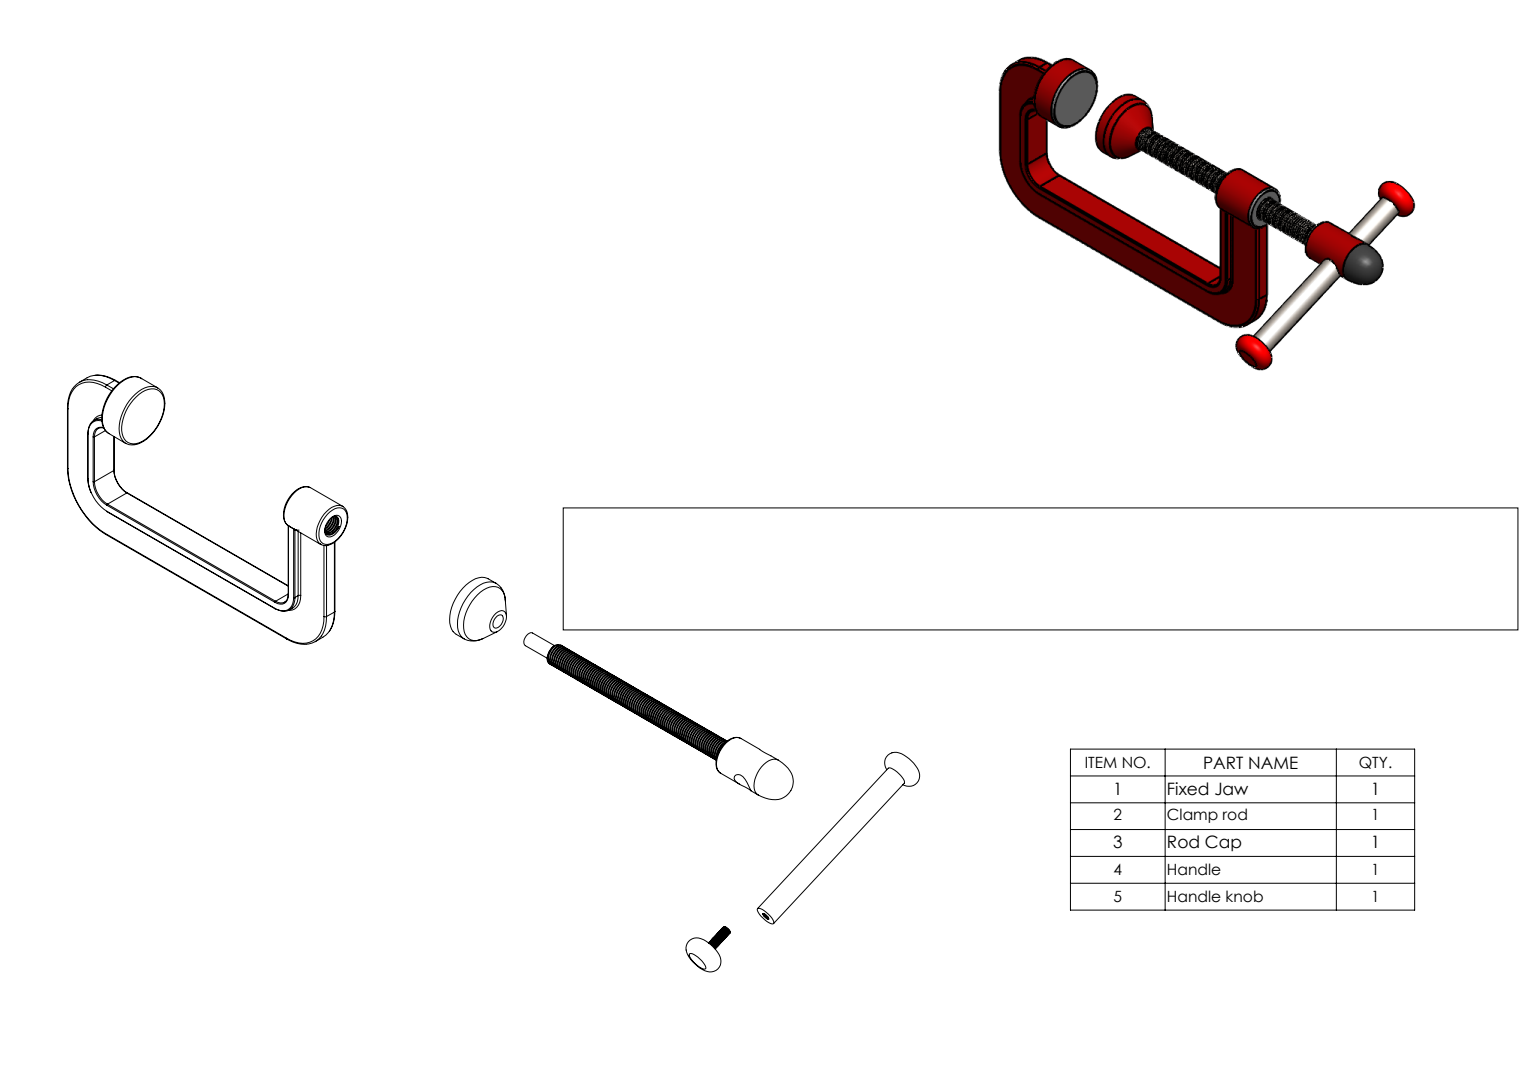
ISO-10303-21;
HEADER;
FILE_DESCRIPTION (('STEP AP214'),
    '1' );
FILE_NAME ('MAS-675',
    '2026-10-07T06:38:26',
    ( '' ),
    ( '' ),
    'SwSTEP 2.0',
    'SolidWorks 2021',
    '' );
FILE_SCHEMA (( 'AUTOMOTIVE_DESIGN' ));
ENDSEC;

DATA;
#1 = VERTEX_POINT ( 'NONE', #13580 ) ;
#2 = ORIENTED_EDGE ( 'NONE', *, *, #13115, .T. ) ;
#3 = CARTESIAN_POINT ( 'NONE',  ( 151.8675748654052029, -5.500000000000012434, 2.278174593052012309 ) ) ;
#4 = CARTESIAN_POINT ( 'NONE',  ( 134.2500000000000284, -6.000000000000005329, 0.000000000000000000 ) ) ;
#5 = ORIENTED_EDGE ( 'NONE', *, *, #19399, .F. ) ;
#6 = CARTESIAN_POINT ( 'NONE',  ( -5.412658773652684552, -3.125000000000099920, -143.0669872981078470 ) ) ;
#7 =( NAMED_UNIT ( * ) PLANE_ANGLE_UNIT ( ) SI_UNIT ( $, .RADIAN. ) );
#8 = CARTESIAN_POINT ( 'NONE',  ( 11.81249999999999822, -2.649519052838298805, 1.097466725451559322 ) ) ;
#9 = ADVANCED_FACE ( 'NONE', ( #19589 ), #12972, .F. ) ;
#10 = CARTESIAN_POINT ( 'NONE',  ( 5.999999999999999112, 2.951592740943527306E-14, -151.5863248654052029 ) ) ;
#11 = VECTOR ( 'NONE', #10192, 1000.000000000000000 ) ;
#12 = CARTESIAN_POINT ( 'NONE',  ( 18.18750000000005684, 0.8284271247463557142, 1.999999999999971800 ) ) ;
#13 = CARTESIAN_POINT ( 'NONE',  ( 3.464101615137757051, -5.999999999999979572, -171.3363248654052029 ) ) ;
#14 = CARTESIAN_POINT ( 'NONE',  ( 116.0000000000000142, 6.735557395310442023E-16, 5.500000000000000000 ) ) ;
#15 = CARTESIAN_POINT ( 'NONE',  ( -5.412658773652739619, 3.124999999999975131, -63.18301270189225249 ) ) ;
#16 = CARTESIAN_POINT ( 'NONE',  ( -5.999999999999963585, 1.780251999655701777E-13, -110.9136751345948255 ) ) ;
#17 = CARTESIAN_POINT ( 'NONE',  ( 143.2351497308104058, 3.535533905932725318, -3.535533905932725318 ) ) ;
#18 = DIRECTION ( 'NONE',  ( 1.000000000000000000, -5.551115123125774074E-17, 0.000000000000000000 ) ) ;
#19 = DIRECTION ( 'NONE',  ( -0.000000000000000000, -0.000000000000000000, -1.000000000000000000 ) ) ;
#20 = LINE ( 'NONE', #9560, #12153 ) ;
#21 = CYLINDRICAL_SURFACE ( 'NONE', #16144, 11.00000000000001599 ) ;
#22 = CARTESIAN_POINT ( 'NONE',  ( 112.1249999999998437, 1.767766952966293159, 1.767766952966431937 ) ) ;
#23 = EDGE_CURVE ( 'NONE', #18475, #14303, #3726, .T. ) ;
#24 = CARTESIAN_POINT ( 'NONE',  ( 15.64882486540532547, 2.500000000000084821, -1.035533905932929599 ) ) ;
#25 = DIRECTION ( 'NONE',  ( 0.000000000000000000, 0.000000000000000000, -1.000000000000000000 ) ) ;
#26 = EDGE_LOOP ( 'NONE', ( #21447, #18277, #20127, #3460 ) ) ;
#27 = CARTESIAN_POINT ( 'NONE',  ( -6.350852961085760029, -1.281975124255709124E-13, -55.12500000000003553 ) ) ;
#28 = DIRECTION ( 'NONE',  ( 1.000000000000000000, 0.000000000000000000, 0.000000000000000000 ) ) ;
#29 = CARTESIAN_POINT ( 'NONE',  ( 6.000000000000000888, -1.859271017917181981E-14, -167.1636751345948255 ) ) ;
#30 = CARTESIAN_POINT ( 'NONE',  ( -3.464101615137757051, -5.999999999999979572, -179.0863248654052313 ) ) ;
#31 = ORIENTED_EDGE ( 'NONE', *, *, #1535, .F. ) ;
#32 = CARTESIAN_POINT ( 'NONE',  ( 104.9374999999997726, 2.500000000000114575, -1.035533905932448873 ) ) ;
#33 = CARTESIAN_POINT ( 'NONE',  ( 142.6875000000000284, 4.242640687119269671, 4.242640687119298093 ) ) ;
#34 = CARTESIAN_POINT ( 'NONE',  ( -3.608439182435052128, -6.250000000000110134, -103.9419872981078328 ) ) ;
#35 = MECHANICAL_DESIGN_GEOMETRIC_PRESENTATION_REPRESENTATION (  '', ( #14770 ), #26040 ) ;
#36 = CARTESIAN_POINT ( 'NONE',  ( -3.464101615137725076, 5.999999999999979572, -176.5863248654052313 ) ) ;
#37 = VECTOR ( 'NONE', #4562, 1000.000000000000000 ) ;
#38 = CARTESIAN_POINT ( 'NONE',  ( 160.5788997308103774, -4.999999999999989342, 2.071067811865468400 ) ) ;
#39 = CARTESIAN_POINT ( 'NONE',  ( 118.3749999999999147, -1.767766952966293159, 1.767766952966431937 ) ) ;
#40 = CARTESIAN_POINT ( 'NONE',  ( 3.175426480543072749, -5.500000000000105693, -138.6250000000000568 ) ) ;
#41 = VECTOR ( 'NONE', #11597, 1000.000000000000000 ) ;
#42 = VERTEX_POINT ( 'NONE', #1381 ) ;
#43 = VECTOR ( 'NONE', #27184, 1000.000000000000000 ) ;
#44 = ORIENTED_EDGE ( 'NONE', *, *, #20112, .T. ) ;
#45 =( NAMED_UNIT ( * ) PLANE_ANGLE_UNIT ( ) SI_UNIT ( $, .RADIAN. ) );
#46 = EDGE_CURVE ( 'NONE', #22177, #19788, #18313, .T. ) ;
#47 = CARTESIAN_POINT ( 'NONE',  ( -3.175426480542816510, -5.500000000000057732, -66.87500000000002842 ) ) ;
#48 = CARTESIAN_POINT ( 'NONE',  ( 0.000000000000000000, -5.999999999999991118, -81.46132486540524553 ) ) ;
#49 = CARTESIAN_POINT ( 'NONE',  ( 159.6411875853270885, -12.17723633016814233, -3.777793391642500165 ) ) ;
#50 = CARTESIAN_POINT ( 'NONE',  ( 3.608439182435180470, 6.249999999999982236, -80.05801270189219565 ) ) ;
#51 = CARTESIAN_POINT ( 'NONE',  ( 5.196152422706629359, 3.000000000000002665, -140.0386751345948255 ) ) ;
#52 = CARTESIAN_POINT ( 'NONE',  ( 106.7497167782375129, 1.308140751793612777, 1.308140751793529510 ) ) ;
#53 = DIRECTION ( 'NONE',  ( -1.000000000000000000, -0.000000000000000000, -0.000000000000000000 ) ) ;
#54 = VECTOR ( 'NONE', #17424, 1000.000000000000000 ) ;
#55 = CARTESIAN_POINT ( 'NONE',  ( 119.3127832217621034, 1.849990392679501827, -0.7662911109077087390 ) ) ;
#56 = ADVANCED_FACE ( 'NONE', ( #10625 ), #5822, .T. ) ;
#57 = CONTEXT_DEPENDENT_SHAPE_REPRESENTATION ( #15191, #20980 ) ;
#58 =( BOUNDED_CURVE ( )  B_SPLINE_CURVE ( 2, ( #3111, #10057, #5114, #12242, #12386, #512, #17135, #26164, #2819 ),
 .UNSPECIFIED., .F., .T. ) 
 B_SPLINE_CURVE_WITH_KNOTS ( ( 3, 2, 2, 2, 3 ),
 ( 0.05277777777777781232, 0.05370370370370369795, 0.05555555555555558023, 0.05740740740740746251, 0.05833333333333334814 ),
 .UNSPECIFIED. ) 
 CURVE ( )  GEOMETRIC_REPRESENTATION_ITEM ( )  RATIONAL_B_SPLINE_CURVE ( ( 0.9330127018922194093, 0.9330127018922234061, 1.000000000000000000, 0.8660254037844388186, 1.000000000000000000, 0.8660254037844388186, 1.000000000000000000, 0.9330127018922194093, 0.9330127018922194093 ) ) 
 REPRESENTATION_ITEM ( '' )  );
#59 = CARTESIAN_POINT ( 'NONE',  ( 4.763139720814407951, -2.749999999999988454, -149.0000000000000284 ) ) ;
#60 = CARTESIAN_POINT ( 'NONE',  ( 139.5760635317500089, -9.165151396444613852, -8.000000000000007105 ) ) ;
#61 = CARTESIAN_POINT ( 'NONE',  ( 3.175426480543072749, -5.500000000000105693, -138.6250000000000568 ) ) ;
#62 = CARTESIAN_POINT ( 'NONE',  ( 3.608439182435180470, 6.249999999999982236, -164.0580127018922383 ) ) ;
#63 = CARTESIAN_POINT ( 'NONE',  ( 0.000000000000000000, -5.999999999999991118, -148.9613248654052597 ) ) ;
#64 = DIRECTION ( 'NONE',  ( 6.938893903907222067E-15, 1.000000000000000000, 0.000000000000000000 ) ) ;
#65 = CARTESIAN_POINT ( 'NONE',  ( 6.350852961086080661, -9.614813431917819062E-14, -76.87500000000002842 ) ) ;
#66 = FILL_AREA_STYLE ('',( #23440 ) ) ;
#67 = CARTESIAN_POINT ( 'NONE',  ( -4.763139720814407951, 2.749999999999946709, -62.75000000000002842 ) ) ;
#68 = CARTESIAN_POINT ( 'NONE',  ( -5.196152422706601826, 2.999999999999975131, -154.5386751345948539 ) ) ;
#69 = CARTESIAN_POINT ( 'NONE',  ( 145.1398502691896510, -3.535533905932752852, 3.535533905932725318 ) ) ;
#70 = CARTESIAN_POINT ( 'NONE',  ( 3.464101615137757051, -5.999999999999979572, -114.3363248654051745 ) ) ;
#71 = CARTESIAN_POINT ( 'NONE',  ( -5.196152422706573404, -3.000000000000002665, -144.7113248654052313 ) ) ;
#72 = CARTESIAN_POINT ( 'NONE',  ( 157.4062500000000284, 6.000000000000005329, -2.485281374238556218 ) ) ;
#73 = DIRECTION ( 'NONE',  ( 5.551115123125785167E-17, -1.000000000000000000, -8.881784197001256268E-16 ) ) ;
#74 = CARTESIAN_POINT ( 'NONE',  ( -3.464101615137757051, -5.999999999999979572, -50.08632486540522422 ) ) ;
#75 = CARTESIAN_POINT ( 'NONE',  ( 6.000000000000000888, -3.330669073875464691E-16, -7.560779664488942560E-35 ) ) ;
#76 = CARTESIAN_POINT ( 'NONE',  ( 116.5622167782374135, 1.849990392679562001, -0.7662911109077087390 ) ) ;
#77 = DIRECTION ( 'NONE',  ( 1.000000000000000000, 0.000000000000000000, 0.000000000000000000 ) ) ;
#78 = ORIENTED_EDGE ( 'NONE', *, *, #7844, .T. ) ;
#79 = CARTESIAN_POINT ( 'NONE',  ( 150.3750000000000284, 0.000000000000000000, 6.000000000000005329 ) ) ;
#80 = SURFACE_SIDE_STYLE ('',( #6693 ) ) ;
#81 = CARTESIAN_POINT ( 'NONE',  ( 115.7502832217623308, -1.308140751793585022, 1.308140751793640533 ) ) ;
#82 = CARTESIAN_POINT ( 'NONE',  ( -3.464101615137757051, -5.999999999999979572, -85.16367513459481131 ) ) ;
#83 = ORIENTED_EDGE ( 'NONE', *, *, #26629, .F. ) ;
#84 = VERTEX_POINT ( 'NONE', #7829 ) ;
#85 = CARTESIAN_POINT ( 'NONE',  ( 19.25000000000009948, 1.110223024625156540E-13, 1.999999999999946265 ) ) ;
#86 = VECTOR ( 'NONE', #24008, 1000.000000000000114 ) ;
#87 = VERTEX_POINT ( 'NONE', #29166 ) ;
#88 = EDGE_CURVE ( 'NONE', #16343, #27983, #2946, .T. ) ;
#89 = CARTESIAN_POINT ( 'NONE',  ( -6.350852961085760029, -1.281975124255709124E-13, -91.12500000000001421 ) ) ;
#90 = CARTESIAN_POINT ( 'NONE',  ( -7.216878364870328078, 0.000000000000000000, -106.5580127018922525 ) ) ;
#91 = VERTEX_POINT ( 'NONE', #21836 ) ;
#92 = CARTESIAN_POINT ( 'NONE',  ( 5.959413262067462469, 9.246315551493085039, -24.19612909832622449 ) ) ;
#93 = CARTESIAN_POINT ( 'NONE',  ( 156.4538997308104626, -2.071067811865468400, -4.999999999999989342 ) ) ;
#94 = CIRCLE ( 'NONE', #6471, 2.000000000000003109 ) ;
#95 = CARTESIAN_POINT ( 'NONE',  ( 3.464101615137757051, -5.999999999999979572, -63.33632486540521711 ) ) ;
#96 = CARTESIAN_POINT ( 'NONE',  ( 135.6737246954180023, -8.728829995094853800, 8.172675940893835644 ) ) ;
#97 = ADVANCED_FACE ( 'NONE', ( #784 ), #22288, .T. ) ;
#98 = ADVANCED_FACE ( 'NONE', ( #17543 ), #26707, .F. ) ;
#99 = CARTESIAN_POINT ( 'NONE',  ( 4.763139720814407951, 2.750000000000002665, -169.7500000000000000 ) ) ;
#100 = CARTESIAN_POINT ( 'NONE',  ( 23.03867513459492855, 2.220446049250313081E-13, -2.500000000000057732 ) ) ;
#101 = STYLED_ITEM ( 'NONE', ( #7132 ), #3790 ) ;
#102 = CARTESIAN_POINT ( 'NONE',  ( -4.763139720814407951, 2.749999999999946709, -151.2500000000000000 ) ) ;
#103 = SHAPE_REPRESENTATION ( 'MAS-675', ( #12959, #2139, #10996, #7044, #27128, #21262 ), #2611 ) ;
#104 = CARTESIAN_POINT ( 'NONE',  ( 112.4374999999998010, -2.499999999999934719, 1.035533905932989551 ) ) ;
#105 = AXIS2_PLACEMENT_3D ( 'NONE', #8951, #27958, #28266 ) ;
#106 = CARTESIAN_POINT ( 'NONE',  ( -2.775557561562891351E-14, -5.500000000000115463, -101.2500000000000000 ) ) ;
#107 = CARTESIAN_POINT ( 'NONE',  ( 135.0000000000000284, -54.99999999999993605, -7.500000000000007105 ) ) ;
#108 = CARTESIAN_POINT ( 'NONE',  ( 125.0000000000000568, -55.00000000000000711, -7.500000000000007105 ) ) ;
#110 = CARTESIAN_POINT ( 'NONE',  ( -3.175426480542816510, 5.499999999999865885, -86.87500000000007105 ) ) ;
#109 = CARTESIAN_POINT ( 'NONE',  ( 3.175426480543072749, 5.499999999999865885, -154.6250000000000853 ) ) ;
#111 = CARTESIAN_POINT ( 'NONE',  ( 161.5461002691896226, -2.071067811865468400, 4.999999999999989342 ) ) ;
#112 = CARTESIAN_POINT ( 'NONE',  ( 0.7724517649218355375, -15.49026069396310490, 8.142614232235679594 ) ) ;
#113 = ORIENTED_EDGE ( 'NONE', *, *, #22581, .F. ) ;
#114 = CARTESIAN_POINT ( 'NONE',  ( 9.937500000000083489, -1.097466725451379244, 2.649519052838238409 ) ) ;
#115 = UNCERTAINTY_MEASURE_WITH_UNIT (LENGTH_MEASURE( 1.000000000000000082E-05 ), #12056, 'distance_accuracy_value', 'NONE');
#116 = CARTESIAN_POINT ( 'NONE',  ( 114.5624999999997442, -2.499999999999934719, -1.035533905932448873 ) ) ;
#117 = CARTESIAN_POINT ( 'NONE',  ( -4.999999999999990230, -55.00000000000002132, 5.000000000000004441 ) ) ;
#118 = CARTESIAN_POINT ( 'NONE',  ( 106.5627832217621602, 0.7662911109078588412, 1.849990392679712103 ) ) ;
#119 = CARTESIAN_POINT ( 'NONE',  ( 23.66367513459491434, -1.767766952966209892, 1.767766952966376426 ) ) ;
#120 = ORIENTED_EDGE ( 'NONE', *, *, #127, .F. ) ;
#121 = DIRECTION ( 'NONE',  ( 0.000000000000000000, 0.000000000000000000, -1.000000000000000000 ) ) ;
#122 = DIRECTION ( 'NONE',  ( -7.147005652999508048E-36, 5.642372883946980038E-36, 1.000000000000000000 ) ) ;
#123 = ORIENTED_EDGE ( 'NONE', *, *, #24115, .F. ) ;
#124 = VERTEX_POINT ( 'NONE', #14929 ) ;
#125 = CARTESIAN_POINT ( 'NONE',  ( 151.9687500000000568, -2.485281374238585972, 6.000000000000005329 ) ) ;
#126 = ORIENTED_EDGE ( 'NONE', *, *, #11372, .T. ) ;
#127 = EDGE_CURVE ( 'NONE', #21812, #1827, #10033, .T. ) ;
#128 = CARTESIAN_POINT ( 'NONE',  ( 4.763139720814407951, -2.749999999999988454, -109.9999999999999858 ) ) ;
#129 = CARTESIAN_POINT ( 'NONE',  ( 21.62500000000011724, 1.110223024625156540E-13, 2.649519052838167354 ) ) ;
#130 = CARTESIAN_POINT ( 'NONE',  ( 3.175426480543072749, -5.500000000000105693, -150.6250000000000284 ) ) ;
#131 = CARTESIAN_POINT ( 'NONE',  ( -5.412658773652684552, -3.125000000000099920, -130.4330127018922383 ) ) ;
#132 = ORIENTED_EDGE ( 'NONE', *, *, #22296, .F. ) ;
#133 = CARTESIAN_POINT ( 'NONE',  ( 0.000000000000000000, 0.000000000000000000, 0.000000000000000000 ) ) ;
#134 = CARTESIAN_POINT ( 'NONE',  ( 3.608439182435180470, -6.249999999999997335, -171.1919872981078470 ) ) ;
#135 = CARTESIAN_POINT ( 'NONE',  ( 107.1249999999998437, 1.767766952966265404, 1.767766952966320915 ) ) ;
#136 = CARTESIAN_POINT ( 'NONE',  ( 134.2351497308104058, 3.535533905932725318, -3.535533905932725318 ) ) ;
#137 = VERTEX_POINT ( 'NONE', #1215 ) ;
#138 = CARTESIAN_POINT ( 'NONE',  ( 0.1879814459054835185, -15.40071801525260220, -8.313003687118166951 ) ) ;
#139 = ADVANCED_FACE ( 'NONE', ( #915 ), #19679, .F. ) ;
#140 = COLOUR_RGB ( '', 0.31764706, 0.68627451, 0.89019608) ;
#141 = CARTESIAN_POINT ( 'NONE',  ( -3.464101615137725076, 5.999999999999979572, -95.58632486540524553 ) ) ;
#142 = CYLINDRICAL_SURFACE ( 'NONE', #25085, 0.5000000000000004441 ) ;
#143 = CARTESIAN_POINT ( 'NONE',  ( -2.775557561562891351E-14, -5.500000000000115463, -180.7500000000000284 ) ) ;
#144 = CARTESIAN_POINT ( 'NONE',  ( 108.6877832217621318, -0.7662911109077388261, 1.849990392679712103 ) ) ;
#145 = CARTESIAN_POINT ( 'NONE',  ( -5.412658773652739619, 3.124999999999975131, -178.6830127018922383 ) ) ;
#146 = CARTESIAN_POINT ( 'NONE',  ( -0.5130136762305975706, -9.973972647538804637, -4.738252045315842764 ) ) ;
#147 = CARTESIAN_POINT ( 'NONE',  ( 159.9897649647779474, -11.17313463120727057, -4.377898023955410167 ) ) ;
#148 = UNCERTAINTY_MEASURE_WITH_UNIT (LENGTH_MEASURE( 1.000000000000000082E-05 ), #22122, 'distance_accuracy_value', 'NONE');
#149 = CARTESIAN_POINT ( 'NONE',  ( -6.350852961085760029, -1.281975124255709124E-13, -113.6249999999999858 ) ) ;
#150 = CARTESIAN_POINT ( 'NONE',  ( 135.0000000000000284, -8.662311887307041047, -7.546725650337192448 ) ) ;
#151 = CARTESIAN_POINT ( 'NONE',  ( 154.1175748654052313, 5.500000000000012434, -2.278174593052012309 ) ) ;
#152 = VERTEX_POINT ( 'NONE', #29328 ) ;
#153 = CARTESIAN_POINT ( 'NONE',  ( 21.25000000000013145, -1.873492889144845464, -1.873492889145178530 ) ) ;
#154 = DIRECTION ( 'NONE',  ( -7.147005652999508048E-36, 5.642372883946980038E-36, 1.000000000000000000 ) ) ;
#155 = CARTESIAN_POINT ( 'NONE',  ( 6.000000000000000888, 1.607695154586715303, -168.5966878364870354 ) ) ;
#156 = CARTESIAN_POINT ( 'NONE',  ( 5.196152422706629359, 3.000000000000002665, -131.9613248654052313 ) ) ;
#157 =( BOUNDED_CURVE ( )  B_SPLINE_CURVE ( 2, ( #10782, #15865, #1831, #11235, #29931, #22280, #26855, #27319, #5814 ),
 .UNSPECIFIED., .F., .T. ) 
 B_SPLINE_CURVE_WITH_KNOTS ( ( 3, 2, 2, 2, 3 ),
 ( 0.6750000000000000444, 0.6759259259259259300, 0.6777777777777778123, 0.6796296296296295836, 0.6805555555555554692 ),
 .UNSPECIFIED. ) 
 CURVE ( )  GEOMETRIC_REPRESENTATION_ITEM ( )  RATIONAL_B_SPLINE_CURVE ( ( 0.9330127018922194093, 0.9330127018922234061, 1.000000000000000000, 0.8660254037844388186, 1.000000000000000000, 0.8660254037844388186, 1.000000000000000000, 0.9330127018922234061, 0.9330127018922194093 ) ) 
 REPRESENTATION_ITEM ( '' )  );
#158 = AXIS2_PLACEMENT_3D ( 'NONE', #25640, #4289, #30093 ) ;
#159 = EDGE_LOOP ( 'NONE', ( #11290, #9356, #28132, #17982 ) ) ;
#160 = CARTESIAN_POINT ( 'NONE',  ( 118.4613248654051034, 1.110223024625156540E-13, -2.000000000000001776 ) ) ;
#161 = CARTESIAN_POINT ( 'NONE',  ( 22.21132486540528106, -2.499999999999780176, -1.110223024625156540E-13 ) ) ;
#162 = CARTESIAN_POINT ( 'NONE',  ( 142.5863248654052313, 0.000000000000000000, 5.500000000000005329 ) ) ;
#163 = CARTESIAN_POINT ( 'NONE',  ( 113.2113248654051034, -1.999999999999918510, 1.110223024625156540E-13 ) ) ;
#164 = ORIENTED_EDGE ( 'NONE', *, *, #27531, .F. ) ;
#165 = ORIENTED_EDGE ( 'NONE', *, *, #8341, .F. ) ;
#166 = CARTESIAN_POINT ( 'NONE',  ( 20.85117513459493921, -2.499999999999844569, -1.035533905932809473 ) ) ;
#167 = CARTESIAN_POINT ( 'NONE',  ( 135.1875000000000568, 4.242640687119269671, 4.242640687119298093 ) ) ;
#168 = EDGE_CURVE ( 'NONE', #2390, #1119, #5990, .T. ) ;
#169 = ADVANCED_FACE ( 'NONE', ( #22749 ), #29791, .T. ) ;
#170 = CARTESIAN_POINT ( 'NONE',  ( 3.608439182435180470, -6.249999999999997335, -141.1919872981078186 ) ) ;
#171 = CARTESIAN_POINT ( 'NONE',  ( -4.999999999999920952, -65.50000000000001421, -8.000000000000007105 ) ) ;
#172 =( NAMED_UNIT ( * ) PLANE_ANGLE_UNIT ( ) SI_UNIT ( $, .RADIAN. ) );
#173 = CARTESIAN_POINT ( 'NONE',  ( 19.75000000000009948, 1.665334536937734811E-13, -2.000000000000001776 ) ) ;
#174 = CARTESIAN_POINT ( 'NONE',  ( 117.7261751345945413, -1.999999999999971800, 0.8284271247464157772 ) ) ;
#175 = CIRCLE ( 'NONE', #14898, 0.5000000000000004441 ) ;
#176 = CARTESIAN_POINT ( 'NONE',  ( 144.5476497308104058, 0.000000000000000000, -5.000000000000004441 ) ) ;
#177 = CYLINDRICAL_SURFACE ( 'NONE', #16338, 6.000000000000000888 ) ;
#178 = CARTESIAN_POINT ( 'NONE',  ( 13.03867513459488947, 5.551115123125782702E-14, -2.500000000000002220 ) ) ;
#179 = CARTESIAN_POINT ( 'NONE',  ( 3.464101615137852974, 5.999999999999884537, -146.8363248654052313 ) ) ;
#180 = AXIS2_PLACEMENT_3D ( 'NONE', #24945, #8684, #29090 ) ;
#181 = CARTESIAN_POINT ( 'NONE',  ( 114.2886751345947971, 2.000000000000029310, 1.110223024625156540E-13 ) ) ;
#182 = CARTESIAN_POINT ( 'NONE',  ( 110.6249999999998437, -1.767766952966376426, -1.767766952966320915 ) ) ;
#183 = ORIENTED_EDGE ( 'NONE', *, *, #15487, .T. ) ;
#184 = CARTESIAN_POINT ( 'NONE',  ( -4.763139720814407951, -2.750000000000016431, -58.00000000000004974 ) ) ;
#185 = DIRECTION ( 'NONE',  ( 0.000000000000000000, 0.000000000000000000, 1.000000000000000000 ) ) ;
#186 = CYLINDRICAL_SURFACE ( 'NONE', #12466, 6.000000000000000888 ) ;
#187 = ORIENTED_EDGE ( 'NONE', *, *, #6959, .T. ) ;
#188 = CARTESIAN_POINT ( 'NONE',  ( 117.8122167782374135, 0.7662911109077388261, 1.849990392679832230 ) ) ;
#189 = CARTESIAN_POINT ( 'NONE',  ( 139.2187500000000284, 2.485281374238556218, -6.000000000000005329 ) ) ;
#190 = CARTESIAN_POINT ( 'NONE',  ( -7.216878364870328078, 0.000000000000000000, -99.69198729810781856 ) ) ;
#191 = DIRECTION ( 'NONE',  ( -0.000000000000000000, 1.000000000000000000, -0.000000000000000000 ) ) ;
#192 = CARTESIAN_POINT ( 'NONE',  ( 132.8437500000000284, -6.000000000000005329, -2.485281374238555774 ) ) ;
#193 = COLOUR_RGB ( '', 0.31764706, 0.68627451, 0.89019608) ;
#194 = CARTESIAN_POINT ( 'NONE',  ( -4.763139720814407951, 2.749999999999946709, -128.7500000000000284 ) ) ;
#195 = EDGE_CURVE ( 'NONE', #1664, #6421, #4446, .T. ) ;
#196 = EDGE_LOOP ( 'NONE', ( #23554, #27384, #25817, #24929 ) ) ;
#197 = EDGE_LOOP ( 'NONE', ( #23745, #2064, #9008, #12960 ) ) ;
#198 = CARTESIAN_POINT ( 'NONE',  ( 6.000000000000052403, 1.607695154586625819, -163.5193375672974128 ) ) ;
#199 = CARTESIAN_POINT ( 'NONE',  ( 0.000000000000000000, 5.499999999999991118, -67.50000000000000000 ) ) ;
#200 = CARTESIAN_POINT ( 'NONE',  ( -19.99999999999998224, -25.00000000000010658, -5.000000000000004441 ) ) ;
#201 = CARTESIAN_POINT ( 'NONE',  ( 2.775557561562891351E-14, 6.250000000000033751, -84.43301270189223828 ) ) ;
#202 = CARTESIAN_POINT ( 'NONE',  ( 6.000000000000000888, -3.330669073875464691E-16, -7.560779664488942560E-35 ) ) ;
#203 = CARTESIAN_POINT ( 'NONE',  ( 6.000000000000000888, 1.743066579297358182E-13, -113.1636751345948397 ) ) ;
#204 = CARTESIAN_POINT ( 'NONE',  ( 104.5622167782374703, 1.849990392679501827, -0.7662911109076485650 ) ) ;
#205 = FACE_OUTER_BOUND ( 'NONE', #29290, .T. ) ;
#206 = CARTESIAN_POINT ( 'NONE',  ( 119.3752832217622313, 1.849990392679523588, 0.000000000000000000 ) ) ;
#207 = ITEM_DEFINED_TRANSFORMATION ( 'NONE', 'NONE', #21262,  #18805 ) ;
#208 = CARTESIAN_POINT ( 'NONE',  ( -3.175426480542816066, -5.500000000000057732, -144.8750000000000853 ) ) ;
#209 = CARTESIAN_POINT ( 'NONE',  ( 5.196152422706629359, -2.999999999999988898, -105.2113248654052455 ) ) ;
#210 = CARTESIAN_POINT ( 'NONE',  ( 3.608439182435180470, -6.249999999999997335, -155.5580127018922383 ) ) ;
#211 = DIRECTION ( 'NONE',  ( 1.000000000000000000, -5.551115123125773458E-17, -1.260129944081490338E-35 ) ) ;
#212 = DIRECTION ( 'NONE',  ( 1.000000000000000000, -5.551115123125774074E-17, 0.000000000000000000 ) ) ;
#213 = CARTESIAN_POINT ( 'NONE',  ( -4.763139720814407951, 2.749999999999946709, -82.25000000000004263 ) ) ;
#214 = CARTESIAN_POINT ( 'NONE',  ( 5.999999999999974243, 1.607695154586759934, -132.5966878364870354 ) ) ;
#215 = CARTESIAN_POINT ( 'NONE',  ( -6.350852961085760029, -1.281975124255709124E-13, -67.12500000000002842 ) ) ;
#216 = CARTESIAN_POINT ( 'NONE',  ( -5.999999999999971578, 1.607695154586715303, -154.4806624327026157 ) ) ;
#217 = CARTESIAN_POINT ( 'NONE',  ( 145.0461002691896510, -2.071067811865468400, 4.999999999999989342 ) ) ;
#218 = CARTESIAN_POINT ( 'NONE',  ( 0.000000000000000000, 0.000000000000000000, 0.000000000000000000 ) ) ;
#219 = CARTESIAN_POINT ( 'NONE',  ( 157.2187500000000284, 2.485281374238556218, -6.000000000000005329 ) ) ;
#220 = CARTESIAN_POINT ( 'NONE',  ( 16.37500000000008527, -1.414213562373090038, 1.414213562373034527 ) ) ;
#221 = EDGE_CURVE ( 'NONE', #23969, #26551, #13207, .T. ) ;
#222 = CARTESIAN_POINT ( 'NONE',  ( 6.000000000000000888, 1.743066579297358182E-13, -49.58632486540520290 ) ) ;
#223 = FACE_OUTER_BOUND ( 'NONE', #11618, .T. ) ;
#224 = CARTESIAN_POINT ( 'NONE',  ( 116.4372167782373850, 0.7662911109078588412, -1.849990392679411677 ) ) ;
#225 = DIRECTION ( 'NONE',  ( -7.147005652999508048E-36, 5.642372883946980038E-36, 1.000000000000000000 ) ) ;
#226 = VERTEX_POINT ( 'NONE', #20904 ) ;
#227 = CARTESIAN_POINT ( 'NONE',  ( 149.4375000000000284, -4.242640687119298093, -4.242640687119298093 ) ) ;
#228 = CARTESIAN_POINT ( 'NONE',  ( 114.8752832217623165, -1.849990392679523588, 0.000000000000000000 ) ) ;
#229 = CARTESIAN_POINT ( 'NONE',  ( -5.999999999999963585, 1.780251999655701777E-13, -62.91367513459483973 ) ) ;
#230 =( BOUNDED_CURVE ( )  B_SPLINE_CURVE ( 2, ( #16660, #4488, #23098, #2488, #25984, #326, #16513, #12052, #16065 ),
 .UNSPECIFIED., .F., .T. ) 
 B_SPLINE_CURVE_WITH_KNOTS ( ( 3, 2, 2, 2, 3 ),
 ( 0.5083333333333334147, 0.5092592592592593004, 0.5111111111111110716, 0.5129629629629629539, 0.5138888888888888395 ),
 .UNSPECIFIED. ) 
 CURVE ( )  GEOMETRIC_REPRESENTATION_ITEM ( )  RATIONAL_B_SPLINE_CURVE ( ( 0.9330127018922194093, 0.9330127018922234061, 1.000000000000000000, 0.8660254037844388186, 1.000000000000000000, 0.8660254037844388186, 1.000000000000000000, 0.9330127018922234061, 0.9330127018922194093 ) ) 
 REPRESENTATION_ITEM ( '' )  );
#231 = ADVANCED_FACE ( 'NONE', ( #13556 ), #6599, .F. ) ;
#232 = CARTESIAN_POINT ( 'NONE',  ( 22.87500000000000711, 1.414213562373312083, -1.414213562373090038 ) ) ;
#233 = CARTESIAN_POINT ( 'NONE',  ( 2.775557561562891351E-14, -6.250000000000061284, -151.8169872981078186 ) ) ;
#234 = VERTEX_POINT ( 'NONE', #29941 ) ;
#235 = CARTESIAN_POINT ( 'NONE',  ( -2.775557561562891351E-14, -5.500000000000115463, -87.75000000000000000 ) ) ;
#236 = CARTESIAN_POINT ( 'NONE',  ( -5.412658773652684552, -3.125000000000099920, -100.4330127018922525 ) ) ;
#237 =( BOUNDED_CURVE ( )  B_SPLINE_CURVE ( 2, ( #7992, #5676, #24577, #27183, #10633, #12799, #20145, #15086, #3680 ),
 .UNSPECIFIED., .F., .F. ) 
 B_SPLINE_CURVE_WITH_KNOTS ( ( 3, 2, 2, 2, 3 ),
 ( 0.5416666666666667407, 0.5425925925925925153, 0.5444444444444445086, 0.5462962962962962798, 0.5472222222222222765 ),
 .UNSPECIFIED. ) 
 CURVE ( )  GEOMETRIC_REPRESENTATION_ITEM ( )  RATIONAL_B_SPLINE_CURVE ( ( 0.9330127018922194093, 0.9330127018922274029, 1.000000000000000000, 0.8660254037844388186, 1.000000000000000000, 0.8660254037844388186, 1.000000000000000000, 0.9330127018922154125, 0.9330127018922194093 ) ) 
 REPRESENTATION_ITEM ( '' )  );
#238 = ORIENTED_EDGE ( 'NONE', *, *, #23310, .F. ) ;
#239 = CARTESIAN_POINT ( 'NONE',  ( 154.6726497308104058, -5.000000000000004441, 0.000000000000000000 ) ) ;
#240 = CARTESIAN_POINT ( 'NONE',  ( 3.175426480543072749, -5.500000000000105693, -167.1250000000000000 ) ) ;
#241 = CARTESIAN_POINT ( 'NONE',  ( -5.999999999999962697, 3.323446944526963891E-14, -155.3363248654052313 ) ) ;
#242 = DIRECTION ( 'NONE',  ( 1.000000000000000000, -0.000000000000000000, -0.000000000000000000 ) ) ;
#243 = CARTESIAN_POINT ( 'NONE',  ( -5.999999999999963585, 1.780251999655701777E-13, -68.33632486540521711 ) ) ;
#244 = CARTESIAN_POINT ( 'NONE',  ( 6.350852961086080661, -9.614813431917819062E-14, -175.8750000000000284 ) ) ;
#245 = LINE ( 'NONE', #5439, #2253 ) ;
#246 = AXIS2_PLACEMENT_3D ( 'NONE', #9140, #8524, #18081 ) ;
#247 = CARTESIAN_POINT ( 'NONE',  ( -6.350852961085760029, -1.281975124255709124E-13, -158.6250000000000284 ) ) ;
#248 = CARTESIAN_POINT ( 'NONE',  ( 113.0624999999997726, 2.500000000000084821, 1.035533905932989551 ) ) ;
#249 = CARTESIAN_POINT ( 'NONE',  ( 0.000000000000000000, -5.999999999999991118, -103.9613248654052171 ) ) ;
#250 = AXIS2_PLACEMENT_3D ( 'NONE', #6454, #4145, #24741 ) ;
#251 = CARTESIAN_POINT ( 'NONE',  ( 6.350852961086080661, -9.614813431917819062E-14, -100.8749999999999858 ) ) ;
#252 = DIRECTION ( 'NONE',  ( 1.000000000000000000, 0.000000000000000000, 0.000000000000000000 ) ) ;
#253 = CARTESIAN_POINT ( 'NONE',  ( 144.7574251345947687, -2.278174593051733421, 5.500000000000292211 ) ) ;
#255 = CARTESIAN_POINT ( 'NONE',  ( 0.000000000000000000, 5.499999999999991118, -87.00000000000002842 ) ) ;
#254 = CARTESIAN_POINT ( 'NONE',  ( 0.000000000000000000, 5.499999999999991118, -156.0000000000000284 ) ) ;
#256 = CARTESIAN_POINT ( 'NONE',  ( 13.83632486540523132, 1.767766952966376426, 1.767766952966376426 ) ) ;
#257 = CARTESIAN_POINT ( 'NONE',  ( 156.7648502691896510, 3.535533905932725318, 3.535533905932752852 ) ) ;
#258 = CARTESIAN_POINT ( 'NONE',  ( 124.9999999999999432, -65.00000000000000000, -7.500000000000007105 ) ) ;
#259 = ORIENTED_EDGE ( 'NONE', *, *, #5614, .F. ) ;
#260 = CARTESIAN_POINT ( 'NONE',  ( 23.37500000000000711, -1.414213562373090038, 1.414213562373034527 ) ) ;
#261 = CARTESIAN_POINT ( 'NONE',  ( 111.3124999999998295, -1.035533905932629173, 2.500000000000325517 ) ) ;
#262 = EDGE_CURVE ( 'NONE', #25850, #8065, #1532, .T. ) ;
#263 = CARTESIAN_POINT ( 'NONE',  ( 106.6877832217621602, -0.7662911109076785410, 1.849990392679712103 ) ) ;
#264 = LINE ( 'NONE', #7761, #2214 ) ;
#265 = ORIENTED_EDGE ( 'NONE', *, *, #5075, .F. ) ;
#266 = VECTOR ( 'NONE', #18330, 1000.000000000000000 ) ;
#267 = FACE_OUTER_BOUND ( 'NONE', #28986, .T. ) ;
#268 = DIRECTION ( 'NONE',  ( 1.000000000000000000, -5.551115123125773458E-17, -1.260129944081490338E-35 ) ) ;
#269 = VERTEX_POINT ( 'NONE', #30248 ) ;
#270 = EDGE_CURVE ( 'NONE', #5714, #18702, #21431, .T. ) ;
#271 = EDGE_CURVE ( 'NONE', #137, #4894, #411, .T. ) ;
#272 = ORIENTED_EDGE ( 'NONE', *, *, #28675, .F. ) ;
#273 = CARTESIAN_POINT ( 'NONE',  ( 153.4687500000000853, -2.485281374238585972, 6.000000000000005329 ) ) ;
#274 = STYLED_ITEM ( 'NONE', ( #25687 ), #21644 ) ;
#275 = CARTESIAN_POINT ( 'NONE',  ( 4.763139720814407951, -2.749999999999988454, -111.5000000000000426 ) ) ;
#276 = CARTESIAN_POINT ( 'NONE',  ( 19.25000000000009948, 1.873492889145067508, -1.873492889144956486 ) ) ;
#277 = CARTESIAN_POINT ( 'NONE',  ( -7.216878364870328078, 0.000000000000000000, -123.0580127018922667 ) ) ;
#278 = VERTEX_POINT ( 'NONE', #29639 ) ;
#279 = CARTESIAN_POINT ( 'NONE',  ( 116.0000000000000142, 0.000000000000000000, 0.000000000000000000 ) ) ;
#280 = CARTESIAN_POINT ( 'NONE',  ( 5.412658773652712085, -3.125000000000086153, -171.0669872981078186 ) ) ;
#281 = CARTESIAN_POINT ( 'NONE',  ( 106.5624999999998295, -2.499999999999874767, -1.035533905932629173 ) ) ;
#282 = CARTESIAN_POINT ( 'NONE',  ( -5.999999999999963585, 1.780251999655701777E-13, -95.91367513459483973 ) ) ;
#283 = VERTEX_POINT ( 'NONE', #9216 ) ;
#284 = CARTESIAN_POINT ( 'NONE',  ( 1.170107792545981740, 5.489964307952348577, -180.0000000000000000 ) ) ;
#285 = CARTESIAN_POINT ( 'NONE',  ( 6.000000000000052403, 1.607695154586625819, -138.0193375672974128 ) ) ;
#286 = CARTESIAN_POINT ( 'NONE',  ( 3.175426480543072749, -5.500000000000105693, -176.1250000000000284 ) ) ;
#287 = CARTESIAN_POINT ( 'NONE',  ( 108.0002832217622597, -1.308140751793585022, -1.308140751793640533 ) ) ;
#288 = CARTESIAN_POINT ( 'NONE',  ( 5.412658773652712085, -3.125000000000086153, -173.4330127018922667 ) ) ;
#289 = SURFACE_SIDE_STYLE ('',( #7647 ) ) ;
#290 = CARTESIAN_POINT ( 'NONE',  ( 6.000000000000000888, -1.859271017917181981E-14, -159.6636751345948539 ) ) ;
#291 = CARTESIAN_POINT ( 'NONE',  ( 0.000000000000000000, 5.499999999999991118, -113.9999999999999858 ) ) ;
#292 = CARTESIAN_POINT ( 'NONE',  ( 116.2113248654050750, -2.000000000000029310, 0.000000000000000000 ) ) ;
#293 = CARTESIAN_POINT ( 'NONE',  ( 5.196152422706629359, 3.000000000000002665, -89.03867513459485394 ) ) ;
#294 = ORIENTED_EDGE ( 'NONE', *, *, #12008, .F. ) ;
#295 = CARTESIAN_POINT ( 'NONE',  ( 17.56250000000009592, 2.649519052838419153, -1.097466725451619718 ) ) ;
#296 = CIRCLE ( 'NONE', #5196, 0.5000000000000004441 ) ;
#297 = FACE_OUTER_BOUND ( 'NONE', #159, .T. ) ;
#298 = ADVANCED_FACE ( 'NONE', ( #18607 ), #22898, .T. ) ;
#299 = LINE ( 'NONE', #12465, #20459 ) ;
#300 = FACE_OUTER_BOUND ( 'NONE', #4802, .T. ) ;
#301 = ORIENTED_EDGE ( 'NONE', *, *, #25346, .T. ) ;
#302 = PLANE ( 'NONE',  #5431 ) ;
#303 = CARTESIAN_POINT ( 'NONE',  ( -2.775557561562891351E-14, -5.500000000000115463, -177.7500000000000284 ) ) ;
#304 = CARTESIAN_POINT ( 'NONE',  ( -5.999999999999919176, 1.607695154586804565, -109.4806624327025872 ) ) ;
#305 = VERTEX_POINT ( 'NONE', #20290 ) ;
#306 = ADVANCED_FACE ( 'NONE', ( #6902 ), #3947, .F. ) ;
#307 = CARTESIAN_POINT ( 'NONE',  ( 157.0386751345948539, -5.500000000000005329, 0.000000000000000000 ) ) ;
#308 = CARTESIAN_POINT ( 'NONE',  ( 140.9925748654052029, 2.278174593052074925, 5.499999999999950262 ) ) ;
#309 = ORIENTED_EDGE ( 'NONE', *, *, #13878, .F. ) ;
#310 = CARTESIAN_POINT ( 'NONE',  ( 6.000000000000000888, 1.607695154586715303, -141.5966878364870354 ) ) ;
#311 = CARTESIAN_POINT ( 'NONE',  ( 138.4687500000000284, -2.485281374238585972, 6.000000000000005329 ) ) ;
#312 = AXIS2_PLACEMENT_3D ( 'NONE', #25231, #13938, #2374 ) ;
#313 = CARTESIAN_POINT ( 'NONE',  ( 3.608439182435180470, -6.249999999999997335, -139.6919872981078470 ) ) ;
#314 =( LENGTH_UNIT ( ) NAMED_UNIT ( * ) SI_UNIT ( .MILLI., .METRE. ) );
#315 = CARTESIAN_POINT ( 'NONE',  ( 10.25000000000000888, 1.873492889144956486, -1.873492889144900975 ) ) ;
#316 = CARTESIAN_POINT ( 'NONE',  ( 0.000000000000000000, -5.999999999999991118, -116.5386751345948113 ) ) ;
#317 = CARTESIAN_POINT ( 'NONE',  ( 19.31250000000010303, -0.8284271247459350507, 2.000000000000091926 ) ) ;
#318 = CARTESIAN_POINT ( 'NONE',  ( 0.1092184406287978471, -15.15152031211519201, 8.760553818335999665 ) ) ;
#319 = CARTESIAN_POINT ( 'NONE',  ( 136.1101497308104342, 3.535533905932725318, 3.535533905932725318 ) ) ;
#320 = CARTESIAN_POINT ( 'NONE',  ( -6.000000000000007105, -1.607695154586655129, -56.84668783648705670 ) ) ;
#321 = CARTESIAN_POINT ( 'NONE',  ( -5.196152422706601826, 2.999999999999975131, -92.46132486540520290 ) ) ;
#322 = CARTESIAN_POINT ( 'NONE',  ( -5.196152422706601826, 2.999999999999975131, -60.03867513459481842 ) ) ;
#323 = CYLINDRICAL_SURFACE ( 'NONE', #17586, 6.000000000000000888 ) ;
#324 = CARTESIAN_POINT ( 'NONE',  ( 105.4374999999998153, -2.499999999999994671, 1.035533905932929599 ) ) ;
#325 =( BOUNDED_CURVE ( )  B_SPLINE_CURVE ( 2, ( #10202, #24450, #15442, #15117, #22321, #16023, #7867, #17427, #1256 ),
 .UNSPECIFIED., .F., .T. ) 
 B_SPLINE_CURVE_WITH_KNOTS ( ( 3, 2, 2, 2, 3 ),
 ( 0.9694444444444444420, 0.9703703703703703276, 0.9722222222222222099, 0.9740740740740740922, 0.9749999999999999778 ),
 .UNSPECIFIED. ) 
 CURVE ( )  GEOMETRIC_REPRESENTATION_ITEM ( )  RATIONAL_B_SPLINE_CURVE ( ( 0.9330127018922194093, 0.9330127018922194093, 1.000000000000000000, 0.8660254037844388186, 1.000000000000000000, 0.8660254037844388186, 1.000000000000000000, 0.9330127018922234061, 0.9330127018922194093 ) ) 
 REPRESENTATION_ITEM ( '' )  );
#326 = CARTESIAN_POINT ( 'NONE',  ( -3.464101615137725076, 5.999999999999979572, -112.6636751345948113 ) ) ;
#327 = ORIENTED_EDGE ( 'NONE', *, *, #30362, .T. ) ;
#328 = ADVANCED_FACE ( 'NONE', ( #15715 ), #11243, .F. ) ;
#329 = CARTESIAN_POINT ( 'NONE',  ( -20.99999999999998224, -54.99999999999990763, -4.000000000000003553 ) ) ;
#330 = CARTESIAN_POINT ( 'NONE',  ( 5.196152422706629359, 3.000000000000002665, -88.46132486540525974 ) ) ;
#331 = DIRECTION ( 'NONE',  ( 1.000000000000000000, -5.551115123125773458E-17, -1.260129944081490338E-35 ) ) ;
#332 = EDGE_CURVE ( 'NONE', #7475, #16343, #25564, .T. ) ;
#333 = ORIENTED_EDGE ( 'NONE', *, *, #11296, .T. ) ;
#334 = CARTESIAN_POINT ( 'NONE',  ( 116.4372167782373850, 0.7662911109078588412, -1.849990392679411677 ) ) ;
#335 = PRESENTATION_STYLE_ASSIGNMENT (( #28879 ) ) ;
#336 = CARTESIAN_POINT ( 'NONE',  ( -5.412658773652684552, -3.125000000000099920, -107.0669872981078186 ) ) ;
#337 = CARTESIAN_POINT ( 'NONE',  ( 133.5000000000000284, 6.000000000000005329, 0.000000000000000000 ) ) ;
#338 = CARTESIAN_POINT ( 'NONE',  ( 116.6249999999999716, -1.767766952966459693, -1.767766952966209892 ) ) ;
#339 = COLOUR_RGB ( '', 0.72549020, 0.75294118, 0.79215686) ;
#340 = CARTESIAN_POINT ( 'NONE',  ( -2.775557561562891351E-14, -5.500000000000115463, -126.7500000000000284 ) ) ;
#341 = VERTEX_POINT ( 'NONE', #2733 ) ;
#342 = ORIENTED_EDGE ( 'NONE', *, *, #4463, .F. ) ;
#343 = CARTESIAN_POINT ( 'NONE',  ( 0.000000000000000000, 5.999999999999977796, -163.2113248654052313 ) ) ;
#344 = CARTESIAN_POINT ( 'NONE',  ( 6.350852961086080661, -9.614813431917819062E-14, -58.87500000000005684 ) ) ;
#345 = CARTESIAN_POINT ( 'NONE',  ( 3.464101615137852974, 5.999999999999884537, -115.9136751345948255 ) ) ;
#346 = CARTESIAN_POINT ( 'NONE',  ( 159.0000000000000284, -12.00000000000001066, -4.000000000000003553 ) ) ;
#347 = CARTESIAN_POINT ( 'NONE',  ( -3.608439182435052128, -6.250000000000110134, -83.80801270189228092 ) ) ;
#348 = AXIS2_PLACEMENT_3D ( 'NONE', #13196, #18093, #13038 ) ;
#349 = CARTESIAN_POINT ( 'NONE',  ( 106.5622167782373708, 1.849990392679501827, -0.7662911109076485650 ) ) ;
#350 = CARTESIAN_POINT ( 'NONE',  ( 140.9019117484300523, -11.80382349685862486, -4.000000000000003553 ) ) ;
#351 = DIRECTION ( 'NONE',  ( 1.000000000000000000, -0.000000000000000000, -0.000000000000000000 ) ) ;
#352 = CARTESIAN_POINT ( 'NONE',  ( 114.3127832217620465, 1.849990392679562001, -0.7662911109076485650 ) ) ;
#353 = CARTESIAN_POINT ( 'NONE',  ( 4.763139720814407951, 2.750000000000002665, -141.2500000000000000 ) ) ;
#354 = CARTESIAN_POINT ( 'NONE',  ( 140.0509928599997238, -9.340762233865111952, 7.535282035301673176 ) ) ;
#355 = AXIS2_PLACEMENT_3D ( 'NONE', #19839, #19142, #17411 ) ;
#356 = CARTESIAN_POINT ( 'NONE',  ( -5.999999999999919176, 1.607695154586804565, -89.40331216351302146 ) ) ;
#357 = CARTESIAN_POINT ( 'NONE',  ( -4.763139720814407951, -2.750000000000016431, -70.00000000000000000 ) ) ;
#358 = AXIS2_PLACEMENT_3D ( 'NONE', #28689, #759, #17069 ) ;
#359 = CARTESIAN_POINT ( 'NONE',  ( 145.1175748654052597, 5.500000000000012434, -2.278174593052012309 ) ) ;
#360 =( NAMED_UNIT ( * ) SI_UNIT ( $, .STERADIAN. ) SOLID_ANGLE_UNIT ( ) );
#361 = CARTESIAN_POINT ( 'NONE',  ( 4.763139720814407951, -2.749999999999988454, -68.00000000000000000 ) ) ;
#362 = EDGE_CURVE ( 'NONE', #22602, #4075, #22644, .T. ) ;
#363 = CARTESIAN_POINT ( 'NONE',  ( 139.5500633684294769, -9.165151389911672553, 8.000000000000010658 ) ) ;
#364 = CARTESIAN_POINT ( 'NONE',  ( 146.8273502691896510, -5.000000000000004441, 0.000000000000000000 ) ) ;
#365 = CARTESIAN_POINT ( 'NONE',  ( 13.99999999999999822, 0.000000000000000000, 17.50000000000000355 ) ) ;
#366 = CARTESIAN_POINT ( 'NONE',  ( 160.5937500000000284, 6.000000000000005329, 2.485281374238585972 ) ) ;
#367 = CARTESIAN_POINT ( 'NONE',  ( 135.0000000000000284, -8.301023251189437957, -7.690744244795082452 ) ) ;
#368 = FACE_OUTER_BOUND ( 'NONE', #26036, .T. ) ;
#369 = CARTESIAN_POINT ( 'NONE',  ( 115.6872167782374561, 1.849990392679532247, 0.7662911109080692285 ) ) ;
#370 =( NAMED_UNIT ( * ) PLANE_ANGLE_UNIT ( ) SI_UNIT ( $, .RADIAN. ) );
#371 = VERTEX_POINT ( 'NONE', #11866 ) ;
#372 = CARTESIAN_POINT ( 'NONE',  ( 148.4062500000000568, 6.000000000000005329, -2.485281374238555774 ) ) ;
#373 = CARTESIAN_POINT ( 'NONE',  ( 112.5627832217621886, 0.7662911109078588412, 1.849990392679712103 ) ) ;
#374 =( NAMED_UNIT ( * ) PLANE_ANGLE_UNIT ( ) SI_UNIT ( $, .RADIAN. ) );
#375 = CARTESIAN_POINT ( 'NONE',  ( 5.196152422706629359, -2.999999999999988898, -158.2886751345948824 ) ) ;
#376 = CARTESIAN_POINT ( 'NONE',  ( 5.412658773652739619, 3.124999999999988898, -46.31698729810784698 ) ) ;
#377 = CARTESIAN_POINT ( 'NONE',  ( 20.25000000000015632, 1.110223024625156540E-13, 1.999999999999946265 ) ) ;
#378 = CARTESIAN_POINT ( 'NONE',  ( -3.608439182435115633, 6.249999999999965361, -152.4419872981078186 ) ) ;
#379 = VERTEX_POINT ( 'NONE', #23659 ) ;
#380 = CARTESIAN_POINT ( 'NONE',  ( 6.350852961086080661, -9.614813431917819062E-14, -93.37500000000001421 ) ) ;
#381 = ORIENTED_EDGE ( 'NONE', *, *, #8508, .F. ) ;
#382 = CARTESIAN_POINT ( 'NONE',  ( -5.999999999999963585, 8.134310703387671600E-14, -146.9136751345948255 ) ) ;
#383 = CARTESIAN_POINT ( 'NONE',  ( 155.5163997308104342, 4.999999999999989342, 2.071067811865468400 ) ) ;
#384 = EDGE_CURVE ( 'NONE', #3266, #22196, #14318, .T. ) ;
#385 = CARTESIAN_POINT ( 'NONE',  ( 3.464101615137852974, 5.999999999999884537, -54.41367513459480421 ) ) ;
#386 = CYLINDRICAL_SURFACE ( 'NONE', #2332, 2.000000000000012879 ) ;
#387 = SURFACE_SIDE_STYLE ('',( #14990 ) ) ;
#388 = CARTESIAN_POINT ( 'NONE',  ( 6.000000000000000888, -1.859271017917181981E-14, -58.58632486540521001 ) ) ;
#389 = FILL_AREA_STYLE_COLOUR ( '', #23703 ) ;
#390 = CARTESIAN_POINT ( 'NONE',  ( -6.350852961085760029, -1.281975124255709124E-13, -161.6250000000000284 ) ) ;
#391 = CARTESIAN_POINT ( 'NONE',  ( 3.464101615137852974, 5.999999999999884537, -58.33632486540519579 ) ) ;
#392 = STYLED_ITEM ( 'NONE', ( #29024 ), #17172 ) ;
#393 = CARTESIAN_POINT ( 'NONE',  ( 3.175426480543072749, 5.499999999999865885, -157.6250000000000000 ) ) ;
#394 = CARTESIAN_POINT ( 'NONE',  ( 113.9999999999998153, 2.500000000000085265, 0.000000000000000000 ) ) ;
#395 = CARTESIAN_POINT ( 'NONE',  ( -5.999999999999963585, 1.780251999655701777E-13, -52.41367513459481842 ) ) ;
#396 = CARTESIAN_POINT ( 'NONE',  ( 4.763139720814407951, -2.749999999999988454, -104.0000000000000426 ) ) ;
#397 = PLANE ( 'NONE',  #15284 ) ;
#398 = CARTESIAN_POINT ( 'NONE',  ( 4.763139720814407951, 2.750000000000002665, -85.75000000000000000 ) ) ;
#399 = EDGE_CURVE ( 'NONE', #13073, #10035, #3539, .T. ) ;
#400 = CARTESIAN_POINT ( 'NONE',  ( 155.3586002691896226, 2.071067811865468400, 4.999999999999989342 ) ) ;
#401 = CARTESIAN_POINT ( 'NONE',  ( 106.8511751345945981, -1.999999999999941602, -0.8284271247459350507 ) ) ;
#402 = CARTESIAN_POINT ( 'NONE',  ( 111.3749999999999289, -1.767766952966320915, 1.767766952966431937 ) ) ;
#403 = CARTESIAN_POINT ( 'NONE',  ( 6.000000000000000888, 1.743066579297358182E-13, -66.08632486540521711 ) ) ;
#404 = CARTESIAN_POINT ( 'NONE',  ( 149.3363248654052029, 0.000000000000000000, -5.500000000000005329 ) ) ;
#405 = DIRECTION ( 'NONE',  ( -7.147005652999508048E-36, 5.642372883946980038E-36, 1.000000000000000000 ) ) ;
#406 =( BOUNDED_CURVE ( )  B_SPLINE_CURVE ( 2, ( #1039, #17971, #8566, #24843, #3636, #27284, #29442, #15202, #10435 ),
 .UNSPECIFIED., .F., .T. ) 
 B_SPLINE_CURVE_WITH_KNOTS ( ( 3, 2, 2, 2, 3 ),
 ( 0.7305555555555556246, 0.7314814814814813992, 0.7333333333333333925, 0.7351851851851851638, 0.7361111111111111605 ),
 .UNSPECIFIED. ) 
 CURVE ( )  GEOMETRIC_REPRESENTATION_ITEM ( )  RATIONAL_B_SPLINE_CURVE ( ( 0.9330127018922194093, 0.9330127018922274029, 1.000000000000000000, 0.8660254037844388186, 1.000000000000000000, 0.8660254037844388186, 1.000000000000000000, 0.9330127018922154125, 0.9330127018922194093 ) ) 
 REPRESENTATION_ITEM ( '' )  );
#407 = VERTEX_POINT ( 'NONE', #16470 ) ;
#408 = DIRECTION ( 'NONE',  ( -8.326672684688675286E-17, -2.081668171172168821E-17, 1.000000000000000000 ) ) ;
#409 = CARTESIAN_POINT ( 'NONE',  ( 107.5622167782374561, 1.849990392679472073, -0.7662911109077686911 ) ) ;
#410 = ORIENTED_EDGE ( 'NONE', *, *, #8956, .T. ) ;
#411 =( BOUNDED_CURVE ( )  B_SPLINE_CURVE ( 2, ( #22599, #27778, #25320, #13714, #3980, #25172, #11559, #20749, #13403 ),
 .UNSPECIFIED., .F., .T. ) 
 B_SPLINE_CURVE_WITH_KNOTS ( ( 3, 2, 2, 2, 3 ),
 ( 0.7916666666666666297, 0.7925925925925926263, 0.7944444444444445086, 0.7962962962962962798, 0.7972222222222222765 ),
 .UNSPECIFIED. ) 
 CURVE ( )  GEOMETRIC_REPRESENTATION_ITEM ( )  RATIONAL_B_SPLINE_CURVE ( ( 0.9330127018922194093, 0.9330127018922154125, 1.000000000000000000, 0.8660254037844388186, 1.000000000000000000, 0.8660254037844388186, 1.000000000000000000, 0.9330127018922154125, 0.9330127018922194093 ) ) 
 REPRESENTATION_ITEM ( '' )  );
#412 = ORIENTED_EDGE ( 'NONE', *, *, #17980, .F. ) ;
#413 = CARTESIAN_POINT ( 'NONE',  ( 146.7187500000000284, 2.485281374238555774, -6.000000000000005329 ) ) ;
#414 = ORIENTED_EDGE ( 'NONE', *, *, #12706, .T. ) ;
#415 = CARTESIAN_POINT ( 'NONE',  ( -6.350852961085760029, -1.281975124255709124E-13, -116.6250000000000000 ) ) ;
#416 = CARTESIAN_POINT ( 'NONE',  ( 18.12500000000011369, 1.110223024625156540E-13, -2.649519052838278377 ) ) ;
#417 = CARTESIAN_POINT ( 'NONE',  ( -7.216878364870328078, 0.000000000000000000, -126.0580127018922383 ) ) ;
#418 = UNCERTAINTY_MEASURE_WITH_UNIT (LENGTH_MEASURE( 1.000000000000000082E-05 ), #11834, 'distance_accuracy_value', 'NONE');
#419 = ORIENTED_EDGE ( 'NONE', *, *, #27844, .T. ) ;
#420 = DIRECTION ( 'NONE',  ( -7.147005652999508048E-36, 5.642372883946980038E-36, 1.000000000000000000 ) ) ;
#421 = CARTESIAN_POINT ( 'NONE',  ( -5.412658773652739619, 3.124999999999975131, -164.3169872981078470 ) ) ;
#422 = CARTESIAN_POINT ( 'NONE',  ( 108.1874999999998579, 1.035533905932719101, 2.500000000000205169 ) ) ;
#423 = CARTESIAN_POINT ( 'NONE',  ( 133.4851497308104058, -3.535533905932725318, 3.535533905932725318 ) ) ;
#424 = EDGE_CURVE ( 'NONE', #5958, #13461, #21610, .T. ) ;
#425 = ORIENTED_EDGE ( 'NONE', *, *, #2357, .T. ) ;
#426 = CARTESIAN_POINT ( 'NONE',  ( 0.2111655239558809238, -15.49101385207805492, -8.141616853885579985 ) ) ;
#427 = CARTESIAN_POINT ( 'NONE',  ( 158.5386751345948539, -5.500000000000005329, 0.000000000000000000 ) ) ;
#428 = CYLINDRICAL_SURFACE ( 'NONE', #8935, 30.00000000000000000 ) ;
#429 = CARTESIAN_POINT ( 'NONE',  ( -6.350852961085760029, -1.281975124255709124E-13, -178.1250000000000568 ) ) ;
#430 = CARTESIAN_POINT ( 'NONE',  ( 109.6252832217622739, -2.775557561562891351E-14, 1.849990392679523588 ) ) ;
#431 = CARTESIAN_POINT ( 'NONE',  ( 1.110223024625164183E-16, -2.000000000000012879, -1.776356839400262692E-15 ) ) ;
#432 = CARTESIAN_POINT ( 'NONE',  ( 5.412658773652712085, -3.125000000000086153, -180.9330127018922099 ) ) ;
#433 = CARTESIAN_POINT ( 'NONE',  ( 3.464101615137852974, 5.999999999999884537, -76.33632486540521711 ) ) ;
#434 = CARTESIAN_POINT ( 'NONE',  ( 6.000000000000000888, -1.859271017917181981E-14, -101.1636751345948397 ) ) ;
#435 = CARTESIAN_POINT ( 'NONE',  ( 3.175426480543072749, 5.499999999999865885, -123.1250000000000426 ) ) ;
#436 = EDGE_CURVE ( 'NONE', #17742, #25655, #11378, .T. ) ;
#437 = CARTESIAN_POINT ( 'NONE',  ( 4.763139720814407951, -2.749999999999988454, -115.9999999999999858 ) ) ;
#438 = CARTESIAN_POINT ( 'NONE',  ( 135.4999999999990052, -9.047800747817513312, -8.000000000000007105 ) ) ;
#439 = DIRECTION ( 'NONE',  ( -1.000000000000000000, -1.665334536937736783E-16, -2.220446049250315546E-16 ) ) ;
#440 = ORIENTED_EDGE ( 'NONE', *, *, #16202, .T. ) ;
#441 = DIRECTION ( 'NONE',  ( 0.000000000000000000, 0.000000000000000000, -1.000000000000000000 ) ) ;
#442 = CARTESIAN_POINT ( 'NONE',  ( -6.000000000000007105, -1.607695154586655129, -137.2693375672974412 ) ) ;
#443 = EDGE_LOOP ( 'NONE', ( #123, #12542, #25078, #1896 ) ) ;
#444 = CARTESIAN_POINT ( 'NONE',  ( 111.7886751345948255, -1.999999999999974021, 0.000000000000000000 ) ) ;
#445 = CARTESIAN_POINT ( 'NONE',  ( -3.175426480542816066, -5.500000000000057732, -176.3750000000000284 ) ) ;
#446 = AXIS2_PLACEMENT_3D ( 'NONE', #10967, #13586, #23085 ) ;
#447 = CARTESIAN_POINT ( 'NONE',  ( 6.000000000000000888, -1.859271017917181981E-14, -110.1636751345948397 ) ) ;
#448 = VERTEX_POINT ( 'NONE', #25798 ) ;
#449 = CARTESIAN_POINT ( 'NONE',  ( 6.000000000000000888, 1.743066579297358182E-13, -77.16367513459482552 ) ) ;
#450 =( BOUNDED_CURVE ( )  B_SPLINE_CURVE ( 2, ( #19930, #8557, #7941, #22090, #29276, #19775, #5935, #15359, #8402 ),
 .UNSPECIFIED., .F., .F. ) 
 B_SPLINE_CURVE_WITH_KNOTS ( ( 3, 2, 2, 2, 3 ),
 ( 0.1874999999999996947, 0.1937499999999999500, 0.2000000000000002054, 0.2062500000000004330, 0.2125000000000006883 ),
 .UNSPECIFIED. ) 
 CURVE ( )  GEOMETRIC_REPRESENTATION_ITEM ( )  RATIONAL_B_SPLINE_CURVE ( ( 1.000000000000003775, 0.9238795325112830747, 1.000000000000000000, 0.9238795325112867385, 1.000000000000000000, 0.9238795325112867385, 1.000000000000000000, 0.9238795325112783008, 1.000000000000008438 ) ) 
 REPRESENTATION_ITEM ( '' )  );
#451 = ORIENTED_EDGE ( 'NONE', *, *, #28247, .T. ) ;
#452 = VERTEX_POINT ( 'NONE', #16766 ) ;
#453 = CARTESIAN_POINT ( 'NONE',  ( -5.999999999999919176, 1.607695154586804565, -84.90331216351302146 ) ) ;
#454 = CARTESIAN_POINT ( 'NONE',  ( 134.4523502691896510, 0.000000000000000000, 5.000000000000004441 ) ) ;
#455 = CARTESIAN_POINT ( 'NONE',  ( 10.93750000000009948, 2.000000000000091926, -0.8284271247462354770 ) ) ;
#456 = ORIENTED_EDGE ( 'NONE', *, *, #9428, .T. ) ;
#457 = CARTESIAN_POINT ( 'NONE',  ( -7.216878364870328078, 0.000000000000000000, -131.1919872981078754 ) ) ;
#458 = CARTESIAN_POINT ( 'NONE',  ( 12.37500000000010836, 2.649519052838500421, 0.000000000000000000 ) ) ;
#459 = CARTESIAN_POINT ( 'NONE',  ( 116.0000000000000142, 0.000000000000000000, -5.500000000000000000 ) ) ;
#460 = ADVANCED_FACE ( 'NONE', ( #26093 ), #4748, .F. ) ;
#461 = ORIENTED_EDGE ( 'NONE', *, *, #4777, .F. ) ;
#462 = CARTESIAN_POINT ( 'NONE',  ( 20.43750000000014566, -1.999999999999911626, 0.8284271247462354770 ) ) ;
#463 = CARTESIAN_POINT ( 'NONE',  ( 0.1053031288717025393, -15.23283975038566318, 8.619984219653339608 ) ) ;
#464 = CARTESIAN_POINT ( 'NONE',  ( 139.8601497308104058, -3.535533905932725318, -3.535533905932725318 ) ) ;
#465 = CARTESIAN_POINT ( 'NONE',  ( 22.97617513459487881, -1.035533905932689347, -2.500000000000024425 ) ) ;
#466 = DIRECTION ( 'NONE',  ( 1.000000000000000000, 0.000000000000000000, 0.000000000000000000 ) ) ;
#467 = LINE ( 'NONE', #14635, #3548 ) ;
#468 =( NAMED_UNIT ( * ) PLANE_ANGLE_UNIT ( ) SI_UNIT ( $, .RADIAN. ) );
#469 = PRESENTATION_STYLE_ASSIGNMENT (( #21238 ) ) ;
#470 = CARTESIAN_POINT ( 'NONE',  ( 104.8124999999998153, 1.035533905932779275, -2.499999999999904521 ) ) ;
#471 = DIRECTION ( 'NONE',  ( 1.000000000000000000, -5.551115123125773458E-17, -1.260129944081490338E-35 ) ) ;
#472 = AXIS2_PLACEMENT_3D ( 'NONE', #8835, #8361, #29233 ) ;
#473 = EDGE_CURVE ( 'NONE', #2749, #5395, #21945, .T. ) ;
#474 = AXIS2_PLACEMENT_3D ( 'NONE', #15433, #6176, #10653 ) ;
#475 = CARTESIAN_POINT ( 'NONE',  ( 15.71132486540535744, 2.500000000000113243, -1.110223024625156540E-13 ) ) ;
#476 = VERTEX_POINT ( 'NONE', #745 ) ;
#477 = DIRECTION ( 'NONE',  ( 0.000000000000000000, 1.224646799147353454E-16, 1.000000000000000000 ) ) ;
#478 = CARTESIAN_POINT ( 'NONE',  ( -5.196152422706601826, 2.999999999999975131, -62.46132486540523132 ) ) ;
#479 = ORIENTED_EDGE ( 'NONE', *, *, #25996, .F. ) ;
#480 = CARTESIAN_POINT ( 'NONE',  ( 115.9372167782375129, -0.7662911109076785410, 1.849990392679712103 ) ) ;
#481 = CARTESIAN_POINT ( 'NONE',  ( 136.2187500000000284, 2.485281374238556218, -6.000000000000005329 ) ) ;
#482 = CARTESIAN_POINT ( 'NONE',  ( 11.93750000000008527, 2.000000000000091926, -0.8284271247462354770 ) ) ;
#483 = CARTESIAN_POINT ( 'NONE',  ( -5.412658773652739619, 3.124999999999975131, -107.3169872981078470 ) ) ;
#484 = CARTESIAN_POINT ( 'NONE',  ( 0.000000000000000000, -5.999999999999991118, -50.53867513459481131 ) ) ;
#485 = CARTESIAN_POINT ( 'NONE',  ( 160.9538997308104058, -2.071067811865468400, -4.999999999999989342 ) ) ;
#486 = CARTESIAN_POINT ( 'NONE',  ( 116.4999999999999574, -2.499999999999891198, 0.000000000000000000 ) ) ;
#487 = CIRCLE ( 'NONE', #25995, 17.50000000000000355 ) ;
#488 = CARTESIAN_POINT ( 'NONE',  ( -4.763139720814407951, -2.750000000000016431, -128.5000000000000000 ) ) ;
#489 = AXIS2_PLACEMENT_3D ( 'NONE', #15313, #15469, #1284 ) ;
#490 = ORIENTED_EDGE ( 'NONE', *, *, #27090, .F. ) ;
#491 =( NAMED_UNIT ( * ) SI_UNIT ( $, .STERADIAN. ) SOLID_ANGLE_UNIT ( ) );
#492 = CARTESIAN_POINT ( 'NONE',  ( -4.763139720814407951, -2.750000000000016431, -58.00000000000004974 ) ) ;
#493 = EDGE_CURVE ( 'NONE', #3216, #20658, #28980, .T. ) ;
#494 = CARTESIAN_POINT ( 'NONE',  ( 3.464101615137757051, -5.999999999999979572, -179.4136751345948255 ) ) ;
#495 = ADVANCED_FACE ( 'NONE', ( #14745 ), #24385, .T. ) ;
#496 = CARTESIAN_POINT ( 'NONE',  ( -5.412658773652739619, 3.124999999999975131, -85.68301270189226670 ) ) ;
#497 =( BOUNDED_CURVE ( )  B_SPLINE_CURVE ( 2, ( #1610, #24805, #8523, #10863, #3898, #11012, #30329, #18684, #16396 ),
 .UNSPECIFIED., .F., .T. ) 
 B_SPLINE_CURVE_WITH_KNOTS ( ( 3, 2, 2, 2, 3 ),
 ( 0.3027777777777777568, 0.3037037037037036979, 0.3055555555555555802, 0.3074074074074074070, 0.3083333333333333481 ),
 .UNSPECIFIED. ) 
 CURVE ( )  GEOMETRIC_REPRESENTATION_ITEM ( )  RATIONAL_B_SPLINE_CURVE ( ( 0.9330127018922194093, 0.9330127018922174109, 1.000000000000000000, 0.8660254037844388186, 1.000000000000000000, 0.8660254037844388186, 1.000000000000000000, 0.9330127018922174109, 0.9330127018922194093 ) ) 
 REPRESENTATION_ITEM ( '' )  );
#498 = UNCERTAINTY_MEASURE_WITH_UNIT (LENGTH_MEASURE( 1.000000000000000082E-05 ), #21304, 'distance_accuracy_value', 'NONE');
#499 = LINE ( 'NONE', #202, #6440 ) ;
#500 = CARTESIAN_POINT ( 'NONE',  ( 105.2886751345946550, 2.000000000000057288, 0.000000000000000000 ) ) ;
#501 = CARTESIAN_POINT ( 'NONE',  ( 105.4997167782376550, 1.308140751793668288, -1.308140751793640533 ) ) ;
#502 = CARTESIAN_POINT ( 'NONE',  ( 116.0000000000000142, 0.000000000000000000, -5.500000000000000000 ) ) ;
#503 = CARTESIAN_POINT ( 'NONE',  ( 114.1877832217620892, 0.7662911109078588412, -1.849990392679291551 ) ) ;
#504 = CARTESIAN_POINT ( 'NONE',  ( -3.175426480542816066, 5.499999999999865885, -137.8750000000000568 ) ) ;
#505 = CARTESIAN_POINT ( 'NONE',  ( -5.999999999999963585, 1.780251999655701777E-13, -68.33632486540521711 ) ) ;
#506 = CARTESIAN_POINT ( 'NONE',  ( 3.608439182435180470, 6.249999999999982236, -156.5580127018922383 ) ) ;
#507 = CARTESIAN_POINT ( 'NONE',  ( 139.6011751345948539, 3.889087296526011706, -3.889087296526011706 ) ) ;
#508 = AXIS2_PLACEMENT_3D ( 'NONE', #25825, #23387, #22922 ) ;
#509 = CARTESIAN_POINT ( 'NONE',  ( 3.175426480543072749, -5.500000000000105693, -68.12500000000002842 ) ) ;
#510 = CARTESIAN_POINT ( 'NONE',  ( 6.000000000000000888, 1.607695154586715303, -114.5966878364870496 ) ) ;
#511 = CARTESIAN_POINT ( 'NONE',  ( 4.763139720814407951, -2.749999999999988454, -66.50000000000000000 ) ) ;
#512 = CARTESIAN_POINT ( 'NONE',  ( 3.464101615137852974, 5.999999999999884537, -53.83632486540516737 ) ) ;
#513 = CARTESIAN_POINT ( 'NONE',  ( 146.5461002691896510, -2.071067811865468400, 4.999999999999989342 ) ) ;
#514 = CARTESIAN_POINT ( 'NONE',  ( 6.000000000000000888, -1.607695154586752384, -144.1533121635130215 ) ) ;
#515 = CARTESIAN_POINT ( 'NONE',  ( 153.9375000000000284, -4.242640687119298093, -4.242640687119298093 ) ) ;
#516 = CARTESIAN_POINT ( 'NONE',  ( 0.000000000000000000, 5.999999999999977796, -133.7886751345947971 ) ) ;
#517 = CARTESIAN_POINT ( 'NONE',  ( 115.1488248654049613, -1.999999999999941602, 0.8284271247464759513 ) ) ;
#518 = DIRECTION ( 'NONE',  ( 1.000000000000000000, -5.551115123125773458E-17, -1.260129944081490338E-35 ) ) ;
#520 = ORIENTED_EDGE ( 'NONE', *, *, #8340, .T. ) ;
#519 = AXIS2_PLACEMENT_3D ( 'NONE', #17217, #21810, #19211 ) ;
#521 = CARTESIAN_POINT ( 'NONE',  ( 149.6250000000000284, 0.000000000000000000, -6.000000000000005329 ) ) ;
#522 = CARTESIAN_POINT ( 'NONE',  ( 118.8511751345945413, -1.999999999999911626, -0.8284271247460553989 ) ) ;
#523 = UNCERTAINTY_MEASURE_WITH_UNIT (LENGTH_MEASURE( 1.000000000000000082E-05 ), #26176, 'distance_accuracy_value', 'NONE');
#524 = CARTESIAN_POINT ( 'NONE',  ( 104.7836787521071216, 1.152921169277180358, 1.489079044806365992 ) ) ;
#525 = CARTESIAN_POINT ( 'NONE',  ( -4.763139720814407951, 2.749999999999946709, -176.7500000000000284 ) ) ;
#526 = CARTESIAN_POINT ( 'NONE',  ( 22.00000000000010303, 2.000000000000168310, 0.000000000000000000 ) ) ;
#527 = ORIENTED_EDGE ( 'NONE', *, *, #25589, .T. ) ;
#528 = CARTESIAN_POINT ( 'NONE',  ( 5.412658773652712085, -3.125000000000086153, -151.5669872981077901 ) ) ;
#529 = ORIENTED_EDGE ( 'NONE', *, *, #11929, .F. ) ;
#530 = CARTESIAN_POINT ( 'NONE',  ( 0.000000000000000000, 5.499999999999991118, -79.50000000000001421 ) ) ;
#531 = AXIS2_PLACEMENT_3D ( 'NONE', #29230, #26925, #12705 ) ;
#532 = EDGE_CURVE ( 'NONE', #23217, #14931, #6701, .T. ) ;
#533 = EDGE_CURVE ( 'NONE', #16758, #856, #5098, .T. ) ;
#534 = CARTESIAN_POINT ( 'NONE',  ( 2.775557561562891351E-14, -6.250000000000061284, -98.68301270189222407 ) ) ;
#535 = ORIENTED_EDGE ( 'NONE', *, *, #24962, .F. ) ;
#536 = AXIS2_PLACEMENT_3D ( 'NONE', #24063, #9950, #268 ) ;
#537 = CARTESIAN_POINT ( 'NONE',  ( 6.000000000000000888, 1.743066579297358182E-13, -99.08632486540518869 ) ) ;
#538 = DIRECTION ( 'NONE',  ( 5.551115123125785167E-17, -1.000000000000000000, -8.881784197001256268E-16 ) ) ;
#539 = CARTESIAN_POINT ( 'NONE',  ( 111.4613248654051176, 5.551115123125782702E-14, -2.000000000000001776 ) ) ;
#540 = CARTESIAN_POINT ( 'NONE',  ( 134.9486760520005078, -8.594915014419392207, 8.000000000000007105 ) ) ;
#541 = FILL_AREA_STYLE ('',( #389 ) ) ;
#542 = CARTESIAN_POINT ( 'NONE',  ( -6.350852961085760029, -1.281975124255709124E-13, -167.6249999999999716 ) ) ;
#543 = CARTESIAN_POINT ( 'NONE',  ( 143.3363248654052029, 0.000000000000000000, -5.500000000000005329 ) ) ;
#544 = CARTESIAN_POINT ( 'NONE',  ( -3.175426480542816510, -5.500000000000057732, -155.3750000000000000 ) ) ;
#545 = CARTESIAN_POINT ( 'NONE',  ( -5.999999999999971578, 1.607695154586715303, -76.48066243270260145 ) ) ;
#546 = CARTESIAN_POINT ( 'NONE',  ( -3.464101615137757051, -5.999999999999979572, -104.0863248654052171 ) ) ;
#547 =( BOUNDED_SURFACE ( )  B_SPLINE_SURFACE ( 3, 2, ( 
 ( #13704, #1829, #23045 ),
 ( #11233, #20739, #27768 ),
 ( #8443, #14456, #16759 ),
 ( #2587, #11702, #20890 ),
 ( #2301, #21499, #23504 ),
 ( #4588, #426, #4740 ),
 ( #16902, #19192, #4435 ),
 ( #7051, #14167, #11858 ),
 ( #21198, #138, #737 ),
 ( #26662, #8079, #7637 ),
 ( #12747, #12446, #19491 ),
 ( #10269, #10420, #14736 ),
 ( #17198, #19634, #26225 ),
 ( #24223, #10119, #7781 ) ),
 .UNSPECIFIED., .F., .F., .F. ) 
 B_SPLINE_SURFACE_WITH_KNOTS ( ( 4, 2, 2, 2, 2, 2, 4 ),
 ( 3, 3 ),
 ( 0.007087992156775593799, 0.007143427954787825995, 0.007198863752800057324, 0.007254299550812288652, 0.007309735348824520848, 0.007420606944848983505, 0.007531478540873447029 ),
 ( 0.000000000000000000, 1.000000000000000000 ),
 .UNSPECIFIED. ) 
 GEOMETRIC_REPRESENTATION_ITEM ( )  RATIONAL_B_SPLINE_SURFACE ( (
 ( 1.000000000000000000, 0.8593225670956824436, 1.000000000000000000),
 ( 1.000000000000000000, 0.8663660590095438874, 1.000000000000000000),
 ( 1.000000000000000000, 0.8726340236266260098, 1.000000000000000000),
 ( 1.000000000000000000, 0.8802009473587890653, 1.000000000000000000),
 ( 1.000000000000000000, 0.8813323811479394365, 1.000000000000000000),
 ( 1.000000000000000000, 0.8771298408144754255, 1.000000000000000000),
 ( 1.000000000000000000, 0.8720285761146205905, 1.000000000000000000),
 ( 1.000000000000000000, 0.8593306477498514617, 1.000000000000000000),
 ( 1.000000000000000000, 0.8518162931196250343, 1.000000000000000000),
 ( 1.000000000000000000, 0.8295128813679467639, 1.000000000000000000),
 ( 1.000000000000000000, 0.8153081809651850920, 1.000000000000000000),
 ( 1.000000000000000000, 0.7919334258735726273, 1.000000000000000000),
 ( 1.000000000000000000, 0.7823637235328708694, 1.000000000000000000),
 ( 1.000000000000000000, 0.7743236465966842896, 1.000000000000000000) ) ) 
 REPRESENTATION_ITEM ( '' )  SURFACE ( )  );
#548 = CARTESIAN_POINT ( 'NONE',  ( -4.763139720814407951, 2.749999999999946709, -91.25000000000005684 ) ) ;
#549 = CARTESIAN_POINT ( 'NONE',  ( -5.999999999999963585, 8.134310703387671600E-14, -125.3363248654052171 ) ) ;
#550 = CARTESIAN_POINT ( 'NONE',  ( 145.4136751345948539, 0.000000000000000000, -5.500000000000005329 ) ) ;
#551 = CARTESIAN_POINT ( 'NONE',  ( -4.763139720814407951, -2.750000000000016431, -89.50000000000002842 ) ) ;
#552 = CARTESIAN_POINT ( 'NONE',  ( 135.5550748654052313, -5.500000000000012434, -2.278174593052012309 ) ) ;
#553 = DIRECTION ( 'NONE',  ( -7.147005652999508048E-36, 5.642372883946980038E-36, 1.000000000000000000 ) ) ;
#554 = CARTESIAN_POINT ( 'NONE',  ( 23.50000000000010303, -1.999999999999779732, -5.551115123125782702E-14 ) ) ;
#555 = CARTESIAN_POINT ( 'NONE',  ( 114.0624999999997300, 2.500000000000114575, 1.035533905932989551 ) ) ;
#556 = DIRECTION ( 'NONE',  ( 0.000000000000000000, 0.000000000000000000, -1.000000000000000000 ) ) ;
#557 = AXIS2_PLACEMENT_3D ( 'NONE', #30242, #4590, #11704 ) ;
#558 =( NAMED_UNIT ( * ) PLANE_ANGLE_UNIT ( ) SI_UNIT ( $, .RADIAN. ) );
#559 = FACE_OUTER_BOUND ( 'NONE', #25739, .T. ) ;
#560 = ORIENTED_EDGE ( 'NONE', *, *, #8732, .F. ) ;
#561 = CARTESIAN_POINT ( 'NONE',  ( 2.775557561562895769E-14, 11.00000000000000000, -14.99152654425661702 ) ) ;
#562 = LINE ( 'NONE', #14722, #2515 ) ;
#563 = VECTOR ( 'NONE', #154, 1000.000000000000000 ) ;
#564 = CARTESIAN_POINT ( 'NONE',  ( 104.6872167782374277, 1.849990392679532247, 0.7662911109080692285 ) ) ;
#565 = EDGE_CURVE ( 'NONE', #10035, #23969, #28298, .T. ) ;
#566 = VERTEX_POINT ( 'NONE', #11935 ) ;
#567 = VERTEX_POINT ( 'NONE', #2802 ) ;
#568 = CARTESIAN_POINT ( 'NONE',  ( 6.350852961086080661, -9.614813431917819062E-14, -108.3750000000000426 ) ) ;
#569 = CARTESIAN_POINT ( 'NONE',  ( 16.87499999999997158, -2.649519052838222866, 0.000000000000000000 ) ) ;
#570 = EDGE_CURVE ( 'NONE', #16363, #15998, #499, .T. ) ;
#571 = CARTESIAN_POINT ( 'NONE',  ( -5.412658773652739619, 3.124999999999975131, -124.6830127018922525 ) ) ;
#572 = ORIENTED_EDGE ( 'NONE', *, *, #9855, .F. ) ;
#573 = CARTESIAN_POINT ( 'NONE',  ( 158.3363248654052313, 0.000000000000000000, -5.500000000000005329 ) ) ;
#574 = CARTESIAN_POINT ( 'NONE',  ( -3.608439182435115633, 6.249999999999965361, -164.4419872981078186 ) ) ;
#575 = CARTESIAN_POINT ( 'NONE',  ( 107.4374999999997868, -2.499999999999964473, 1.035533905932989551 ) ) ;
#576 = AXIS2_PLACEMENT_3D ( 'NONE', #8205, #17621, #15159 ) ;
#577 = CARTESIAN_POINT ( 'NONE',  ( 132.7351497308104058, 3.535533905932725318, -3.535533905932725318 ) ) ;
#578 = VECTOR ( 'NONE', #10743, 1000.000000000000000 ) ;
#579 = CARTESIAN_POINT ( 'NONE',  ( -5.412658773652739619, 3.124999999999975131, -57.18301270189224539 ) ) ;
#580 = ORIENTED_EDGE ( 'NONE', *, *, #270, .T. ) ;
#581 = DIRECTION ( 'NONE',  ( 0.000000000000000000, -5.551115123125768527E-17, 1.000000000000000000 ) ) ;
#582 = CARTESIAN_POINT ( 'NONE',  ( 158.7261751345948539, -3.889087296526011706, -3.889087296526011706 ) ) ;
#583 = CARTESIAN_POINT ( 'NONE',  ( -4.763139720814407951, -2.750000000000016431, -175.0000000000000568 ) ) ;
#584 = CARTESIAN_POINT ( 'NONE',  ( 109.7502832217623734, -1.308140751793612777, 1.308140751793640533 ) ) ;
#585 = CARTESIAN_POINT ( 'NONE',  ( 0.000000000000000000, -5.999999999999991118, -112.9613248654052171 ) ) ;
#586 = CARTESIAN_POINT ( 'NONE',  ( 2.775557561562891351E-14, 6.250000000000033751, -177.4330127018922667 ) ) ;
#587 = DIRECTION ( 'NONE',  ( 0.000000000000000000, 1.000000000000000000, -1.224646799147353207E-16 ) ) ;
#588 = DIRECTION ( 'NONE',  ( 1.000000000000000000, 0.000000000000000000, 0.000000000000000000 ) ) ;
#589 = CARTESIAN_POINT ( 'NONE',  ( 3.175426480543072749, 5.499999999999865885, -118.6250000000000284 ) ) ;
#590 = CARTESIAN_POINT ( 'NONE',  ( -5.999999999999963585, 1.780251999655701777E-13, -48.83632486540521711 ) ) ;
#591 =( BOUNDED_CURVE ( )  B_SPLINE_CURVE ( 3, ( #1681, #22434, #25161, #22888 ),
 .UNSPECIFIED., .F., .T. ) 
 B_SPLINE_CURVE_WITH_KNOTS ( ( 4, 4 ),
 ( 1.570796326794896558, 2.746801533890014468 ),
 .UNSPECIFIED. ) 
 CURVE ( )  GEOMETRIC_REPRESENTATION_ITEM ( )  RATIONAL_B_SPLINE_CURVE ( ( 1.000000000000000000, 0.8880335295585656263, 0.8880335295585656263, 1.000000000000000000 ) ) 
 REPRESENTATION_ITEM ( '' )  );
#592 = CARTESIAN_POINT ( 'NONE',  ( -4.763139720814407951, -2.750000000000016431, -113.5000000000000426 ) ) ;
#593 = DIRECTION ( 'NONE',  ( -1.000000000000000000, 6.938893903907221278E-15, 0.000000000000000000 ) ) ;
#594 = CARTESIAN_POINT ( 'NONE',  ( 0.000000000000000000, 5.999999999999977796, -88.78867513459486815 ) ) ;
#595 = ORIENTED_EDGE ( 'NONE', *, *, #5857, .F. ) ;
#596 = AXIS2_PLACEMENT_3D ( 'NONE', #27372, #17745, #27220 ) ;
#597 = CARTESIAN_POINT ( 'NONE',  ( 6.000000000000000888, -1.859271017917181981E-14, -171.6636751345948539 ) ) ;
#598 = PLANE ( 'NONE',  #4757 ) ;
#599 =( BOUNDED_CURVE ( )  B_SPLINE_CURVE ( 2, ( #12471, #25953, #21667, #4903, #7659, #2902, #14759, #17068, #757 ),
 .UNSPECIFIED., .F., .T. ) 
 B_SPLINE_CURVE_WITH_KNOTS ( ( 3, 2, 2, 2, 3 ),
 ( 0.4531250000000000000, 0.4609375000000000000, 0.4687500000000000000, 0.4765625000000000000, 0.4843750000000000000 ),
 .UNSPECIFIED. ) 
 CURVE ( )  GEOMETRIC_REPRESENTATION_ITEM ( )  RATIONAL_B_SPLINE_CURVE ( ( 1.000000000000000000, 0.9238795325112867385, 1.000000000000000000, 0.9238795325112867385, 1.000000000000000000, 0.9238795325112867385, 1.000000000000000000, 0.9238795325112867385, 1.000000000000000000 ) ) 
 REPRESENTATION_ITEM ( '' )  );
#600 = ORIENTED_EDGE ( 'NONE', *, *, #19995, .T. ) ;
#601 = EDGE_CURVE ( 'NONE', #5531, #29422, #23638, .T. ) ;
#602 = CARTESIAN_POINT ( 'NONE',  ( 0.000000000000000000, 5.499999999999991118, -177.0000000000000568 ) ) ;
#603 = EDGE_CURVE ( 'NONE', #26278, #3013, #9857, .T. ) ;
#604 = CARTESIAN_POINT ( 'NONE',  ( 22.58632486540529527, 1.767766952966487448, -1.767766952966431937 ) ) ;
#605 = VERTEX_POINT ( 'NONE', #14955 ) ;
#606 = CARTESIAN_POINT ( 'NONE',  ( -5.196152422706573404, -3.000000000000002665, -125.7886751345948539 ) ) ;
#607 = ORIENTED_EDGE ( 'NONE', *, *, #14978, .T. ) ;
#608 = FACE_OUTER_BOUND ( 'NONE', #22324, .T. ) ;
#609 = CARTESIAN_POINT ( 'NONE',  ( 161.5312500000000568, -2.485281374238555774, -6.000000000000005329 ) ) ;
#610 = EDGE_CURVE ( 'NONE', #5920, #21964, #16795, .T. ) ;
#611 = CARTESIAN_POINT ( 'NONE',  ( 11.12500000000010658, 1.414213562373201061, 1.414213562373034527 ) ) ;
#612 = EDGE_LOOP ( 'NONE', ( #28143, #13844, #4187, #4536 ) ) ;
#613 = CARTESIAN_POINT ( 'NONE',  ( 135.0000000000000284, 6.735557395310442023E-16, 5.500000000000000000 ) ) ;
#614 = CARTESIAN_POINT ( 'NONE',  ( 2.775557561562891351E-14, 6.250000000000033751, -134.5669872981078470 ) ) ;
#615 = CARTESIAN_POINT ( 'NONE',  ( 116.0000000000000142, 0.000000000000000000, 0.000000000000000000 ) ) ;
#616 = CARTESIAN_POINT ( 'NONE',  ( 3.464101615137852974, 5.999999999999884537, -130.9136751345948539 ) ) ;
#617 = LINE ( 'NONE', #459, #26505 ) ;
#618 = B_SPLINE_CURVE_WITH_KNOTS ( 'NONE', 3,
 ( #5629, #26527, #9972, #878 ),
 .UNSPECIFIED., .F., .F.,
 ( 4, 4 ),
 ( 0.000000000000000000, 0.0004191943366147233034 ),
 .UNSPECIFIED. ) ;
#619 = ORIENTED_EDGE ( 'NONE', *, *, #4595, .F. ) ;
#620 = CARTESIAN_POINT ( 'NONE',  ( 20.75000000000012790, 1.665334536937734811E-13, -2.000000000000001776 ) ) ;
#621 = CARTESIAN_POINT ( 'NONE',  ( 6.000000000000000888, -1.859271017917181981E-14, -135.6636751345948255 ) ) ;
#622 = DIRECTION ( 'NONE',  ( 0.000000000000000000, 0.000000000000000000, 1.000000000000000000 ) ) ;
#623 = CARTESIAN_POINT ( 'NONE',  ( 10.00000000000014744, 1.110223024625156540E-13, -5.551115123125782702E-14 ) ) ;
#624 = CARTESIAN_POINT ( 'NONE',  ( 139.2038997308104058, 2.071067811865468400, 4.999999999999989342 ) ) ;
#625 = CARTESIAN_POINT ( 'NONE',  ( -2.081668171172168020E-16, -5.204170427930420051E-17, 2.499999999999999112 ) ) ;
#626 = CARTESIAN_POINT ( 'NONE',  ( 15.53867513459491967, 1.110223024625156540E-13, 2.499999999999835687 ) ) ;
#627 = DIRECTION ( 'NONE',  ( 1.000000000000000000, 0.000000000000000000, 0.000000000000000000 ) ) ;
#628 = CARTESIAN_POINT ( 'NONE',  ( 107.9999999999998863, 2.500000000000002220, 0.000000000000000000 ) ) ;
#629 = LINE ( 'NONE', #14357, #14784 ) ;
#630 = CARTESIAN_POINT ( 'NONE',  ( 4.763139720814407951, 2.750000000000002665, -139.7500000000000284 ) ) ;
#631 =( NAMED_UNIT ( * ) SI_UNIT ( $, .STERADIAN. ) SOLID_ANGLE_UNIT ( ) );
#632 = CARTESIAN_POINT ( 'NONE',  ( 153.7574251345948539, -2.278174593051795149, 5.500000000000228262 ) ) ;
#633 = EDGE_LOOP ( 'NONE', ( #16313, #27975, #1968, #14002 ) ) ;
#634 = CARTESIAN_POINT ( 'NONE',  ( 3.175426480543072749, -5.500000000000105693, -48.62500000000000711 ) ) ;
#635 = CARTESIAN_POINT ( 'NONE',  ( -3.464101615137725076, 5.999999999999979572, -88.08632486540520290 ) ) ;
#636 = CARTESIAN_POINT ( 'NONE',  ( -3.464101615137757051, -5.999999999999979572, -100.1636751345948113 ) ) ;
#637 = STYLED_ITEM ( 'NONE', ( #9932 ), #15129 ) ;
#638 = EDGE_LOOP ( 'NONE', ( #15445, #9531, #17876, #24636 ) ) ;
#639 = CARTESIAN_POINT ( 'NONE',  ( 116.9997167782375698, -1.308140751793557266, 1.308140751793862577 ) ) ;
#640 = CARTESIAN_POINT ( 'NONE',  ( 118.3511751345946266, 2.000000000000091926, 0.8284271247463557142 ) ) ;
#641 = CARTESIAN_POINT ( 'NONE',  ( 12.06249999999996447, 2.000000000000091926, 0.8284271247461753029 ) ) ;
#642 = EDGE_CURVE ( 'NONE', #1738, #14551, #13017, .T. ) ;
#643 = CARTESIAN_POINT ( 'NONE',  ( 7.216878364870455975, -6.409875621278545621E-14, -95.94198729810780435 ) ) ;
#644 = CARTESIAN_POINT ( 'NONE',  ( 20.46132486540533435, 1.110223024625156540E-13, -2.500000000000057732 ) ) ;
#645 = CARTESIAN_POINT ( 'NONE',  ( 117.5624999999997584, -2.499999999999904521, -1.035533905932508825 ) ) ;
#646 = CARTESIAN_POINT ( 'NONE',  ( 0.000000000000000000, 0.000000000000000000, 0.000000000000000000 ) ) ;
#647 = EDGE_CURVE ( 'NONE', #14487, #18130, #29517, .T. ) ;
#648 = CARTESIAN_POINT ( 'NONE',  ( -6.350852961085760029, -1.281975124255709124E-13, -130.1250000000000284 ) ) ;
#649 = VECTOR ( 'NONE', #7995, 1000.000000000000000 ) ;
#650 = ADVANCED_FACE ( 'NONE', ( #5702 ), #17888, .T. ) ;
#651 = VERTEX_POINT ( 'NONE', #19847 ) ;
#652 = ORIENTED_EDGE ( 'NONE', *, *, #19956, .F. ) ;
#653 = MECHANICAL_DESIGN_GEOMETRIC_PRESENTATION_REPRESENTATION (  '', ( #6546 ), #18839 ) ;
#654 = LINE ( 'NONE', #11769, #4245 ) ;
#655 = CARTESIAN_POINT ( 'NONE',  ( 4.763139720814407951, -2.749999999999988454, -56.00000000000004974 ) ) ;
#656 = DIRECTION ( 'NONE',  ( -7.147005652999508048E-36, 5.642372883946980038E-36, 1.000000000000000000 ) ) ;
#657 = DIRECTION ( 'NONE',  ( 1.000000000000000000, 0.000000000000000000, 0.000000000000000000 ) ) ;
#658 = CARTESIAN_POINT ( 'NONE',  ( -7.216878364870328078, 0.000000000000000000, -82.55801270189220986 ) ) ;
#659 = CARTESIAN_POINT ( 'NONE',  ( -6.000000000000000888, 1.067854986875958443E-15, 7.560779664488942560E-35 ) ) ;
#660 = CARTESIAN_POINT ( 'NONE',  ( 152.7261751345948539, -3.889087296526011706, -3.889087296526011706 ) ) ;
#661 = CARTESIAN_POINT ( 'NONE',  ( -5.196152422706601826, 2.999999999999975131, -79.53867513459483973 ) ) ;
#662 = CARTESIAN_POINT ( 'NONE',  ( 140.3637585460053288, -11.68187927300243345, -4.222310544175148728 ) ) ;
#663 = CARTESIAN_POINT ( 'NONE',  ( 117.1877832217620892, 0.7662911109078287542, -1.849990392679472073 ) ) ;
#664 = CARTESIAN_POINT ( 'NONE',  ( -4.763139720814407951, 2.749999999999946709, -136.2499999999999716 ) ) ;
#665 = CARTESIAN_POINT ( 'NONE',  ( 139.9918614756773536, -8.909704403337718404, 8.038575526839014884 ) ) ;
#666 = DIRECTION ( 'NONE',  ( -7.147005652999508048E-36, 5.642372883946980038E-36, 1.000000000000000000 ) ) ;
#667 = CARTESIAN_POINT ( 'NONE',  ( 6.000000000000000888, 1.743066579297358182E-13, -51.66367513459483263 ) ) ;
#668 = CARTESIAN_POINT ( 'NONE',  ( -2.775557561562891351E-14, -5.500000000000115463, -71.25000000000002842 ) ) ;
#669 = CARTESIAN_POINT ( 'NONE',  ( 0.000000000000000000, 5.999999999999977796, -114.2886751345948397 ) ) ;
#670 = CARTESIAN_POINT ( 'NONE',  ( 3.175426480543072749, 5.499999999999865885, -58.62499999999998579 ) ) ;
#671 = LINE ( 'NONE', #12834, #5698 ) ;
#672 = CARTESIAN_POINT ( 'NONE',  ( 144.2961002691896795, 2.071067811865468400, -4.999999999999989342 ) ) ;
#673 = CARTESIAN_POINT ( 'NONE',  ( 150.0000000000000284, 6.000000000000005329, 0.000000000000000000 ) ) ;
#674 = DIRECTION ( 'NONE',  ( 1.260129944081490070E-35, 5.642372883946978702E-36, 1.000000000000000000 ) ) ;
#675 = CARTESIAN_POINT ( 'NONE',  ( 17.31250000000004263, -0.8284271247461152399, 2.000000000000091926 ) ) ;
#676 = EDGE_CURVE ( 'NONE', #12037, #42, #5973, .T. ) ;
#677 = CARTESIAN_POINT ( 'NONE',  ( -5.196152422706573404, -3.000000000000002665, -58.28867513459484684 ) ) ;
#678 =( LENGTH_UNIT ( ) NAMED_UNIT ( * ) SI_UNIT ( .MILLI., .METRE. ) );
#679 = EDGE_LOOP ( 'NONE', ( #963, #7486, #21683, #27878 ) ) ;
#680 = CARTESIAN_POINT ( 'NONE',  ( 142.3125000000000284, 4.242640687119298093, -4.242640687119298093 ) ) ;
#681 = DIRECTION ( 'NONE',  ( -7.147005652999508048E-36, 5.642372883946980038E-36, 1.000000000000000000 ) ) ;
#682 = B_SPLINE_CURVE_WITH_KNOTS ( 'NONE', 3,
 ( #9797, #28649, #26068, #3010, #25919, #2864, #19176, #7620 ),
 .UNSPECIFIED., .F., .F.,
 ( 4, 2, 2, 4 ),
 ( 0.000000000000000000, 0.0002903981794584280240, 0.0005807963589168560481, 0.001161592717833712096 ),
 .UNSPECIFIED. ) ;
#683 = EDGE_CURVE ( 'NONE', #22336, #13151, #10426, .T. ) ;
#684 = CARTESIAN_POINT ( 'NONE',  ( 112.7886751345947403, -1.999999999999946265, 0.000000000000000000 ) ) ;
#685 =( BOUNDED_CURVE ( )  B_SPLINE_CURVE ( 2, ( #21379, #16796, #14490, #23827, #19664, #24717, #8270, #12486, #26695 ),
 .UNSPECIFIED., .F., .T. ) 
 B_SPLINE_CURVE_WITH_KNOTS ( ( 3, 2, 2, 2, 3 ),
 ( 0.9527777777777778345, 0.9537037037037037202, 0.9555555555555556024, 0.9574074074074073737, 0.9583333333333333703 ),
 .UNSPECIFIED. ) 
 CURVE ( )  GEOMETRIC_REPRESENTATION_ITEM ( )  RATIONAL_B_SPLINE_CURVE ( ( 0.9330127018922194093, 0.9330127018922234061, 1.000000000000000000, 0.8660254037844388186, 1.000000000000000000, 0.8660254037844388186, 1.000000000000000000, 0.9330127018922154125, 0.9330127018922194093 ) ) 
 REPRESENTATION_ITEM ( '' )  );
#686 = CARTESIAN_POINT ( 'NONE',  ( 3.175426480543072749, -5.500000000000105693, -180.6250000000000284 ) ) ;
#687 = CARTESIAN_POINT ( 'NONE',  ( 23.00000000000013145, 2.000000000000168310, 0.000000000000000000 ) ) ;
#688 = VERTEX_POINT ( 'NONE', #17572 ) ;
#689 = CARTESIAN_POINT ( 'NONE',  ( -6.350852961085760029, -1.281975124255709124E-13, -79.12500000000001421 ) ) ;
#690 = CARTESIAN_POINT ( 'NONE',  ( 5.412658773652739619, 3.124999999999988898, -101.1830127018922241 ) ) ;
#691 = VERTEX_POINT ( 'NONE', #5851 ) ;
#692 = DIRECTION ( 'NONE',  ( -0.000000000000000000, 0.000000000000000000, 1.000000000000000000 ) ) ;
#693 = CARTESIAN_POINT ( 'NONE',  ( -4.763139720814407951, 2.749999999999946709, -167.7500000000000000 ) ) ;
#694 = DIRECTION ( 'NONE',  ( 5.551115123125785167E-17, -1.000000000000000000, -8.881784197001256268E-16 ) ) ;
#695 = DIRECTION ( 'NONE',  ( 0.000000000000000000, 0.000000000000000000, -1.000000000000000000 ) ) ;
#696 = CARTESIAN_POINT ( 'NONE',  ( 111.2113248654051176, -1.999999999999946265, 0.000000000000000000 ) ) ;
#697 = CARTESIAN_POINT ( 'NONE',  ( -5.999999999999956479, -1.607695154586745057, -59.26933756729745539 ) ) ;
#698 = PRESENTATION_LAYER_ASSIGNMENT (  '', '', ( #6600 ) ) ;
#699 =( NAMED_UNIT ( * ) SI_UNIT ( $, .STERADIAN. ) SOLID_ANGLE_UNIT ( ) );
#700 = CARTESIAN_POINT ( 'NONE',  ( 4.763139720814407951, -2.749999999999988454, -167.0000000000000284 ) ) ;
#701 = CARTESIAN_POINT ( 'NONE',  ( 0.000000000000000000, -5.999999999999991118, -60.46132486540523132 ) ) ;
#702 = CARTESIAN_POINT ( 'NONE',  ( -2.775557561562891351E-14, -5.500000000000115463, -150.7500000000000568 ) ) ;
#703 = DIRECTION ( 'NONE',  ( 0.000000000000000000, 0.000000000000000000, 1.000000000000000000 ) ) ;
#704 = CARTESIAN_POINT ( 'NONE',  ( -5.196152422706573404, -3.000000000000002665, -52.28867513459483973 ) ) ;
#705 = CARTESIAN_POINT ( 'NONE',  ( 3.175426480543072749, -5.500000000000105693, -98.12500000000004263 ) ) ;
#706 = CARTESIAN_POINT ( 'NONE',  ( -3.175426480542816510, 5.499999999999865885, -89.87500000000001421 ) ) ;
#707 = CARTESIAN_POINT ( 'NONE',  ( 140.0000000000000284, 0.000000000000000000, 0.000000000000000000 ) ) ;
#708 = CARTESIAN_POINT ( 'NONE',  ( 157.4211002691896510, -4.999999999999989342, -2.071067811865468400 ) ) ;
#709 = CARTESIAN_POINT ( 'NONE',  ( 0.000000000000000000, -5.999999999999991118, -136.0386751345948255 ) ) ;
#710 = CARTESIAN_POINT ( 'NONE',  ( 24.87500000000009237, 1.414213562373312083, -1.414213562373145550 ) ) ;
#711 = CARTESIAN_POINT ( 'NONE',  ( 110.8749999999998721, 1.767766952966431937, -1.767766952966209892 ) ) ;
#712 = CARTESIAN_POINT ( 'NONE',  ( 6.000000000000000888, -1.859271017917181981E-14, -88.58632486540523132 ) ) ;
#713 = EDGE_CURVE ( 'NONE', #28274, #9960, #8962, .T. ) ;
#714 = FILL_AREA_STYLE_COLOUR ( '', #23926 ) ;
#715 = CARTESIAN_POINT ( 'NONE',  ( 112.9613248654051461, 5.551115123125782702E-14, 2.000000000000112799 ) ) ;
#716 = EDGE_CURVE ( 'NONE', #15617, #21702, #27616, .T. ) ;
#717 = EDGE_LOOP ( 'NONE', ( #27605, #12662, #17142, #22496 ) ) ;
#718 = CARTESIAN_POINT ( 'NONE',  ( 6.000000000000000888, -3.330669073875464691E-16, -7.560779664488942560E-35 ) ) ;
#719 = CYLINDRICAL_SURFACE ( 'NONE', #14325, 4.000000000000004441 ) ;
#720 = CARTESIAN_POINT ( 'NONE',  ( 119.5002832217621886, 1.308140751793640533, 1.308140751793751555 ) ) ;
#721 = EDGE_LOOP ( 'NONE', ( #24132, #26615, #12517, #1556 ) ) ;
#722 = CARTESIAN_POINT ( 'NONE',  ( 145.5000000000000284, 6.000000000000005329, 0.000000000000000000 ) ) ;
#723 = ORIENTED_EDGE ( 'NONE', *, *, #24077, .F. ) ;
#724 = CARTESIAN_POINT ( 'NONE',  ( -4.763139720814407951, 2.749999999999946709, -106.2500000000000142 ) ) ;
#725 = CARTESIAN_POINT ( 'NONE',  ( 20.18750000000012079, 1.097466725451679892, -2.649519052838238409 ) ) ;
#726 = CARTESIAN_POINT ( 'NONE',  ( 2.775557561562891351E-14, -6.250000000000061284, -122.6830127018922525 ) ) ;
#727 = ORIENTED_EDGE ( 'NONE', *, *, #26320, .T. ) ;
#728 = CARTESIAN_POINT ( 'NONE',  ( 6.000000000000000888, 1.743066579297358182E-13, -111.6636751345948255 ) ) ;
#729 = CARTESIAN_POINT ( 'NONE',  ( 3.608439182435180470, 6.249999999999982236, -157.1919872981078470 ) ) ;
#730 = CARTESIAN_POINT ( 'NONE',  ( 104.8124999999997868, 1.035533905932779275, -2.499999999999904521 ) ) ;
#731 = CARTESIAN_POINT ( 'NONE',  ( -0.4142135623730960892, -9.292893218813460976, 4.000000000000004441 ) ) ;
#732 = TOROIDAL_SURFACE ( 'NONE', #28662, 1.000000000000000000, 0.5000000000000000000 ) ;
#733 = VECTOR ( 'NONE', #24203, 1000.000000000000000 ) ;
#734 =( BOUNDED_CURVE ( )  B_SPLINE_CURVE ( 2, ( #7930, #21493, #12589, #26656, #9808, #28516, #7487, #16897, #14586 ),
 .UNSPECIFIED., .F., .F. ) 
 B_SPLINE_CURVE_WITH_KNOTS ( ( 3, 2, 2, 2, 3 ),
 ( 0.8361111111111110272, 0.8370370370370370239, 0.8388888888888889062, 0.8407407407407407884, 0.8416666666666666741 ),
 .UNSPECIFIED. ) 
 CURVE ( )  GEOMETRIC_REPRESENTATION_ITEM ( )  RATIONAL_B_SPLINE_CURVE ( ( 0.9330127018922194093, 0.9330127018922154125, 1.000000000000000000, 0.8660254037844388186, 1.000000000000000000, 0.8660254037844388186, 1.000000000000000000, 0.9330127018922194093, 0.9330127018922194093 ) ) 
 REPRESENTATION_ITEM ( '' )  );
#735 = CARTESIAN_POINT ( 'NONE',  ( 2.775557561562891351E-14, -6.250000000000061284, -61.18301270189224539 ) ) ;
#736 = ORIENTED_EDGE ( 'NONE', *, *, #27454, .T. ) ;
#737 = CARTESIAN_POINT ( 'NONE',  ( 0.7723847956792433411, -15.49036276797524891, -8.142419924191026226 ) ) ;
#738 = CARTESIAN_POINT ( 'NONE',  ( 158.2574251345948539, -2.278174593051826236, 5.500000000000198064 ) ) ;
#739 = CARTESIAN_POINT ( 'NONE',  ( 116.0000000000000142, 0.000000000000000000, 0.000000000000000000 ) ) ;
#740 = FACE_OUTER_BOUND ( 'NONE', #21778, .T. ) ;
#741 = CARTESIAN_POINT ( 'NONE',  ( 118.5624999999997016, -2.499999999999874767, -1.035533905932568777 ) ) ;
#742 = CARTESIAN_POINT ( 'NONE',  ( -5.999999999999963585, -1.487416814333745711E-14, -113.3363248654052029 ) ) ;
#743 = CARTESIAN_POINT ( 'NONE',  ( -7.216878364870328078, 0.000000000000000000, -166.5580127018922383 ) ) ;
#744 = CARTESIAN_POINT ( 'NONE',  ( 0.000000000000000000, 0.000000000000000000, 0.000000000000000000 ) ) ;
#745 = CARTESIAN_POINT ( 'NONE',  ( -19.99999999999998224, -25.00000000000010658, 5.000000000000004441 ) ) ;
#746 = AXIS2_PLACEMENT_3D ( 'NONE', #18168, #3378, #12804 ) ;
#747 = CARTESIAN_POINT ( 'NONE',  ( 4.763139720814407951, 2.750000000000002665, -115.7500000000000142 ) ) ;
#748 = CARTESIAN_POINT ( 'NONE',  ( -4.763139720814407951, -2.750000000000016431, -114.9999999999999858 ) ) ;
#749 = CARTESIAN_POINT ( 'NONE',  ( -5.999999999999963585, -1.487416814333745711E-14, -88.41367513459482552 ) ) ;
#750 = VERTEX_POINT ( 'NONE', #6178 ) ;
#751 = CARTESIAN_POINT ( 'NONE',  ( 17.06250000000010303, -2.649519052838178457, 1.097466725451559322 ) ) ;
#752 = CARTESIAN_POINT ( 'NONE',  ( 120.3124999999998579, -1.035533905932689347, 2.500000000000205169 ) ) ;
#753 = CARTESIAN_POINT ( 'NONE',  ( 3.464101615137852974, 5.999999999999884537, -109.3363248654052313 ) ) ;
#754 = ADVANCED_FACE ( 'NONE', ( #3547 ), #12979, .T. ) ;
#755 = EDGE_LOOP ( 'NONE', ( #871, #25414, #7664, #11467 ) ) ;
#756 = FILL_AREA_STYLE ('',( #7658 ) ) ;
#757 = CARTESIAN_POINT ( 'NONE',  ( 17.53867513459494987, 1.665334536937734811E-13, 2.499999999999946709 ) ) ;
#758 = CIRCLE ( 'NONE', #17959, 6.500000000000016875 ) ;
#759 = DIRECTION ( 'NONE',  ( 1.000000000000000000, 0.000000000000000000, -0.000000000000000000 ) ) ;
#760 = ORIENTED_EDGE ( 'NONE', *, *, #21946, .T. ) ;
#761 = CARTESIAN_POINT ( 'NONE',  ( 5.196152422706629359, 3.000000000000002665, -144.5386751345948539 ) ) ;
#762 = ORIENTED_EDGE ( 'NONE', *, *, #5312, .T. ) ;
#763 = ORIENTED_EDGE ( 'NONE', *, *, #21634, .T. ) ;
#764 = CARTESIAN_POINT ( 'NONE',  ( 135.3898502691896510, 3.535533905932725318, -3.535533905932725318 ) ) ;
#765 = VERTEX_POINT ( 'NONE', #10655 ) ;
#766 = AXIS2_PLACEMENT_3D ( 'NONE', #22355, #13325, #29562 ) ;
#767 = VECTOR ( 'NONE', #17071, 1000.000000000000000 ) ;
#768 = CARTESIAN_POINT ( 'NONE',  ( -3.608439182435115633, 6.249999999999965361, -131.4419872981078470 ) ) ;
#769 =( LENGTH_UNIT ( ) NAMED_UNIT ( * ) SI_UNIT ( .MILLI., .METRE. ) );
#770 = CARTESIAN_POINT ( 'NONE',  ( 6.000000000000000888, -1.859271017917181981E-14, -84.08632486540520290 ) ) ;
#771 = CARTESIAN_POINT ( 'NONE',  ( -5.999999999999963585, 8.134310703387671600E-14, -116.9136751345948539 ) ) ;
#772 = ORIENTED_EDGE ( 'NONE', *, *, #22651, .T. ) ;
#773 = CARTESIAN_POINT ( 'NONE',  ( 17.00000000000015277, 2.000000000000112799, 0.000000000000000000 ) ) ;
#774 = DIRECTION ( 'NONE',  ( -7.147005652999508048E-36, 5.642372883946980038E-36, 1.000000000000000000 ) ) ;
#775 = CARTESIAN_POINT ( 'NONE',  ( 135.5000000000000284, -9.047800747817580813, -8.000000000000007105 ) ) ;
#776 =( BOUNDED_CURVE ( )  B_SPLINE_CURVE ( 2, ( #18217, #4046, #8982, #16240, #3741, #13175, #17921, #22513, #27535 ),
 .UNSPECIFIED., .F., .T. ) 
 B_SPLINE_CURVE_WITH_KNOTS ( ( 3, 2, 2, 2, 3 ),
 ( 0.7249999999999999778, 0.7259259259259259744, 0.7277777777777777457, 0.7296296296296296280, 0.7305555555555556246 ),
 .UNSPECIFIED. ) 
 CURVE ( )  GEOMETRIC_REPRESENTATION_ITEM ( )  RATIONAL_B_SPLINE_CURVE ( ( 0.9330127018922194093, 0.9330127018922154125, 1.000000000000000000, 0.8660254037844388186, 1.000000000000000000, 0.8660254037844388186, 1.000000000000000000, 0.9330127018922154125, 0.9330127018922194093 ) ) 
 REPRESENTATION_ITEM ( '' )  );
#777 = CARTESIAN_POINT ( 'NONE',  ( 139.7663997308104342, -4.999999999999989342, -2.071067811865468400 ) ) ;
#778 = CARTESIAN_POINT ( 'NONE',  ( 0.000000000000000000, 0.000000000000000000, 0.000000000000000000 ) ) ;
#779 = DIRECTION ( 'NONE',  ( 1.000000000000000000, -0.000000000000000000, 0.000000000000000000 ) ) ;
#780 = ADVANCED_FACE ( 'NONE', ( #10194 ), #11219, .F. ) ;
#781 = CARTESIAN_POINT ( 'NONE',  ( 6.000000000000052403, -1.607695154586662678, -162.1533121635129646 ) ) ;
#782 = CARTESIAN_POINT ( 'NONE',  ( -0.5000000000000004441, -15.50000000000001421, 7.500000000000007105 ) ) ;
#783 = CARTESIAN_POINT ( 'NONE',  ( 104.5624999999997442, -2.499999999999934719, -1.035533905932689347 ) ) ;
#784 = FACE_OUTER_BOUND ( 'NONE', #24987, .T. ) ;
#785 = CARTESIAN_POINT ( 'NONE',  ( 6.350852961086080661, -9.614813431917819062E-14, -138.3750000000000568 ) ) ;
#786 = CARTESIAN_POINT ( 'NONE',  ( 0.8631338372297875372, -15.37878787878788067, -8.351220472436777342 ) ) ;
#787 = ORIENTED_EDGE ( 'NONE', *, *, #30306, .T. ) ;
#788 = CARTESIAN_POINT ( 'NONE',  ( -6.000000000000000888, 1.067854986875958443E-15, 7.560779664488942560E-35 ) ) ;
#789 = DIRECTION ( 'NONE',  ( 1.000000000000000000, 0.000000000000000000, 0.000000000000000000 ) ) ;
#790 = ADVANCED_FACE ( 'NONE', ( #29667 ), #8635, .T. ) ;
#791 = ORIENTED_EDGE ( 'NONE', *, *, #29842, .T. ) ;
#792 = CARTESIAN_POINT ( 'NONE',  ( 118.7497167782375982, 1.308140751793696044, 1.308140751793640533 ) ) ;
#793 = DIRECTION ( 'NONE',  ( -7.147005652999508048E-36, 5.642372883946980038E-36, 1.000000000000000000 ) ) ;
#794 = CARTESIAN_POINT ( 'NONE',  ( 2.775557561562891351E-14, -6.250000000000061284, -91.81698729810783277 ) ) ;
#795 = CARTESIAN_POINT ( 'NONE',  ( 13.99999999999999822, 0.000000000000000000, 0.000000000000000000 ) ) ;
#796 = CARTESIAN_POINT ( 'NONE',  ( 114.2499999999999147, -1.110223024625156540E-13, 2.500000000000057732 ) ) ;
#797 = CARTESIAN_POINT ( 'NONE',  ( 140.4831164018241338, -11.48311640182299698, 4.126236462591083232 ) ) ;
#798 = CARTESIAN_POINT ( 'NONE',  ( -4.763139720814407951, -2.750000000000016431, -130.0000000000000000 ) ) ;
#799 = VERTEX_POINT ( 'NONE', #16 ) ;
#800 = EDGE_LOOP ( 'NONE', ( #8417, #10263, #10021, #8901 ) ) ;
#801 = PRESENTATION_LAYER_ASSIGNMENT (  '', '', ( #18016 ) ) ;
#802 = CARTESIAN_POINT ( 'NONE',  ( 159.0000000000000284, -11.07692307692306777, 4.615384615384604317 ) ) ;
#803 = CARTESIAN_POINT ( 'NONE',  ( -3.175426480542816510, 5.499999999999865885, -53.87500000000003553 ) ) ;
#804 = CARTESIAN_POINT ( 'NONE',  ( -6.000000000000007105, -1.607695154586655129, -51.76933756729743408 ) ) ;
#805 = CARTESIAN_POINT ( 'NONE',  ( 3.682280293032525798, 10.37087330740121516, -29.75307074678472219 ) ) ;
#806 = CARTESIAN_POINT ( 'NONE',  ( -3.608439182435052128, -6.250000000000110134, -73.30801270189222407 ) ) ;
#807 = DIRECTION ( 'NONE',  ( -1.000000000000000000, 0.000000000000000000, 0.000000000000000000 ) ) ;
#808 = CARTESIAN_POINT ( 'NONE',  ( 0.000000000000000000, 0.000000000000000000, -183.0000000000000000 ) ) ;
#809 = EDGE_CURVE ( 'NONE', #26790, #13355, #14385, .T. ) ;
#810 = CARTESIAN_POINT ( 'NONE',  ( 3.175426480543072749, -5.500000000000105693, -141.6250000000000000 ) ) ;
#811 = CARTESIAN_POINT ( 'NONE',  ( 140.5000000000000000, -9.600000000000008527, 7.199999999999995737 ) ) ;
#812 = CARTESIAN_POINT ( 'NONE',  ( -7.216878364870328078, 0.000000000000000000, -156.0580127018922383 ) ) ;
#813 = CARTESIAN_POINT ( 'NONE',  ( 0.000000000000000000, 5.499999999999991118, -70.50000000000000000 ) ) ;
#814 = ADVANCED_FACE ( 'NONE', ( #25673 ), #14053, .T. ) ;
#815 = CARTESIAN_POINT ( 'NONE',  ( -6.350852961085760029, -1.281975124255709124E-13, -61.12500000000000711 ) ) ;
#816 = ORIENTED_EDGE ( 'NONE', *, *, #14649, .T. ) ;
#817 = CARTESIAN_POINT ( 'NONE',  ( 142.0461002691896795, -2.071067811865468400, 4.999999999999989342 ) ) ;
#818 = CARTESIAN_POINT ( 'NONE',  ( 152.3437500000000853, -6.000000000000005329, -2.485281374238556218 ) ) ;
#819 = CARTESIAN_POINT ( 'NONE',  ( 6.000000000000000888, 7.762456499804234384E-14, -127.5863248654052171 ) ) ;
#820 = VECTOR ( 'NONE', #10037, 1000.000000000000000 ) ;
#821 = DIRECTION ( 'NONE',  ( -1.000000000000000000, -1.665334536937736783E-16, -2.220446049250315546E-16 ) ) ;
#822 = CIRCLE ( 'NONE', #18037, 10.49999999999999822 ) ;
#823 = ORIENTED_EDGE ( 'NONE', *, *, #13344, .F. ) ;
#824 = CARTESIAN_POINT ( 'NONE',  ( 141.8437500000000284, -6.000000000000005329, -2.485281374238555774 ) ) ;
#825 = LINE ( 'NONE', #21591, #17050 ) ;
#826 = COLOUR_RGB ( '', 0.31764706, 0.68627451, 0.89019608) ;
#827 = CARTESIAN_POINT ( 'NONE',  ( -4.999999999999990230, -9.165151389911669000, -8.000000000000007105 ) ) ;
#828 = CARTESIAN_POINT ( 'NONE',  ( 3.175426480543072749, -5.500000000000105693, -177.6250000000000284 ) ) ;
#829 = CARTESIAN_POINT ( 'NONE',  ( 17.06250000000001066, 2.000000000000151879, 0.8284271247461753029 ) ) ;
#830 = CARTESIAN_POINT ( 'NONE',  ( 2.775557561562891351E-14, 6.250000000000033751, -155.5669872981078186 ) ) ;
#831 = FILL_AREA_STYLE_COLOUR ( '', #193 ) ;
#832 = CARTESIAN_POINT ( 'NONE',  ( 3.175426480543072749, 5.499999999999865885, -79.62500000000002842 ) ) ;
#833 = CARTESIAN_POINT ( 'NONE',  ( 15.50000000000023626, 1.873492889145123019, 1.873492889144845464 ) ) ;
#834 = CARTESIAN_POINT ( 'NONE',  ( 0.000000000000000000, 11.00000000000001066, 4.000000000000003553 ) ) ;
#835 = EDGE_CURVE ( 'NONE', #29880, #28765, #16801, .T. ) ;
#836 = DIRECTION ( 'NONE',  ( 0.000000000000000000, 0.000000000000000000, 1.000000000000000000 ) ) ;
#837 = CARTESIAN_POINT ( 'NONE',  ( 2.676951800742168933E-14, -11.00000000000000000, -19.00000000000002132 ) ) ;
#838 = CARTESIAN_POINT ( 'NONE',  ( -20.99999999999998224, -54.99999999999990763, -5.000000000000004441 ) ) ;
#839 = CARTESIAN_POINT ( 'NONE',  ( -2.775557561562891351E-14, -5.500000000000115463, -162.7500000000000000 ) ) ;
#840 = CARTESIAN_POINT ( 'NONE',  ( -5.999999999999963585, 1.780251999655701777E-13, -70.41367513459482552 ) ) ;
#841 = CARTESIAN_POINT ( 'NONE',  ( 3.175426480543072749, -5.500000000000105693, -144.6250000000000000 ) ) ;
#842 = CARTESIAN_POINT ( 'NONE',  ( 135.0000000000000284, 6.000000000000005329, 0.000000000000000000 ) ) ;
#843 = CARTESIAN_POINT ( 'NONE',  ( 3.175426480543072749, 5.499999999999865885, -91.62500000000001421 ) ) ;
#844 = LINE ( 'NONE', #12869, #23611 ) ;
#845 = EDGE_CURVE ( 'NONE', #8188, #25843, #3483, .T. ) ;
#846 =( BOUNDED_CURVE ( )  B_SPLINE_CURVE ( 2, ( #18304, #29786, #27617, #4440, #13865, #23205, #26380, #5028, #14738 ),
 .UNSPECIFIED., .F., .F. ) 
 B_SPLINE_CURVE_WITH_KNOTS ( ( 3, 2, 2, 2, 3 ),
 ( 0.7694444444444443754, 0.7703703703703703720, 0.7722222222222222543, 0.7740740740740741366, 0.7750000000000000222 ),
 .UNSPECIFIED. ) 
 CURVE ( )  GEOMETRIC_REPRESENTATION_ITEM ( )  RATIONAL_B_SPLINE_CURVE ( ( 0.9330127018922194093, 0.9330127018922154125, 1.000000000000000000, 0.8660254037844388186, 1.000000000000000000, 0.8660254037844388186, 1.000000000000000000, 0.9330127018922194093, 0.9330127018922194093 ) ) 
 REPRESENTATION_ITEM ( '' )  );
#847 = CARTESIAN_POINT ( 'NONE',  ( -6.350852961085760029, -1.281975124255709124E-13, -82.12500000000004263 ) ) ;
#848 = CARTESIAN_POINT ( 'NONE',  ( -3.464101615137725076, 5.999999999999979572, -143.5863248654052029 ) ) ;
#849 = AXIS2_PLACEMENT_3D ( 'NONE', #28828, #17055, #25940 ) ;
#850 = DIRECTION ( 'NONE',  ( 0.000000000000000000, 0.000000000000000000, -1.000000000000000000 ) ) ;
#851 = CARTESIAN_POINT ( 'NONE',  ( 113.0863248654050892, -1.414213562373173305, 1.414213562373145550 ) ) ;
#852 =( BOUNDED_CURVE ( )  B_SPLINE_CURVE ( 2, ( #24151, #4805, #2504, #29351, #26590, #5848, #8314, #29192, #17722 ),
 .UNSPECIFIED., .F., .T. ) 
 B_SPLINE_CURVE_WITH_KNOTS ( ( 3, 2, 2, 2, 3 ),
 ( 0.2624999999999988454, 0.2687499999999991562, 0.2749999999999993561, 0.2812499999999996114, 0.2874999999999998113 ),
 .UNSPECIFIED. ) 
 CURVE ( )  GEOMETRIC_REPRESENTATION_ITEM ( )  RATIONAL_B_SPLINE_CURVE ( ( 1.000000000000013545, 0.9238795325112731938, 1.000000000000000000, 0.9238795325112867385, 1.000000000000000000, 0.9238795325112867385, 1.000000000000000000, 0.9238795325112887369, 0.9999999999999980016 ) ) 
 REPRESENTATION_ITEM ( '' )  );
#853 = ORIENTED_EDGE ( 'NONE', *, *, #6435, .T. ) ;
#854 = DIRECTION ( 'NONE',  ( -7.147005652999508048E-36, 5.642372883946980038E-36, 1.000000000000000000 ) ) ;
#855 = CARTESIAN_POINT ( 'NONE',  ( 0.000000000000000000, 0.000000000000000000, 0.000000000000000000 ) ) ;
#856 = VERTEX_POINT ( 'NONE', #23833 ) ;
#857 = MECHANICAL_DESIGN_GEOMETRIC_PRESENTATION_REPRESENTATION (  '', ( #20483 ), #28806 ) ;
#858 = CARTESIAN_POINT ( 'NONE',  ( 147.3750000000000284, 0.000000000000000000, 6.000000000000005329 ) ) ;
#859 = ORIENTED_EDGE ( 'NONE', *, *, #13108, .T. ) ;
#860 = CARTESIAN_POINT ( 'NONE',  ( -6.350852961085760029, -1.281975124255709124E-13, -109.1250000000000426 ) ) ;
#861 = CARTESIAN_POINT ( 'NONE',  ( 18.81250000000011013, -2.649519052838178457, 1.097466725451379244 ) ) ;
#862 = CARTESIAN_POINT ( 'NONE',  ( 7.216878364870455975, -6.409875621278545621E-14, -123.8080127018922099 ) ) ;
#863 = CARTESIAN_POINT ( 'NONE',  ( -3.464101615137725076, 5.999999999999979572, -111.1636751345948113 ) ) ;
#864 = CARTESIAN_POINT ( 'NONE',  ( -5.412658773652684552, -3.125000000000099920, -158.0669872981078754 ) ) ;
#865 = DIRECTION ( 'NONE',  ( -1.000000000000000000, -1.665334536937736783E-16, -2.220446049250315546E-16 ) ) ;
#866 = VECTOR ( 'NONE', #30376, 1000.000000000000000 ) ;
#867 = CARTESIAN_POINT ( 'NONE',  ( 147.0074251345948539, 2.278174593052012309, -5.500000000000012434 ) ) ;
#868 =( GEOMETRIC_REPRESENTATION_CONTEXT ( 3 ) GLOBAL_UNCERTAINTY_ASSIGNED_CONTEXT ( ( #5005 ) ) GLOBAL_UNIT_ASSIGNED_CONTEXT ( ( #1107, #10205, #8488 ) ) REPRESENTATION_CONTEXT ( 'NONE', 'WORKASPACE' ) );
#869 = ADVANCED_FACE ( 'NONE', ( #2769 ), #23688, .T. ) ;
#870 = CARTESIAN_POINT ( 'NONE',  ( 3.608439182435180470, 6.249999999999982236, -56.05801270189221697 ) ) ;
#871 = ORIENTED_EDGE ( 'NONE', *, *, #20566, .F. ) ;
#872 = DIRECTION ( 'NONE',  ( 1.000000000000000000, 1.067522139062651411E-16, -0.000000000000000000 ) ) ;
#873 = EDGE_CURVE ( 'NONE', #26117, #9617, #18488, .T. ) ;
#874 = DIRECTION ( 'NONE',  ( 1.000000000000000000, 1.067522139062651904E-16, -0.000000000000000000 ) ) ;
#875 = CARTESIAN_POINT ( 'NONE',  ( 0.000000000000000000, 5.999999999999977796, -137.7113248654052029 ) ) ;
#876 = CARTESIAN_POINT ( 'NONE',  ( 3.175426480543072749, -5.500000000000105693, -173.1250000000000284 ) ) ;
#877 = CARTESIAN_POINT ( 'NONE',  ( 105.0627832217622455, -0.7662911109076785410, -1.849990392679411677 ) ) ;
#878 = CARTESIAN_POINT ( 'NONE',  ( 0.000000000000000000, -14.14213562373095634, 8.500000000000007105 ) ) ;
#879 = CARTESIAN_POINT ( 'NONE',  ( 7.216878364870455975, -6.409875621278545621E-14, -167.3080127018922951 ) ) ;
#880 = CARTESIAN_POINT ( 'NONE',  ( 160.0000000000000284, -59.99999999999980105, 4.000000000000003553 ) ) ;
#881 = DIRECTION ( 'NONE',  ( -1.000000000000000000, -1.665334536937731113E-16, 1.526556658859586792E-16 ) ) ;
#882 = CARTESIAN_POINT ( 'NONE',  ( -3.175426480542816066, 5.499999999999865885, -119.8750000000000284 ) ) ;
#883 = DIRECTION ( 'NONE',  ( -1.000000000000000000, -1.665334536937736783E-16, -2.220446049250315546E-16 ) ) ;
#884 = CARTESIAN_POINT ( 'NONE',  ( -2.775557561562891351E-14, -5.500000000000115463, -105.7500000000000142 ) ) ;
#885 = CARTESIAN_POINT ( 'NONE',  ( -5.196152422706601826, 2.999999999999975131, -100.5386751345947971 ) ) ;
#886 = VERTEX_POINT ( 'NONE', #10157 ) ;
#887 = CARTESIAN_POINT ( 'NONE',  ( 19.18750000000007461, -2.649519052838178457, -1.097466725451499370 ) ) ;
#888 = CARTESIAN_POINT ( 'NONE',  ( 119.9999999999999289, 2.500000000000057732, 1.110223024625156540E-13 ) ) ;
#889 = CARTESIAN_POINT ( 'NONE',  ( -5.999999999999963585, 1.780251999655701777E-13, -104.3363248654052313 ) ) ;
#890 = CARTESIAN_POINT ( 'NONE',  ( 0.000000000000000000, 5.999999999999977796, -86.71132486540523132 ) ) ;
#891 = VERTEX_POINT ( 'NONE', #3355 ) ;
#892 = CARTESIAN_POINT ( 'NONE',  ( 5.196152422706629359, -2.999999999999988898, -126.7886751345948539 ) ) ;
#893 = CARTESIAN_POINT ( 'NONE',  ( -7.216878364870328078, 0.000000000000000000, -84.69198729810781856 ) ) ;
#894 = FILL_AREA_STYLE ('',( #9836 ) ) ;
#895 = ORIENTED_EDGE ( 'NONE', *, *, #26464, .T. ) ;
#896 = DIRECTION ( 'NONE',  ( -1.000000000000000000, 6.938893903907222067E-15, 0.000000000000000000 ) ) ;
#897 = ORIENTED_EDGE ( 'NONE', *, *, #14049, .F. ) ;
#898 = CARTESIAN_POINT ( 'NONE',  ( 134.5461002691896510, -2.071067811865468400, 4.999999999999989342 ) ) ;
#899 = VERTEX_POINT ( 'NONE', #10460 ) ;
#900 = CARTESIAN_POINT ( 'NONE',  ( 5.412658773652712085, -3.125000000000086153, -127.5669872981078328 ) ) ;
#901 = FILL_AREA_STYLE_COLOUR ( '', #10334 ) ;
#902 = CARTESIAN_POINT ( 'NONE',  ( 161.0000000000000284, 0.000000000000000000, 0.000000000000000000 ) ) ;
#903 = CARTESIAN_POINT ( 'NONE',  ( 143.9136751345948539, 0.000000000000000000, -5.500000000000005329 ) ) ;
#904 = EDGE_LOOP ( 'NONE', ( #7851, #19174, #4581, #7003 ) ) ;
#905 = DIRECTION ( 'NONE',  ( -1.000000000000000000, -6.938893903907222067E-15, 0.000000000000000000 ) ) ;
#906 = CARTESIAN_POINT ( 'NONE',  ( -4.999999999999990230, -55.00000000000002132, 8.000000000000007105 ) ) ;
#907 = EDGE_CURVE ( 'NONE', #26173, #21329, #8122, .T. ) ;
#908 = CYLINDRICAL_SURFACE ( 'NONE', #11806, 6.000000000000000888 ) ;
#909 = CARTESIAN_POINT ( 'NONE',  ( 137.9851497308104058, -3.535533905932725318, 3.535533905932725318 ) ) ;
#910 = CARTESIAN_POINT ( 'NONE',  ( 137.8050748654052597, 5.500000000000012434, 2.278174593052012309 ) ) ;
#911 = CARTESIAN_POINT ( 'NONE',  ( -3.464101615137757051, -5.999999999999979572, -47.08632486540521001 ) ) ;
#912 = CARTESIAN_POINT ( 'NONE',  ( 2.775557561562891351E-14, 6.250000000000033751, -68.56698729810784698 ) ) ;
#913 =( LENGTH_UNIT ( ) NAMED_UNIT ( * ) SI_UNIT ( .MILLI., .METRE. ) );
#914 = CARTESIAN_POINT ( 'NONE',  ( 107.8124999999997442, 1.035533905932809473, -2.499999999999784173 ) ) ;
#915 = FACE_OUTER_BOUND ( 'NONE', #16215, .T. ) ;
#916 = CARTESIAN_POINT ( 'NONE',  ( -3.175426480542816510, -5.500000000000057732, -135.8750000000000284 ) ) ;
#917 = DIRECTION ( 'NONE',  ( 1.000000000000000000, -0.000000000000000000, -0.000000000000000000 ) ) ;
#918 = CARTESIAN_POINT ( 'NONE',  ( 104.7401757384975980, 1.479039993424821287, -1.137087370475787784 ) ) ;
#919 = ORIENTED_EDGE ( 'NONE', *, *, #28096, .T. ) ;
#920 = CARTESIAN_POINT ( 'NONE',  ( 13.08632486540528461, -1.767766952966265404, 1.767766952966320915 ) ) ;
#921 = CARTESIAN_POINT ( 'NONE',  ( -4.763139720814407951, 2.749999999999946709, -47.75000000000001421 ) ) ;
#922 = FACE_OUTER_BOUND ( 'NONE', #3937, .T. ) ;
#923 = CARTESIAN_POINT ( 'NONE',  ( -6.000000000000000888, 1.067854986875958443E-15, 7.560779664488942560E-35 ) ) ;
#924 = STYLED_ITEM ( 'NONE', ( #25837 ), #14331 ) ;
#925 = ORIENTED_EDGE ( 'NONE', *, *, #18609, .T. ) ;
#926 = CARTESIAN_POINT ( 'NONE',  ( 112.8122167782374419, 0.7662911109079189043, 1.849990392679772278 ) ) ;
#927 = CARTESIAN_POINT ( 'NONE',  ( 136.5000000000000284, 6.000000000000005329, 0.000000000000000000 ) ) ;
#928 = CARTESIAN_POINT ( 'NONE',  ( -7.216878364870328078, 0.000000000000000000, -95.19198729810780435 ) ) ;
#929 = FACE_OUTER_BOUND ( 'NONE', #23458, .T. ) ;
#930 = CARTESIAN_POINT ( 'NONE',  ( 11.21132486540529705, -2.499999999999891198, -5.551115123125782702E-14 ) ) ;
#931 = CARTESIAN_POINT ( 'NONE',  ( 115.8749999999998579, 1.767766952966431937, -1.767766952966320915 ) ) ;
#932 = CARTESIAN_POINT ( 'NONE',  ( 140.6451377260904678, -11.29027545218218087, 4.288736938852112601 ) ) ;
#933 = EDGE_CURVE ( 'NONE', #5714, #6341, #12785, .T. ) ;
#934 =( BOUNDED_CURVE ( )  B_SPLINE_CURVE ( 2, ( #21772, #10103, #29104, #3305, #19474, #12731, #22070, #10405, #17478 ),
 .UNSPECIFIED., .F., .T. ) 
 B_SPLINE_CURVE_WITH_KNOTS ( ( 3, 2, 2, 2, 3 ),
 ( 0.7305555555555556246, 0.7314814814814815103, 0.7333333333333332815, 0.7351851851851851638, 0.7361111111111110494 ),
 .UNSPECIFIED. ) 
 CURVE ( )  GEOMETRIC_REPRESENTATION_ITEM ( )  RATIONAL_B_SPLINE_CURVE ( ( 0.9330127018922194093, 0.9330127018922234061, 1.000000000000000000, 0.8660254037844388186, 1.000000000000000000, 0.8660254037844388186, 1.000000000000000000, 0.9330127018922234061, 0.9330127018922194093 ) ) 
 REPRESENTATION_ITEM ( '' )  );
#935 = CARTESIAN_POINT ( 'NONE',  ( 25.25000000000015987, 1.873492889145067508, -1.873492889144956486 ) ) ;
#936 = ORIENTED_EDGE ( 'NONE', *, *, #2428, .F. ) ;
#937 = DIRECTION ( 'NONE',  ( -8.326672684688675286E-17, -2.081668171172168821E-17, 1.000000000000000000 ) ) ;
#938 = CARTESIAN_POINT ( 'NONE',  ( -4.763139720814407951, -2.750000000000016431, -56.49999999999999289 ) ) ;
#939 = AXIS2_PLACEMENT_3D ( 'NONE', #2581, #2142, #18442 ) ;
#940 = FACE_OUTER_BOUND ( 'NONE', #9045, .T. ) ;
#941 = FACE_OUTER_BOUND ( 'NONE', #3694, .T. ) ;
#942 = CARTESIAN_POINT ( 'NONE',  ( -5.412658773652739619, 3.124999999999975131, -78.18301270189220986 ) ) ;
#943 = ADVANCED_FACE ( 'NONE', ( #22128 ), #15230, .F. ) ;
#944 = CARTESIAN_POINT ( 'NONE',  ( 116.3363248654050608, -1.414213562373201061, -1.414213562373034527 ) ) ;
#945 = CARTESIAN_POINT ( 'NONE',  ( 157.2976497308104342, 0.000000000000000000, 5.000000000000004441 ) ) ;
#946 = DIRECTION ( 'NONE',  ( -7.147005652999508048E-36, 5.642372883946980038E-36, 1.000000000000000000 ) ) ;
#947 = CARTESIAN_POINT ( 'NONE',  ( 0.000000000000000000, 5.999999999999977796, -104.7113248654052455 ) ) ;
#948 = CARTESIAN_POINT ( 'NONE',  ( 3.175426480543072749, -5.500000000000105693, -129.6250000000000284 ) ) ;
#949 = CARTESIAN_POINT ( 'NONE',  ( 135.5000000000000000, -54.99999999999993605, 8.000000000000007105 ) ) ;
#950 = CARTESIAN_POINT ( 'NONE',  ( 139.8824251345948539, 5.500000000000012434, 2.278174593052012309 ) ) ;
#951 = CARTESIAN_POINT ( 'NONE',  ( 5.196152422706629359, 3.000000000000002665, -51.53867513459481131 ) ) ;
#952 = CARTESIAN_POINT ( 'NONE',  ( -3.175426480542816066, 5.499999999999865885, -71.87500000000000000 ) ) ;
#953 = FACE_OUTER_BOUND ( 'NONE', #5363, .T. ) ;
#954 = CARTESIAN_POINT ( 'NONE',  ( 6.350852961086080661, -9.614813431917819062E-14, -55.87500000000003553 ) ) ;
#955 = CARTESIAN_POINT ( 'NONE',  ( 136.0000000000000284, 0.000000000000000000, 0.000000000000000000 ) ) ;
#956 = VERTEX_POINT ( 'NONE', #3206 ) ;
#957 = CARTESIAN_POINT ( 'NONE',  ( 138.8586002691896226, 2.071067811865468400, 4.999999999999989342 ) ) ;
#958 = CARTESIAN_POINT ( 'NONE',  ( 151.1250000000000284, 0.000000000000000000, -6.000000000000005329 ) ) ;
#959 = CARTESIAN_POINT ( 'NONE',  ( 0.000000000000000000, 5.999999999999977796, -97.78867513459482552 ) ) ;
#960 = AXIS2_PLACEMENT_3D ( 'NONE', #4048, #22201, #11151 ) ;
#961 = CARTESIAN_POINT ( 'NONE',  ( -5.999999999999963585, -1.487416814333745711E-14, -167.9136751345948255 ) ) ;
#962 = CARTESIAN_POINT ( 'NONE',  ( 114.3122167782374419, -0.7662911109077388261, -1.849990392679231599 ) ) ;
#963 = ORIENTED_EDGE ( 'NONE', *, *, #30074, .T. ) ;
#964 = PRESENTATION_LAYER_ASSIGNMENT (  '', '', ( #10316 ) ) ;
#965 = CARTESIAN_POINT ( 'NONE',  ( 146.0625000000000284, -4.242640687119298093, 4.242640687119298093 ) ) ;
#966 = CARTESIAN_POINT ( 'NONE',  ( -4.999999999999920952, -65.00000000000001421, 7.500000000000007105 ) ) ;
#967 = AXIS2_PLACEMENT_3D ( 'NONE', #10942, #18012, #27929 ) ;
#968 = ADVANCED_FACE ( 'NONE', ( #1786 ), #908, .T. ) ;
#969 = CYLINDRICAL_SURFACE ( 'NONE', #5964, 6.000000000000000888 ) ;
#970 = CARTESIAN_POINT ( 'NONE',  ( -3.175426480542816510, -5.500000000000057732, -176.3750000000000284 ) ) ;
#971 = CARTESIAN_POINT ( 'NONE',  ( 18.12500000000000355, 1.414213562373090038, 1.414213562373090038 ) ) ;
#972 = CARTESIAN_POINT ( 'NONE',  ( -5.412658773652739619, 3.124999999999975131, -147.8169872981078186 ) ) ;
#973 = SURFACE_SIDE_STYLE ('',( #7890 ) ) ;
#974 = CARTESIAN_POINT ( 'NONE',  ( 4.763139720814407951, 2.750000000000002665, -82.74999999999998579 ) ) ;
#975 = ADVANCED_FACE ( 'NONE', ( #5513 ), #10306, .T. ) ;
#976 = CARTESIAN_POINT ( 'NONE',  ( 2.775557561562891351E-14, 6.250000000000033751, -91.93301270189225249 ) ) ;
#977 = EDGE_CURVE ( 'NONE', #23810, #29031, #4696, .T. ) ;
#978 = ORIENTED_EDGE ( 'NONE', *, *, #13835, .F. ) ;
#979 = ADVANCED_FACE ( 'NONE', ( #10082 ), #9930, .F. ) ;
#980 = CARTESIAN_POINT ( 'NONE',  ( 120.0000000000000000, 1.338994316744045454, 1.808804601853416072 ) ) ;
#981 = DIRECTION ( 'NONE',  ( -8.326672684688675286E-17, -2.081668171172168821E-17, 1.000000000000000000 ) ) ;
#982 = DIRECTION ( 'NONE',  ( 1.000000000000000000, -5.551115123125773458E-17, -1.260129944081490338E-35 ) ) ;
#983 = CARTESIAN_POINT ( 'NONE',  ( 135.0000000000000284, -7.170817622374790368, -8.464363312639777703 ) ) ;
#984 = PLANE ( 'NONE',  #25487 ) ;
#985 = CARTESIAN_POINT ( 'NONE',  ( 4.763139720814407951, -2.749999999999988454, -165.4999999999999716 ) ) ;
#986 = CARTESIAN_POINT ( 'NONE',  ( 137.3363248654052029, 0.000000000000000000, -5.500000000000005329 ) ) ;
#987 = CARTESIAN_POINT ( 'NONE',  ( 3.175426480543072749, 5.499999999999865885, -145.6250000000000284 ) ) ;
#988 = CARTESIAN_POINT ( 'NONE',  ( 117.0386751345946692, 5.551115123125782702E-14, -2.000000000000001776 ) ) ;
#989 = CARTESIAN_POINT ( 'NONE',  ( 0.000000000000000000, 0.000000000000000000, 0.000000000000000000 ) ) ;
#990 = CARTESIAN_POINT ( 'NONE',  ( -3.175426480542816066, 5.499999999999865885, -94.37500000000002842 ) ) ;
#991 = DIRECTION ( 'NONE',  ( 1.000000000000000000, -0.000000000000000000, -0.000000000000000000 ) ) ;
#992 = CARTESIAN_POINT ( 'NONE',  ( 0.000000000000000000, 5.499999999999991118, -78.00000000000001421 ) ) ;
#993 = CARTESIAN_POINT ( 'NONE',  ( 0.000000000000000000, 0.000000000000000000, 0.000000000000000000 ) ) ;
#994 = CARTESIAN_POINT ( 'NONE',  ( 6.000000000000000888, -1.607695154586752384, -72.15331216351299304 ) ) ;
#995 = CARTESIAN_POINT ( 'NONE',  ( 6.000000000000052403, -1.607695154586662678, -108.1533121635129362 ) ) ;
#996 = CARTESIAN_POINT ( 'NONE',  ( 18.21132486540530238, -2.499999999999835687, -2.220446049250313081E-13 ) ) ;
#997 = CARTESIAN_POINT ( 'NONE',  ( 10.77382486540524376, 2.499999999999964473, 1.035533905932689347 ) ) ;
#998 = CARTESIAN_POINT ( 'NONE',  ( -1.110223024625164676E-16, 2.000000000000012879, 2.021286199229734960E-15 ) ) ;
#999 = ORIENTED_EDGE ( 'NONE', *, *, #22038, .F. ) ;
#1000 = CARTESIAN_POINT ( 'NONE',  ( 160.1250000000000568, 0.000000000000000000, -6.000000000000005329 ) ) ;
#1001 = DIRECTION ( 'NONE',  ( 1.000000000000000000, 0.000000000000000000, 0.000000000000000000 ) ) ;
#1002 = CARTESIAN_POINT ( 'NONE',  ( 6.000000000000000888, 1.743066579297358182E-13, -78.66367513459482552 ) ) ;
#1003 = CARTESIAN_POINT ( 'NONE',  ( 120.3127832217622171, 1.849990392679591977, -0.7662911109075883909 ) ) ;
#1004 = ADVANCED_FACE ( 'NONE', ( #16866, #5585 ), #5138, .F. ) ;
#1005 = VECTOR ( 'NONE', #25347, 1000.000000000000000 ) ;
#1006 = ORIENTED_EDGE ( 'NONE', *, *, #436, .T. ) ;
#1007 = AXIS2_PLACEMENT_3D ( 'NONE', #11830, #2700, #14140 ) ;
#1008 = CARTESIAN_POINT ( 'NONE',  ( 147.2812500000000284, 2.485281374238585972, 6.000000000000005329 ) ) ;
#1009 = ORIENTED_EDGE ( 'NONE', *, *, #24041, .F. ) ;
#1010 = CARTESIAN_POINT ( 'NONE',  ( -2.775557561562891351E-14, -5.500000000000115463, -102.7500000000000142 ) ) ;
#1011 = EDGE_CURVE ( 'NONE', #22693, #15450, #2747, .T. ) ;
#1012 = CARTESIAN_POINT ( 'NONE',  ( 7.216878364870455975, -6.409875621278545621E-14, -116.3080127018922383 ) ) ;
#1013 = EDGE_CURVE ( 'NONE', #6421, #8510, #3135, .T. ) ;
#1014 = ORIENTED_EDGE ( 'NONE', *, *, #14291, .F. ) ;
#1015 = CARTESIAN_POINT ( 'NONE',  ( 3.464101615137852974, 5.999999999999884537, -111.4136751345948113 ) ) ;
#1016 = CARTESIAN_POINT ( 'NONE',  ( -3.608439182435115633, 6.249999999999965361, -158.4419872981077901 ) ) ;
#1017 = CARTESIAN_POINT ( 'NONE',  ( 105.6874999999997442, -1.035533905932659149, -2.499999999999724221 ) ) ;
#1018 = CARTESIAN_POINT ( 'NONE',  ( -5.196152422706601826, 2.999999999999975131, -63.03867513459482552 ) ) ;
#1019 = CARTESIAN_POINT ( 'NONE',  ( -3.608439182435115633, 6.249999999999965361, -60.30801270189223118 ) ) ;
#1020 = EDGE_LOOP ( 'NONE', ( #18550, #4036, #18447, #25532 ) ) ;
#1021 = DIRECTION ( 'NONE',  ( -7.147005652999508048E-36, 5.642372883946980038E-36, 1.000000000000000000 ) ) ;
#1022 =( BOUNDED_CURVE ( )  B_SPLINE_CURVE ( 2, ( #24795, #13319, #10381, #3742, #29082, #17457, #26771, #1446, #29558 ),
 .UNSPECIFIED., .F., .F. ) 
 B_SPLINE_CURVE_WITH_KNOTS ( ( 3, 2, 2, 2, 3 ),
 ( 0.2249999999999999778, 0.2259259259259259189, 0.2277777777777777735, 0.2296296296296296280, 0.2305555555555555691 ),
 .UNSPECIFIED. ) 
 CURVE ( )  GEOMETRIC_REPRESENTATION_ITEM ( )  RATIONAL_B_SPLINE_CURVE ( ( 0.9330127018922196314, 0.9330127018922185211, 1.000000000000000000, 0.8660254037844388186, 1.000000000000000000, 0.8660254037844388186, 1.000000000000000000, 0.9330127018922184101, 0.9330127018922194093 ) ) 
 REPRESENTATION_ITEM ( '' )  );
#1023 = CARTESIAN_POINT ( 'NONE',  ( -5.196152422706573404, -3.000000000000002665, -56.78867513459484684 ) ) ;
#1024 = CARTESIAN_POINT ( 'NONE',  ( -5.999999999999963585, 1.780251999655701777E-13, -62.33632486540522422 ) ) ;
#1025 = CARTESIAN_POINT ( 'NONE',  ( 0.9172842643931518047, -15.89806073124487185, -7.323133569090728656 ) ) ;
#1026 = CARTESIAN_POINT ( 'NONE',  ( 4.763139720814407951, -2.749999999999988454, -174.5000000000000000 ) ) ;
#1027 = CARTESIAN_POINT ( 'NONE',  ( 118.4374999999998863, -2.499999999999964473, 1.035533905932929599 ) ) ;
#1028 = DIRECTION ( 'NONE',  ( -1.000000000000000000, -1.665334536937731113E-16, 1.526556658859586792E-16 ) ) ;
#1029 = CARTESIAN_POINT ( 'NONE',  ( -3.608439182435115633, 6.249999999999965361, -165.3080127018922667 ) ) ;
#1030 = CARTESIAN_POINT ( 'NONE',  ( 6.000000000000000888, -3.330669073875464691E-16, -7.560779664488942560E-35 ) ) ;
#1031 = CARTESIAN_POINT ( 'NONE',  ( 116.0000000000000142, 6.735557395310442023E-16, 5.500000000000000000 ) ) ;
#1032 = CARTESIAN_POINT ( 'NONE',  ( 6.350852961086080661, -9.614813431917819062E-14, -112.8750000000000568 ) ) ;
#1033 = CARTESIAN_POINT ( 'NONE',  ( 135.5571281299438056, -8.633349045433602598, 8.190208147179278697 ) ) ;
#1034 = CARTESIAN_POINT ( 'NONE',  ( 3.175426480543072749, -5.500000000000105693, -102.6250000000000000 ) ) ;
#1035 =( BOUNDED_CURVE ( )  B_SPLINE_CURVE ( 2, ( #20444, #22610, #6457, #17710, #18023, #8300, #10800, #6304, #22145 ),
 .UNSPECIFIED., .F., .T. ) 
 B_SPLINE_CURVE_WITH_KNOTS ( ( 3, 2, 2, 2, 3 ),
 ( 0.04687500000000000000, 0.05468750000000000000, 0.06250000000000000000, 0.07031250000000000000, 0.07812500000000000000 ),
 .UNSPECIFIED. ) 
 CURVE ( )  GEOMETRIC_REPRESENTATION_ITEM ( )  RATIONAL_B_SPLINE_CURVE ( ( 1.000000000000000000, 0.9238795325112867385, 1.000000000000000000, 0.9238795325112867385, 1.000000000000000000, 0.9238795325112867385, 1.000000000000000000, 0.9238795325112867385, 1.000000000000000000 ) ) 
 REPRESENTATION_ITEM ( '' )  );
#1036 = SURFACE_STYLE_FILL_AREA ( #5338 ) ;
#1037 = CARTESIAN_POINT ( 'NONE',  ( -5.999999999999963585, 1.780251999655701777E-13, -112.4136751345948255 ) ) ;
#1038 = CARTESIAN_POINT ( 'NONE',  ( 11.16367513459498539, 1.767766952966431937, -1.767766952966431937 ) ) ;
#1039 = CARTESIAN_POINT ( 'NONE',  ( -5.999999999999963585, 8.134310703387671600E-14, -144.8363248654052029 ) ) ;
#1040 = AXIS2_PLACEMENT_3D ( 'NONE', #7864, #2954, #12983 ) ;
#1041 = ORIENTED_EDGE ( 'NONE', *, *, #16511, .T. ) ;
#1042 = CARTESIAN_POINT ( 'NONE',  ( 13.50000000000006750, 1.873492889145123019, -1.873492889145011997 ) ) ;
#1043 = DIRECTION ( 'NONE',  ( -7.147005652999508048E-36, 5.642372883946980038E-36, 1.000000000000000000 ) ) ;
#1044 = CARTESIAN_POINT ( 'NONE',  ( 135.3284178065447634, -8.627956986131243511, -8.066146656158570849 ) ) ;
#1045 = ORIENTED_EDGE ( 'NONE', *, *, #27533, .F. ) ;
#1046 = CARTESIAN_POINT ( 'NONE',  ( -3.175426480542816510, 5.499999999999865885, -160.3750000000000000 ) ) ;
#1047 = CARTESIAN_POINT ( 'NONE',  ( -3.464101615137725076, 5.999999999999979572, -65.58632486540523132 ) ) ;
#1048 = CARTESIAN_POINT ( 'NONE',  ( 109.9997167782376835, -1.308140751793612777, 1.308140751793640533 ) ) ;
#1049 = AXIS2_PLACEMENT_3D ( 'NONE', #25942, #13872, #14024 ) ;
#1050 = CARTESIAN_POINT ( 'NONE',  ( 2.775557561562891351E-14, 6.250000000000033751, -85.06698729810780435 ) ) ;
#1051 = EDGE_CURVE ( 'NONE', #4225, #9180, #11354, .T. ) ;
#1052 = CARTESIAN_POINT ( 'NONE',  ( 6.000000000000052403, -1.607695154586662678, -102.7306624327026014 ) ) ;
#1053 = VERTEX_POINT ( 'NONE', #1286 ) ;
#1054 = AXIS2_PLACEMENT_3D ( 'NONE', #3334, #26390, #14748 ) ;
#1055 = ORIENTED_EDGE ( 'NONE', *, *, #17559, .T. ) ;
#1056 = EDGE_LOOP ( 'NONE', ( #1553, #10806, #23532, #17880 ) ) ;
#1057 = CARTESIAN_POINT ( 'NONE',  ( 133.0461002691896510, -2.071067811865468400, 4.999999999999989342 ) ) ;
#1058 = AXIS2_PLACEMENT_3D ( 'NONE', #778, #19533, #17385 ) ;
#1059 = EDGE_CURVE ( 'NONE', #22372, #26763, #10533, .T. ) ;
#1060 = CARTESIAN_POINT ( 'NONE',  ( 5.412658773652712085, -3.125000000000086153, -141.9330127018922383 ) ) ;
#1061 = ORIENTED_EDGE ( 'NONE', *, *, #15386, .T. ) ;
#1062 = CARTESIAN_POINT ( 'NONE',  ( 157.5863248654052597, 0.000000000000000000, 5.500000000000005329 ) ) ;
#1063 = CARTESIAN_POINT ( 'NONE',  ( 2.775557561562891351E-14, -6.250000000000061284, -130.8169872981078186 ) ) ;
#1064 = CARTESIAN_POINT ( 'NONE',  ( 6.000000000000000888, -1.607695154586752384, -135.1533121635129646 ) ) ;
#1065 = CARTESIAN_POINT ( 'NONE',  ( 6.000000000000000888, 1.743066579297358182E-13, -50.16367513459482552 ) ) ;
#1066 = CARTESIAN_POINT ( 'NONE',  ( 140.5384615384615756, -11.07692307692306777, -4.615384615384604317 ) ) ;
#1067 = VERTEX_POINT ( 'NONE', #13320 ) ;
#1068 = CARTESIAN_POINT ( 'NONE',  ( -0.02759001725020546192, -15.32981123538816703, -6.905035842853324723 ) ) ;
#1069 = CARTESIAN_POINT ( 'NONE',  ( 149.1636751345948255, 0.000000000000000000, 5.500000000000005329 ) ) ;
#1070 = SURFACE_STYLE_FILL_AREA ( #19813 ) ;
#1071 = DIRECTION ( 'NONE',  ( -1.000000000000000000, -1.665334536937736783E-16, -2.220446049250315546E-16 ) ) ;
#1072 = CARTESIAN_POINT ( 'NONE',  ( 3.464101615137852974, 5.999999999999884537, -46.33632486540520290 ) ) ;
#1073 = CARTESIAN_POINT ( 'NONE',  ( -5.412658773652739619, 3.124999999999975131, -65.31698729810780435 ) ) ;
#1074 = VECTOR ( 'NONE', #6895, 1000.000000000000000 ) ;
#1075 = CARTESIAN_POINT ( 'NONE',  ( 3.608439182435180470, 6.249999999999982236, -55.19198729810779724 ) ) ;
#1076 = CARTESIAN_POINT ( 'NONE',  ( 135.0000000000000000, 2.502093630246796874, 4.956520372253784501 ) ) ;
#1077 = CARTESIAN_POINT ( 'NONE',  ( 119.9999999999996163, 1.621546429789529453, -1.617766924407829654 ) ) ;
#1078 = DIRECTION ( 'NONE',  ( -7.147005652999508048E-36, 5.642372883946980038E-36, 1.000000000000000000 ) ) ;
#1079 = CARTESIAN_POINT ( 'NONE',  ( -3.175426480542816510, -5.500000000000057732, -131.3750000000000000 ) ) ;
#1080 = DIRECTION ( 'NONE',  ( 0.000000000000000000, 1.776356839400250465E-15, -1.000000000000000000 ) ) ;
#1081 = ORIENTED_EDGE ( 'NONE', *, *, #14582, .F. ) ;
#1082 = CARTESIAN_POINT ( 'NONE',  ( 141.8363248654052029, 0.000000000000000000, -5.500000000000005329 ) ) ;
#1083 = CARTESIAN_POINT ( 'NONE',  ( 0.000000000000000000, 0.000000000000000000, 0.000000000000000000 ) ) ;
#1084 = CARTESIAN_POINT ( 'NONE',  ( 16.83632486540531659, 1.767766952966487448, 1.767766952966320915 ) ) ;
#1085 = CARTESIAN_POINT ( 'NONE',  ( 6.000000000000000888, 7.762456499804235646E-14, -128.1636751345948539 ) ) ;
#1086 = VERTEX_POINT ( 'NONE', #10382 ) ;
#1087 = CARTESIAN_POINT ( 'NONE',  ( 112.2497167782374561, -1.308140751793585022, -1.308140751793640533 ) ) ;
#1088 = LINE ( 'NONE', #8141, #5633 ) ;
#1089 = CARTESIAN_POINT ( 'NONE',  ( 10.43750000000004619, -1.999999999999851674, 0.8284271247461753029 ) ) ;
#1090 = EDGE_CURVE ( 'NONE', #15347, #24916, #19018, .T. ) ;
#1091 = LINE ( 'NONE', #16959, #11184 ) ;
#1092 = EDGE_CURVE ( 'NONE', #11180, #15059, #22063, .T. ) ;
#1093 = CARTESIAN_POINT ( 'NONE',  ( 20.96132486540536277, 5.551115123125782702E-14, 2.500000000000002220 ) ) ;
#1094 = CARTESIAN_POINT ( 'NONE',  ( 115.3749999999999574, -1.767766952966320915, 1.767766952966431937 ) ) ;
#1095 = FACE_OUTER_BOUND ( 'NONE', #24456, .T. ) ;
#1096 = CARTESIAN_POINT ( 'NONE',  ( 10.06250000000005151, 2.000000000000212275, 0.8284271247461152399 ) ) ;
#1097 = CARTESIAN_POINT ( 'NONE',  ( 136.4925748654052882, 2.278174593052074925, 5.499999999999950262 ) ) ;
#1098 = CARTESIAN_POINT ( 'NONE',  ( -4.763139720814407951, -2.750000000000016431, -50.49999999999998579 ) ) ;
#1099 = FACE_OUTER_BOUND ( 'NONE', #25635, .T. ) ;
#1100 = FACE_OUTER_BOUND ( 'NONE', #19908, .T. ) ;
#1101 = CARTESIAN_POINT ( 'NONE',  ( 148.3913997308104058, -2.071067811865468400, 4.999999999999989342 ) ) ;
#1102 = CARTESIAN_POINT ( 'NONE',  ( 0.000000000000000000, 5.999999999999977796, -169.2113248654052313 ) ) ;
#1103 = CARTESIAN_POINT ( 'NONE',  ( 135.2243793856090690, -8.380352225012890344, 8.129889850246460270 ) ) ;
#1104 =( GEOMETRIC_REPRESENTATION_CONTEXT ( 3 ) GLOBAL_UNCERTAINTY_ASSIGNED_CONTEXT ( ( #498 ) ) GLOBAL_UNIT_ASSIGNED_CONTEXT ( ( #21304, #26930, #28783 ) ) REPRESENTATION_CONTEXT ( 'NONE', 'WORKASPACE' ) );
#1105 = CARTESIAN_POINT ( 'NONE',  ( -4.763139720814407951, -2.750000000000016431, -128.5000000000000000 ) ) ;
#1106 = DIRECTION ( 'NONE',  ( 0.000000000000000000, 5.551115123125767911E-17, -1.000000000000000000 ) ) ;
#1107 =( LENGTH_UNIT ( ) NAMED_UNIT ( * ) SI_UNIT ( .MILLI., .METRE. ) );
#1108 = CARTESIAN_POINT ( 'NONE',  ( 4.763139720814407951, 2.750000000000002665, -60.25000000000002842 ) ) ;
#1109 = CARTESIAN_POINT ( 'NONE',  ( -6.350852961085760029, -1.281975124255709124E-13, -53.62500000000002842 ) ) ;
#1110 = ORIENTED_EDGE ( 'NONE', *, *, #6647, .T. ) ;
#1111 = CARTESIAN_POINT ( 'NONE',  ( 151.0312500000000568, -2.485281374238556218, -6.000000000000005329 ) ) ;
#1112 = CARTESIAN_POINT ( 'NONE',  ( 159.0000000000000284, -11.07692307692306777, 4.615384615384604317 ) ) ;
#1113 = CARTESIAN_POINT ( 'NONE',  ( 15.12500000000000000, 1.414213562373201061, 1.414213562373034527 ) ) ;
#1114 = CARTESIAN_POINT ( 'NONE',  ( 6.000000000000052403, -1.607695154586662678, -98.23066243270257303 ) ) ;
#1115 = CARTESIAN_POINT ( 'NONE',  ( 111.1872167782375698, -1.849990392679472073, -0.7662911109075283278 ) ) ;
#1116 =( BOUNDED_CURVE ( )  B_SPLINE_CURVE ( 2, ( #10622, #3670, #22746, #13106, #10787, #29483, #3826, #13256, #22596 ),
 .UNSPECIFIED., .F., .T. ) 
 B_SPLINE_CURVE_WITH_KNOTS ( ( 3, 2, 2, 2, 3 ),
 ( 0.05882352941176470507, 0.06617647058823529493, 0.07352941176470588480, 0.08088235294117647467, 0.08823529411764706454 ),
 .UNSPECIFIED. ) 
 CURVE ( )  GEOMETRIC_REPRESENTATION_ITEM ( )  RATIONAL_B_SPLINE_CURVE ( ( 1.000000000000000000, 0.9238795325112867385, 1.000000000000000000, 0.9238795325112867385, 1.000000000000000000, 0.9238795325112867385, 1.000000000000000000, 0.9238795325112867385, 1.000000000000000000 ) ) 
 REPRESENTATION_ITEM ( '' )  );
#1117 = EDGE_CURVE ( 'NONE', #22297, #28019, #20626, .T. ) ;
#1118 = VECTOR ( 'NONE', #779, 1000.000000000000000 ) ;
#1119 = VERTEX_POINT ( 'NONE', #8675 ) ;
#1120 = CARTESIAN_POINT ( 'NONE',  ( 144.6562500000000568, -6.000000000000005329, 2.485281374238555774 ) ) ;
#1121 = CARTESIAN_POINT ( 'NONE',  ( 161.4367659555122430, -4.821111411827510906, -3.478723816445097317 ) ) ;
#1122 = EDGE_LOOP ( 'NONE', ( #29042, #12206, #2437, #3414 ) ) ;
#1123 = CARTESIAN_POINT ( 'NONE',  ( 6.350852961086080661, -9.614813431917819062E-14, -147.3750000000000284 ) ) ;
#1124 = CARTESIAN_POINT ( 'NONE',  ( -5.412658773652684552, -3.125000000000099920, -50.06698729810782567 ) ) ;
#1125 = CARTESIAN_POINT ( 'NONE',  ( 15.31250000000006928, -0.8284271247461753029, 1.999999999999911626 ) ) ;
#1126 = EDGE_LOOP ( 'NONE', ( #23177, #6889, #6796, #29307 ) ) ;
#1127 = CARTESIAN_POINT ( 'NONE',  ( -5.412658773652739619, 3.124999999999975131, -150.8169872981078186 ) ) ;
#1128 = CARTESIAN_POINT ( 'NONE',  ( -4.763139720814407951, -2.750000000000016431, -71.50000000000001421 ) ) ;
#1129 = CARTESIAN_POINT ( 'NONE',  ( 3.608439182435180470, -6.249999999999997335, -97.05801270189228092 ) ) ;
#1130 = DIRECTION ( 'NONE',  ( -1.387778780781444256E-14, 1.000000000000000000, 0.000000000000000000 ) ) ;
#1131 = CARTESIAN_POINT ( 'NONE',  ( -3.464101615137757051, -5.999999999999979572, -96.58632486540517448 ) ) ;
#1132 = LINE ( 'NONE', #5889, #21951 ) ;
#1133 = CARTESIAN_POINT ( 'NONE',  ( -5.999999999999963585, 1.780251999655701777E-13, -98.33632486540520290 ) ) ;
#1134 = LINE ( 'NONE', #26929, #11299 ) ;
#1135 = CARTESIAN_POINT ( 'NONE',  ( 3.175426480543072749, 5.499999999999865885, -157.6250000000000284 ) ) ;
#1136 = CARTESIAN_POINT ( 'NONE',  ( 0.000000000000000000, 0.000000000000000000, -185.0000000000000000 ) ) ;
#1137 = CARTESIAN_POINT ( 'NONE',  ( 6.350852961086080661, -9.614813431917819062E-14, -150.3749999999999716 ) ) ;
#1138 = DIRECTION ( 'NONE',  ( -7.147005652999508048E-36, 5.642372883946980038E-36, 1.000000000000000000 ) ) ;
#1139 = CARTESIAN_POINT ( 'NONE',  ( 137.2574251345947971, -2.278174593051671692, 5.500000000000352607 ) ) ;
#1140 = CLOSED_SHELL ( 'NONE', ( #15568, #6778, #2625, #29898, #6539, #6984, #26291, #17172, #11505, #2991 ) ) ;
#1141 = EDGE_CURVE ( 'NONE', #17687, #30043, #25055, .T. ) ;
#1142 = CARTESIAN_POINT ( 'NONE',  ( 3.175426480543072749, -5.500000000000105693, -92.12500000000002842 ) ) ;
#1143 = CARTESIAN_POINT ( 'NONE',  ( 140.0000000000000284, -54.99999999999990763, -7.500000000000007105 ) ) ;
#1144 = CARTESIAN_POINT ( 'NONE',  ( -4.763139720814407951, 2.749999999999946709, -77.74999999999998579 ) ) ;
#1145 = CARTESIAN_POINT ( 'NONE',  ( -3.464101615137725076, 5.999999999999979572, -164.5863248654051745 ) ) ;
#1146 = CARTESIAN_POINT ( 'NONE',  ( 6.000000000000000888, 1.743066579297358182E-13, -108.0863248654051745 ) ) ;
#1147 = CYLINDRICAL_SURFACE ( 'NONE', #12388, 6.000000000000000888 ) ;
#1148 = CARTESIAN_POINT ( 'NONE',  ( 10.89882486540524198, 1.035533905932749299, 2.499999999999904521 ) ) ;
#1149 = CARTESIAN_POINT ( 'NONE',  ( 5.196152422706629359, 3.000000000000002665, -134.9613248654052313 ) ) ;
#1150 = CARTESIAN_POINT ( 'NONE',  ( 5.999999999999993783, 1.607695154586726627, -174.5966878364870638 ) ) ;
#1151 = EDGE_CURVE ( 'NONE', #14341, #27647, #10219, .T. ) ;
#1152 = ORIENTED_EDGE ( 'NONE', *, *, #25660, .T. ) ;
#1153 = CARTESIAN_POINT ( 'NONE',  ( 120.0002832217621886, -1.308140751793557266, -1.308140751793529510 ) ) ;
#1154 = VERTEX_POINT ( 'NONE', #12860 ) ;
#1155 = ADVANCED_BREP_SHAPE_REPRESENTATION ( '', ( #4002, #18805 ), #12932 ) ;
#1156 =( BOUNDED_CURVE ( )  B_SPLINE_CURVE ( 2, ( #15701, #3965, #25011, #22735, #10302, #12938, #19665, #29006, #22274 ),
 .UNSPECIFIED., .F., .F. ) 
 B_SPLINE_CURVE_WITH_KNOTS ( ( 3, 2, 2, 2, 3 ),
 ( 0.2656250000000000000, 0.2734375000000000000, 0.2812500000000000000, 0.2890625000000000000, 0.2968750000000000000 ),
 .UNSPECIFIED. ) 
 CURVE ( )  GEOMETRIC_REPRESENTATION_ITEM ( )  RATIONAL_B_SPLINE_CURVE ( ( 1.000000000000000000, 0.9238795325112867385, 1.000000000000000000, 0.9238795325112867385, 1.000000000000000000, 0.9238795325112867385, 1.000000000000000000, 0.9238795325112867385, 1.000000000000000000 ) ) 
 REPRESENTATION_ITEM ( '' )  );
#1157 = CARTESIAN_POINT ( 'NONE',  ( -3.175426480542816510, -5.500000000000057732, -102.8750000000000142 ) ) ;
#1158 = DIRECTION ( 'NONE',  ( -7.147005652999508048E-36, 5.642372883946980038E-36, 1.000000000000000000 ) ) ;
#1159 = CARTESIAN_POINT ( 'NONE',  ( -7.216878364870328078, 0.000000000000000000, -117.0580127018922383 ) ) ;
#1160 = ORIENTED_EDGE ( 'NONE', *, *, #676, .T. ) ;
#1161 = DIRECTION ( 'NONE',  ( 1.000000000000000000, -5.551115123125773458E-17, -1.260129944081490338E-35 ) ) ;
#1162 = CARTESIAN_POINT ( 'NONE',  ( 105.6249999999999005, -1.767766952966376426, -1.767766952966320915 ) ) ;
#1163 = DIRECTION ( 'NONE',  ( 0.000000000000000000, 1.000000000000000000, -0.000000000000000000 ) ) ;
#1164 = CARTESIAN_POINT ( 'NONE',  ( -5.412658773652739619, 3.124999999999975131, -52.68301270189223828 ) ) ;
#1165 = ORIENTED_EDGE ( 'NONE', *, *, #26865, .F. ) ;
#1166 = CARTESIAN_POINT ( 'NONE',  ( -5.999999999999919176, 1.607695154586804565, -167.4033121635129930 ) ) ;
#1167 = CARTESIAN_POINT ( 'NONE',  ( 6.000000000000000000, 2.951592740943527306E-14, -162.0863248654052029 ) ) ;
#1168 = CARTESIAN_POINT ( 'NONE',  ( 118.8988248654049187, 0.8284271247463855792, 2.000000000000151879 ) ) ;
#1169 = CARTESIAN_POINT ( 'NONE',  ( 4.763139720814407951, -2.749999999999988454, -167.0000000000000284 ) ) ;
#1170 = CARTESIAN_POINT ( 'NONE',  ( 120.3124999999998579, -1.035533905932689347, 2.500000000000205169 ) ) ;
#1171 = CARTESIAN_POINT ( 'NONE',  ( 10.27382486540518869, -2.499999999999844569, -1.035533905932809473 ) ) ;
#1172 = CARTESIAN_POINT ( 'NONE',  ( 3.608439182435180470, 6.249999999999982236, -167.0580127018922383 ) ) ;
#1173 = CARTESIAN_POINT ( 'NONE',  ( 5.196152422706629359, 3.000000000000002665, -48.53867513459481131 ) ) ;
#1174 = EDGE_CURVE ( 'NONE', #6115, #21171, #17488, .T. ) ;
#1175 = CARTESIAN_POINT ( 'NONE',  ( -3.175426480542816066, 5.499999999999865885, -116.8750000000000000 ) ) ;
#1176 = DIRECTION ( 'NONE',  ( 1.000000000000000000, 9.251858538542971828E-16, 0.000000000000000000 ) ) ;
#1177 = CARTESIAN_POINT ( 'NONE',  ( -6.350852961085760029, -1.281975124255709124E-13, -104.6250000000000142 ) ) ;
#1178 = CARTESIAN_POINT ( 'NONE',  ( -0.5000000000000004441, -10.00000000000000888, -8.000000000000007105 ) ) ;
#1179 = CARTESIAN_POINT ( 'NONE',  ( 6.000000000000052403, -1.607695154586662678, -87.15331216351297883 ) ) ;
#1180 = FACE_OUTER_BOUND ( 'NONE', #15762, .T. ) ;
#1181 = ORIENTED_EDGE ( 'NONE', *, *, #24077, .T. ) ;
#1182 = CARTESIAN_POINT ( 'NONE',  ( 14.68750000000004796, 2.649519052838478661, 1.097466725451439196 ) ) ;
#1183 = CARTESIAN_POINT ( 'NONE',  ( -6.000000000000000888, 1.067854986875958443E-15, 7.560779664488942560E-35 ) ) ;
#1184 = CARTESIAN_POINT ( 'NONE',  ( 125.0000000000000568, -55.00000000000000711, 5.000000000000004441 ) ) ;
#1185 = ADVANCED_FACE ( 'NONE', ( #11627 ), #23114, .T. ) ;
#1186 = ADVANCED_FACE ( 'NONE', ( #6969 ), #23283, .T. ) ;
#1187 = EDGE_LOOP ( 'NONE', ( #5977, #17515, #27970, #21972 ) ) ;
#1188 = CARTESIAN_POINT ( 'NONE',  ( 4.763139720814407951, 2.750000000000002665, -160.7500000000000568 ) ) ;
#1189 = CARTESIAN_POINT ( 'NONE',  ( -5.999999999999962697, 3.323446944526963891E-14, -155.9136751345948255 ) ) ;
#1190 = CARTESIAN_POINT ( 'NONE',  ( 2.775557561562891351E-14, 6.250000000000033751, -80.56698729810784698 ) ) ;
#1191 = CARTESIAN_POINT ( 'NONE',  ( 5.196152422706629359, -2.999999999999988898, -129.2113248654052029 ) ) ;
#1192 = VERTEX_POINT ( 'NONE', #25708 ) ;
#1193 = CARTESIAN_POINT ( 'NONE',  ( 107.2113248654050608, -1.999999999999946265, 0.000000000000000000 ) ) ;
#1194 = VERTEX_POINT ( 'NONE', #13469 ) ;
#1195 = AXIS2_PLACEMENT_3D ( 'NONE', #3435, #9936, #26778 ) ;
#1196 = CARTESIAN_POINT ( 'NONE',  ( 154.9687500000000284, -2.485281374238585972, 6.000000000000005329 ) ) ;
#1197 =( BOUNDED_SURFACE ( )  B_SPLINE_SURFACE ( 3, 2, ( 
 ( #16094, #26975, #5780 ),
 ( #13065, #19641, #10581 ),
 ( #28979, #6104, #24687 ),
 ( #15515, #18378, #17815 ),
 ( #10430, #3327, #25401 ),
 ( #22556, #11320, #4362 ),
 ( #6675, #22095, #22397 ),
 ( #3475, #8989, #24838 ),
 ( #29281, #15194, #1336 ),
 ( #19935, #3787, #5940 ) ),
 .UNSPECIFIED., .F., .F., .T. ) 
 B_SPLINE_SURFACE_WITH_KNOTS ( ( 4, 2, 2, 2, 4 ),
 ( 3, 3 ),
 ( 6.283185307179586232, 6.675884388878310816, 7.068583470577034511, 7.461282552275758206, 7.853981633974482790 ),
 ( 0.000000000000000000, 1.000000000000000000 ),
 .UNSPECIFIED. ) 
 GEOMETRIC_REPRESENTATION_ITEM ( )  RATIONAL_B_SPLINE_SURFACE ( (
 ( 1.000000000000000000, 0.7071067811865475727, 1.000000000000000000),
 ( 1.000000000000000000, 0.7066757001360375323, 1.000000000000000000),
 ( 1.000000000000000000, 0.7265518147277378880, 1.000000000000000000),
 ( 1.000000000000000000, 0.7876784249694658291, 1.000000000000000000),
 ( 1.000000000000000000, 0.8282379786091598195, 1.000000000000000000),
 ( 1.000000000000000000, 0.9038128289597173737, 1.000000000000000000),
 ( 1.000000000000000000, 0.9386556746367764603, 1.000000000000000000),
 ( 1.000000000000000000, 0.9867291651255370999, 1.000000000000000000),
 ( 1.000000000000000000, 1.000158598892032291, 1.000000000000000000),
 ( 1.000000000000000000, 1.000000000000000000, 1.000000000000000000) ) ) 
 REPRESENTATION_ITEM ( '' )  SURFACE ( )  );
#1198 = ORIENTED_EDGE ( 'NONE', *, *, #12923, .F. ) ;
#1199 = CARTESIAN_POINT ( 'NONE',  ( -7.216878364870328078, 0.000000000000000000, -126.6919872981078186 ) ) ;
#1200 = CARTESIAN_POINT ( 'NONE',  ( 6.350852961086080661, -9.614813431917819062E-14, -169.8750000000000568 ) ) ;
#1201 = ORIENTED_EDGE ( 'NONE', *, *, #28205, .T. ) ;
#1202 = CARTESIAN_POINT ( 'NONE',  ( 14.81250000000010658, 0.8284271247463557142, -2.000000000000031530 ) ) ;
#1203 = DIRECTION ( 'NONE',  ( 1.000000000000000000, 0.000000000000000000, 0.000000000000000000 ) ) ;
#1204 = DIRECTION ( 'NONE',  ( 1.000000000000000000, 0.000000000000000000, 0.000000000000000000 ) ) ;
#1205 =( BOUNDED_CURVE ( )  B_SPLINE_CURVE ( 2, ( #1262, #8493, #17587, #15285, #1422, #13444, #20183, #10673, #29680 ),
 .UNSPECIFIED., .F., .T. ) 
 B_SPLINE_CURVE_WITH_KNOTS ( ( 3, 2, 2, 2, 3 ),
 ( 0.9472222222222221877, 0.9481481481481481843, 0.9499999999999999556, 0.9518518518518518379, 0.9527777777777778345 ),
 .UNSPECIFIED. ) 
 CURVE ( )  GEOMETRIC_REPRESENTATION_ITEM ( )  RATIONAL_B_SPLINE_CURVE ( ( 0.9330127018922194093, 0.9330127018922154125, 1.000000000000000000, 0.8660254037844388186, 1.000000000000000000, 0.8660254037844388186, 1.000000000000000000, 0.9330127018922154125, 0.9330127018922194093 ) ) 
 REPRESENTATION_ITEM ( '' )  );
#1207 = AXIS2_PLACEMENT_3D ( 'NONE', #21224, #30270, #23233 ) ;
#1206 = CARTESIAN_POINT ( 'NONE',  ( 160.3344755113492681, -11.26008890742377311, -4.149533274956910489 ) ) ;
#1208 = CARTESIAN_POINT ( 'NONE',  ( 139.6800748654052313, -2.278174593051950136, 5.500000000000074607 ) ) ;
#1209 = CARTESIAN_POINT ( 'NONE',  ( 1.000000000000000888, -14.99923475244192339, -9.015151515151522688 ) ) ;
#1210 = CARTESIAN_POINT ( 'NONE',  ( 114.3752832217622597, 1.849990392679551343, 0.000000000000000000 ) ) ;
#1211 = CARTESIAN_POINT ( 'NONE',  ( -3.608439182435115633, 6.249999999999965361, -66.94198729810787540 ) ) ;
#1212 = CARTESIAN_POINT ( 'NONE',  ( 2.775557561562891351E-14, 6.250000000000033751, -56.56698729810783277 ) ) ;
#1213 = DIRECTION ( 'NONE',  ( 1.000000000000000000, -3.469446951953694061E-16, 0.000000000000000000 ) ) ;
#1214 = ADVANCED_FACE ( 'NONE', ( #11475 ), #20499, .T. ) ;
#1215 = CARTESIAN_POINT ( 'NONE',  ( 6.000000000000000000, 2.951592740943527306E-14, -153.0863248654052029 ) ) ;
#1216 = CARTESIAN_POINT ( 'NONE',  ( -3.175426480542816510, 5.499999999999865885, -125.8749999999999858 ) ) ;
#1217 = COLOUR_RGB ( '', 0.72549020, 0.75294118, 0.79215686) ;
#1218 = CARTESIAN_POINT ( 'NONE',  ( -5.196152422706601826, 2.999999999999975131, -166.5386751345948539 ) ) ;
#1219 = CARTESIAN_POINT ( 'NONE',  ( 104.7401757384974843, -1.849990392679535134, -0.2444181134155588853 ) ) ;
#1220 = VERTEX_POINT ( 'NONE', #22811 ) ;
#1221 = CARTESIAN_POINT ( 'NONE',  ( 24.12500000000011724, -2.649519052838167354, 0.000000000000000000 ) ) ;
#1222 = AXIS2_PLACEMENT_3D ( 'NONE', #19173, #2861, #23774 ) ;
#1223 = CARTESIAN_POINT ( 'NONE',  ( -5.999999999999963585, 1.780251999655701777E-13, -68.33632486540521711 ) ) ;
#1224 = DIRECTION ( 'NONE',  ( -1.067522139062651904E-16, 1.000000000000000000, 0.000000000000000000 ) ) ;
#1225 = ADVANCED_FACE ( 'NONE', ( #2223 ), #14094, .T. ) ;
#1226 = CARTESIAN_POINT ( 'NONE',  ( 117.7886751345947545, -1.999999999999946265, 1.110223024625156540E-13 ) ) ;
#1227 = CARTESIAN_POINT ( 'NONE',  ( 3.464101615137757051, -5.999999999999979572, -147.9136751345947971 ) ) ;
#1228 = EDGE_LOOP ( 'NONE', ( #5885, #18243, #10727, #28847 ) ) ;
#1229 = CARTESIAN_POINT ( 'NONE',  ( 112.3747167782374703, -5.551115123125782702E-14, -1.849990392679523588 ) ) ;
#1230 = CYLINDRICAL_SURFACE ( 'NONE', #23312, 6.000000000000000888 ) ;
#1231 = CARTESIAN_POINT ( 'NONE',  ( 7.216878364870455975, -6.409875621278545621E-14, -94.44198729810780435 ) ) ;
#1232 = CARTESIAN_POINT ( 'NONE',  ( 19.53867513459495342, 5.551115123125782702E-14, 2.500000000000002220 ) ) ;
#1233 = CARTESIAN_POINT ( 'NONE',  ( 135.0000000000000284, 0.000000000000000000, 0.000000000000000000 ) ) ;
#1234 = CARTESIAN_POINT ( 'NONE',  ( 115.4374999999997868, -2.499999999999934719, 1.035533905932929599 ) ) ;
#1235 = VERTEX_POINT ( 'NONE', #8834 ) ;
#1236 = CYLINDRICAL_SURFACE ( 'NONE', #12553, 2.000000000000012879 ) ;
#1237 = CARTESIAN_POINT ( 'NONE',  ( 141.0937500000000000, 6.000000000000005329, 2.485281374238585972 ) ) ;
#1238 = EDGE_LOOP ( 'NONE', ( #7077, #14894, #19379, #17896, #8894, #44 ) ) ;
#1239 = CARTESIAN_POINT ( 'NONE',  ( 24.62500000000000711, 1.110223024625156540E-13, 2.649519052838056332 ) ) ;
#1240 = VECTOR ( 'NONE', #11493, 1000.000000000000000 ) ;
#1241 = CARTESIAN_POINT ( 'NONE',  ( -2.775557561562891351E-14, -5.500000000000115463, -50.25000000000001421 ) ) ;
#1242 = CARTESIAN_POINT ( 'NONE',  ( 2.081668171172167281E-16, 3.582034040661430693E-16, -2.499999999999999112 ) ) ;
#1243 = CARTESIAN_POINT ( 'NONE',  ( -5.999999999999963585, -1.487416814333745711E-14, -134.9136751345948255 ) ) ;
#1244 = CARTESIAN_POINT ( 'NONE',  ( 135.6636751345948255, 0.000000000000000000, 5.500000000000005329 ) ) ;
#1245 = CARTESIAN_POINT ( 'NONE',  ( -5.412658773652684552, -3.125000000000099920, -71.93301270189222407 ) ) ;
#1246 = DIRECTION ( 'NONE',  ( 1.000000000000000000, -5.551115123125773458E-17, -1.260129944081490338E-35 ) ) ;
#1247 = CARTESIAN_POINT ( 'NONE',  ( 149.3288997308104626, 4.999999999999989342, -2.071067811865468400 ) ) ;
#1248 = DIRECTION ( 'NONE',  ( -1.000000000000000000, 0.000000000000000000, 0.000000000000000000 ) ) ;
#1249 = PLANE ( 'NONE',  #28981 ) ;
#1250 =( BOUNDED_CURVE ( )  B_SPLINE_CURVE ( 2, ( #18450, #23048, #27922, #4439, #25639, #4288, #22892, #16464, #25793 ),
 .UNSPECIFIED., .F., .F. ) 
 B_SPLINE_CURVE_WITH_KNOTS ( ( 3, 2, 2, 2, 3 ),
 ( 0.6416666666666666075, 0.6425925925925926041, 0.6444444444444443754, 0.6462962962962963687, 0.6472222222222221433 ),
 .UNSPECIFIED. ) 
 CURVE ( )  GEOMETRIC_REPRESENTATION_ITEM ( )  RATIONAL_B_SPLINE_CURVE ( ( 0.9330127018922194093, 0.9330127018922154125, 1.000000000000000000, 0.8660254037844388186, 1.000000000000000000, 0.8660254037844388186, 1.000000000000000000, 0.9330127018922274029, 0.9330127018922194093 ) ) 
 REPRESENTATION_ITEM ( '' )  );
#1251 = CARTESIAN_POINT ( 'NONE',  ( 3.464101615137757051, -5.999999999999979572, -152.4136751345947971 ) ) ;
#1252 = ADVANCED_FACE ( 'NONE', ( #6513 ), #13620, .T. ) ;
#1253 = CARTESIAN_POINT ( 'NONE',  ( -5.999999999999963585, 1.780251999655701777E-13, -104.3363248654052313 ) ) ;
#1254 = EDGE_CURVE ( 'NONE', #18627, #2002, #13331, .T. ) ;
#1255 = CARTESIAN_POINT ( 'NONE',  ( -4.763139720814407951, 2.749999999999946709, -128.7500000000000284 ) ) ;
#1256 = CARTESIAN_POINT ( 'NONE',  ( -5.999999999999963585, 3.021315404115421074E-15, -177.8363248654052029 ) ) ;
#1257 = CARTESIAN_POINT ( 'NONE',  ( -6.000000000000000888, 1.067854986875958443E-15, 7.560779664488942560E-35 ) ) ;
#1258 = ORIENTED_EDGE ( 'NONE', *, *, #14946, .T. ) ;
#1259 = VECTOR ( 'NONE', #23001, 1000.000000000000000 ) ;
#1260 = CARTESIAN_POINT ( 'NONE',  ( -4.763139720814407951, -2.750000000000016431, -67.00000000000000000 ) ) ;
#1261 = CARTESIAN_POINT ( 'NONE',  ( -3.175426480542816510, 5.499999999999865885, -58.37500000000004974 ) ) ;
#1262 = CARTESIAN_POINT ( 'NONE',  ( 6.000000000000001776, 5.345404176511898156E-15, -174.0863248654052597 ) ) ;
#1263 = ORIENTED_EDGE ( 'NONE', *, *, #10873, .F. ) ;
#1264 = CARTESIAN_POINT ( 'NONE',  ( 109.9999999999999432, 2.500000000000030198, 0.000000000000000000 ) ) ;
#1265 = CARTESIAN_POINT ( 'NONE',  ( 145.9687500000000284, -2.485281374238585972, 6.000000000000005329 ) ) ;
#1266 = CARTESIAN_POINT ( 'NONE',  ( 0.000000000000000000, 0.000000000000000000, 0.000000000000000000 ) ) ;
#1267 = CARTESIAN_POINT ( 'NONE',  ( 15.93749999999996980, 2.000000000000091926, -0.8284271247462955401 ) ) ;
#1268 = MECHANICAL_DESIGN_GEOMETRIC_PRESENTATION_REPRESENTATION (  '', ( #8628 ), #18972 ) ;
#1269 =( NAMED_UNIT ( * ) SI_UNIT ( $, .STERADIAN. ) SOLID_ANGLE_UNIT ( ) );
#1270 = CARTESIAN_POINT ( 'NONE',  ( 110.7497167782376550, 1.308140751793640533, 1.308140751793640533 ) ) ;
#1271 = ORIENTED_EDGE ( 'NONE', *, *, #12673, .F. ) ;
#1272 = CARTESIAN_POINT ( 'NONE',  ( 143.5312500000000284, -2.485281374238555774, -6.000000000000005329 ) ) ;
#1273 = CARTESIAN_POINT ( 'NONE',  ( 5.999999999999949374, -1.607695154586841868, -121.6533121635130215 ) ) ;
#1274 = ORIENTED_EDGE ( 'NONE', *, *, #7037, .T. ) ;
#1275 = B_SPLINE_CURVE_WITH_KNOTS ( 'NONE', 3,
 ( #25498, #22914, #30115, #6462, #15730, #4464, #25040, #13891, #15888, #15580, #24893, #11260, #11103, #29807, #23230, #3842, #22615, #20610 ),
 .UNSPECIFIED., .F., .F.,
 ( 4, 2, 2, 2, 2, 2, 2, 2, 4 ),
 ( 0.001391798398341157015, 0.001904360710870518173, 0.002416923023399879331, 0.002929485335929240489, 0.003442047648458601648, 0.003954609960987962372, 0.004467172273517323530, 0.004979734586046684688, 0.005492296898576045847 ),
 .UNSPECIFIED. ) ;
#1276 = CARTESIAN_POINT ( 'NONE',  ( 0.000000000000000000, 5.499999999999991118, -145.5000000000000284 ) ) ;
#1277 = CARTESIAN_POINT ( 'NONE',  ( 2.775557561562891351E-14, -6.250000000000061284, -48.31698729810784698 ) ) ;
#1278 = CARTESIAN_POINT ( 'NONE',  ( 18.18750000000005684, 0.8284271247463557142, 1.999999999999971800 ) ) ;
#1279 = ORIENTED_EDGE ( 'NONE', *, *, #8303, .F. ) ;
#1280 = CARTESIAN_POINT ( 'NONE',  ( 2.775557561562891351E-14, 6.250000000000033751, -146.5669872981077901 ) ) ;
#1281 = CARTESIAN_POINT ( 'NONE',  ( -3.175426480542816510, -5.500000000000057732, -71.37499999999997158 ) ) ;
#1282 = CARTESIAN_POINT ( 'NONE',  ( -5.412658773652684552, -3.125000000000099920, -91.43301270189225249 ) ) ;
#1283 = CARTESIAN_POINT ( 'NONE',  ( -3.035671606378273601, -10.57820549248702413, -19.81012201018820207 ) ) ;
#1284 = DIRECTION ( 'NONE',  ( 0.000000000000000000, 0.000000000000000000, -1.000000000000000000 ) ) ;
#1285 = DIRECTION ( 'NONE',  ( -7.147005652999508048E-36, 5.642372883946980038E-36, 1.000000000000000000 ) ) ;
#1286 = CARTESIAN_POINT ( 'NONE',  ( -4.999999999999886313, -10.00000000000000888, -5.000000000000004441 ) ) ;
#1287 = CARTESIAN_POINT ( 'NONE',  ( 6.000000000000000888, 1.743066579297358182E-13, -64.58632486540520290 ) ) ;
#1288 = SURFACE_STYLE_FILL_AREA ( #19737 ) ;
#1289 = EDGE_CURVE ( 'NONE', #6343, #3203, #19120, .T. ) ;
#1290 = CARTESIAN_POINT ( 'NONE',  ( 4.763139720814407951, 2.750000000000002665, -154.7500000000000568 ) ) ;
#1291 = CARTESIAN_POINT ( 'NONE',  ( 117.8363248654051176, 1.414213562373145550, 1.414213562373034527 ) ) ;
#1292 = CARTESIAN_POINT ( 'NONE',  ( -2.775557561562891351E-14, -5.500000000000115463, -147.7500000000000568 ) ) ;
#1293 = CARTESIAN_POINT ( 'NONE',  ( -2.846577545692754452, 4.964493094582011601, -180.0000000000000568 ) ) ;
#1294 = CARTESIAN_POINT ( 'NONE',  ( 4.763139720814407951, -2.749999999999988454, -83.00000000000001421 ) ) ;
#1295 = CARTESIAN_POINT ( 'NONE',  ( 139.5000000000000284, -54.99999999999990763, 7.500000000000007105 ) ) ;
#1296 = DIRECTION ( 'NONE',  ( 1.000000000000000000, 0.000000000000000000, 0.000000000000000000 ) ) ;
#1297 = CARTESIAN_POINT ( 'NONE',  ( -2.775557561562891351E-14, -5.500000000000115463, -84.74999999999998579 ) ) ;
#1298 =( BOUNDED_CURVE ( )  B_SPLINE_CURVE ( 2, ( #8723, #27280, #10584, #3789, #10750, #8562, #6254, #15672, #29438 ),
 .UNSPECIFIED., .F., .T. ) 
 B_SPLINE_CURVE_WITH_KNOTS ( ( 3, 2, 2, 2, 3 ),
 ( 0.2031250000000000000, 0.2109375000000000000, 0.2187500000000000000, 0.2265625000000000000, 0.2343750000000000000 ),
 .UNSPECIFIED. ) 
 CURVE ( )  GEOMETRIC_REPRESENTATION_ITEM ( )  RATIONAL_B_SPLINE_CURVE ( ( 1.000000000000000000, 0.9238795325112867385, 1.000000000000000000, 0.9238795325112867385, 1.000000000000000000, 0.9238795325112867385, 1.000000000000000000, 0.9238795325112867385, 1.000000000000000000 ) ) 
 REPRESENTATION_ITEM ( '' )  );
#1299 = CARTESIAN_POINT ( 'NONE',  ( 0.000000000000000000, 0.000000000000000000, 0.000000000000000000 ) ) ;
#1300 = CARTESIAN_POINT ( 'NONE',  ( 151.8898502691896510, 3.535533905932725318, -3.535533905932725318 ) ) ;
#1301 = CARTESIAN_POINT ( 'NONE',  ( -0.04562205425674009662, -14.50000000000001243, -8.291335958003937634 ) ) ;
#1302 = CARTESIAN_POINT ( 'NONE',  ( 139.5000000000000284, -9.165151389911669000, -8.000000000000007105 ) ) ;
#1303 = AXIS2_PLACEMENT_3D ( 'NONE', #27495, #22921, #6627 ) ;
#1304 = CARTESIAN_POINT ( 'NONE',  ( -5.999999999999962697, 3.323446944526963891E-14, -149.9136751345948255 ) ) ;
#1305 = CARTESIAN_POINT ( 'NONE',  ( 111.9613248654051461, -2.775557561562891351E-14, 2.000000000000112799 ) ) ;
#1306 = CARTESIAN_POINT ( 'NONE',  ( 120.2497167782375271, -1.308140751793529510, -1.308140751793640533 ) ) ;
#1307 = CARTESIAN_POINT ( 'NONE',  ( 0.000000000000000000, 0.000000000000000000, 0.000000000000000000 ) ) ;
#1308 = ORIENTED_EDGE ( 'NONE', *, *, #3958, .T. ) ;
#1309 = PRESENTATION_STYLE_ASSIGNMENT (( #17177 ) ) ;
#1310 = CARTESIAN_POINT ( 'NONE',  ( 0.000000000000000000, 0.000000000000000000, 0.000000000000000000 ) ) ;
#1311 = CARTESIAN_POINT ( 'NONE',  ( 5.196152422706629359, 3.000000000000002665, -80.96132486540518869 ) ) ;
#1312 = CARTESIAN_POINT ( 'NONE',  ( 1101.535898384862321, 1.665334536937736830E-13, 2.220446049250315605E-13 ) ) ;
#1313 = ORIENTED_EDGE ( 'NONE', *, *, #1406, .F. ) ;
#1314 = UNCERTAINTY_MEASURE_WITH_UNIT (LENGTH_MEASURE( 1.000000000000000082E-05 ), #17406, 'distance_accuracy_value', 'NONE');
#1315 = EDGE_LOOP ( 'NONE', ( #26283, #787, #24719, #15620 ) ) ;
#1316 = ADVANCED_FACE ( 'NONE', ( #205 ), #7283, .T. ) ;
#1317 = CARTESIAN_POINT ( 'NONE',  ( 3.175426480543072749, -5.500000000000105693, -99.62500000000007105 ) ) ;
#1318 = AXIS2_PLACEMENT_3D ( 'NONE', #14407, #23448, #7138 ) ;
#1319 = CARTESIAN_POINT ( 'NONE',  ( 0.000000000000000000, 0.000000000000000000, 0.000000000000000000 ) ) ;
#1320 = CARTESIAN_POINT ( 'NONE',  ( 3.608439182435180470, -6.249999999999997335, -112.0580127018922241 ) ) ;
#1321 = ORIENTED_EDGE ( 'NONE', *, *, #25861, .F. ) ;
#1322 = CARTESIAN_POINT ( 'NONE',  ( -5.196152422706601826, 2.999999999999975131, -140.4613248654052029 ) ) ;
#1323 = CARTESIAN_POINT ( 'NONE',  ( 135.0000000000000568, -7.635447689476136723, 8.089997508179699537 ) ) ;
#1324 = CARTESIAN_POINT ( 'NONE',  ( -7.216878364870328078, 0.000000000000000000, -52.55801270189219565 ) ) ;
#1325 = ORIENTED_EDGE ( 'NONE', *, *, #19386, .F. ) ;
#1326 = LINE ( 'NONE', #10740, #18160 ) ;
#1327 = CARTESIAN_POINT ( 'NONE',  ( 22.66367513459499605, -1.767766952966265404, 1.767766952966376426 ) ) ;
#1328 = EDGE_CURVE ( 'NONE', #891, #6568, #7854, .T. ) ;
#1329 = DIRECTION ( 'NONE',  ( -7.147005652999508048E-36, 5.642372883946980038E-36, 1.000000000000000000 ) ) ;
#1330 = CARTESIAN_POINT ( 'NONE',  ( 118.7738248654049897, 2.000000000000122125, 0.8284271247462955401 ) ) ;
#1331 = AXIS2_PLACEMENT_3D ( 'NONE', #12013, #28380, #24086 ) ;
#1332 = CARTESIAN_POINT ( 'NONE',  ( -4.763139720814407951, -2.750000000000016431, -172.0000000000000284 ) ) ;
#1333 = CARTESIAN_POINT ( 'NONE',  ( 114.9374999999997868, 2.500000000000055067, -1.035533905932629173 ) ) ;
#1334 = CARTESIAN_POINT ( 'NONE',  ( -3.464101615137757051, -5.999999999999979572, -158.0863248654051461 ) ) ;
#1335 = CARTESIAN_POINT ( 'NONE',  ( -3.608439182435052128, -6.250000000000110134, -169.3080127018922383 ) ) ;
#1336 = CARTESIAN_POINT ( 'NONE',  ( -0.8690767379103921941, -9.065461631044712476, 4.000000000000005329 ) ) ;
#1337 = CARTESIAN_POINT ( 'NONE',  ( 3.175426480543072749, -5.500000000000105693, -108.6250000000000426 ) ) ;
#1338 = CARTESIAN_POINT ( 'NONE',  ( 23.89882486540529882, 1.035533905932809473, 2.499999999999844569 ) ) ;
#1339 = CARTESIAN_POINT ( 'NONE',  ( 6.350852961086080661, -9.614813431917819062E-14, -105.3750000000000142 ) ) ;
#1340 = CYLINDRICAL_SURFACE ( 'NONE', #18262, 5.500000000000000000 ) ;
#1341 = CARTESIAN_POINT ( 'NONE',  ( 135.2045928001402331, -8.331920847649417539, 8.143621320507632433 ) ) ;
#1342 = AXIS2_PLACEMENT_3D ( 'NONE', #6536, #15958, #2095 ) ;
#1343 = ORIENTED_EDGE ( 'NONE', *, *, #17804, .T. ) ;
#1344 = CARTESIAN_POINT ( 'NONE',  ( 14.50000000000012434, 1.873492889145067508, -1.873492889144956486 ) ) ;
#1345 = CARTESIAN_POINT ( 'NONE',  ( -5.196152422706573404, -3.000000000000002665, -90.71132486540523132 ) ) ;
#1346 = AXIS2_PLACEMENT_3D ( 'NONE', #795, #23995, #7698 ) ;
#1347 = CARTESIAN_POINT ( 'NONE',  ( 111.8752832217622881, -1.849990392679579099, 1.110223024625156540E-13 ) ) ;
#1348 = ORIENTED_EDGE ( 'NONE', *, *, #15602, .T. ) ;
#1349 = DIRECTION ( 'NONE',  ( 0.000000000000000000, -1.000000000000000000, 0.000000000000000000 ) ) ;
#1350 = CARTESIAN_POINT ( 'NONE',  ( -5.412658773652739619, 3.124999999999975131, -84.81698729810783277 ) ) ;
#1351 =( BOUNDED_CURVE ( )  B_SPLINE_CURVE ( 2, ( #11002, #18216, #11310, #17765, #20347, #30007, #29702 ),
 .UNSPECIFIED., .F., .F. ) 
 B_SPLINE_CURVE_WITH_KNOTS ( ( 3, 2, 2, 3 ),
 ( 0.01238478393654788429, 0.01470588235294112422, 0.02205882352941179736, 0.02941176470588236294 ),
 .UNSPECIFIED. ) 
 CURVE ( )  GEOMETRIC_REPRESENTATION_ITEM ( )  RATIONAL_B_SPLINE_CURVE ( ( 0.9671125746062365636, 0.9759710988701293388, 1.000000000000000000, 0.9238795325112867385, 1.000000000000000000, 0.9238795325112867385, 1.000000000000000000 ) ) 
 REPRESENTATION_ITEM ( '' )  );
#1352 = CARTESIAN_POINT ( 'NONE',  ( 150.0863248654052313, 0.000000000000000000, 5.500000000000005329 ) ) ;
#1353 = EDGE_LOOP ( 'NONE', ( #22306, #16440, #26957, #9386 ) ) ;
#1354 = LINE ( 'NONE', #15056, #20895 ) ;
#1355 = VECTOR ( 'NONE', #18169, 1000.000000000000000 ) ;
#1356 = EDGE_LOOP ( 'NONE', ( #20099, #18143, #1741, #23491 ) ) ;
#1357 = VERTEX_POINT ( 'NONE', #28452 ) ;
#1358 = CARTESIAN_POINT ( 'NONE',  ( 156.8437500000000284, -6.000000000000005329, -2.485281374238555774 ) ) ;
#1359 = EDGE_CURVE ( 'NONE', #1710, #6311, #12374, .T. ) ;
#1360 = CARTESIAN_POINT ( 'NONE',  ( -6.350852961085760029, -1.281975124255709124E-13, -119.6250000000000142 ) ) ;
#1361 = CARTESIAN_POINT ( 'NONE',  ( 5.412658773652739619, 3.124999999999988898, -138.6830127018922099 ) ) ;
#1362 = ORIENTED_EDGE ( 'NONE', *, *, #29688, .F. ) ;
#1363 = CARTESIAN_POINT ( 'NONE',  ( 135.5000000000000284, -9.047800747817580813, -7.500000000000007105 ) ) ;
#1364 = CARTESIAN_POINT ( 'NONE',  ( 3.608439182435180470, -6.249999999999997335, -120.1919872981077901 ) ) ;
#1365 = FACE_OUTER_BOUND ( 'NONE', #19338, .T. ) ;
#1366 = CARTESIAN_POINT ( 'NONE',  ( 3.175426480543072749, 5.499999999999865885, -175.6250000000000284 ) ) ;
#1367 = CARTESIAN_POINT ( 'NONE',  ( 159.4166817098593754, -11.36111566036954912, 3.917249193633611792 ) ) ;
#1368 = CARTESIAN_POINT ( 'NONE',  ( 107.5386751345947403, 5.551115123125782702E-14, 2.000000000000001776 ) ) ;
#1369 = ORIENTED_EDGE ( 'NONE', *, *, #28211, .F. ) ;
#1370 = CARTESIAN_POINT ( 'NONE',  ( 16.68750000000013856, -0.8284271247461753029, -2.000000000000151879 ) ) ;
#1371 = EDGE_CURVE ( 'NONE', #2905, #26686, #29456, .T. ) ;
#1372 = CARTESIAN_POINT ( 'NONE',  ( -3.464101615137725076, 5.999999999999979572, -148.0863248654052029 ) ) ;
#1373 = CARTESIAN_POINT ( 'NONE',  ( 159.6175193642574186, -12.16729450327831685, -3.789279010572755624 ) ) ;
#1374 = CARTESIAN_POINT ( 'NONE',  ( 6.000000000000000888, -1.607695154586752384, -54.73066243270260856 ) ) ;
#1375 = CARTESIAN_POINT ( 'NONE',  ( 115.0002832217621886, -1.308140751793585022, -1.308140751793640533 ) ) ;
#1376 = CARTESIAN_POINT ( 'NONE',  ( 5.412658773652739619, 3.124999999999988898, -68.81698729810781856 ) ) ;
#1377 = CARTESIAN_POINT ( 'NONE',  ( -5.412658773652684552, -3.125000000000099920, -57.56698729810783277 ) ) ;
#1378 = CARTESIAN_POINT ( 'NONE',  ( 6.000000000000000888, -1.859271017917181981E-14, -120.6636751345948255 ) ) ;
#1379 = CARTESIAN_POINT ( 'NONE',  ( -5.196152422706573404, -3.000000000000002665, -64.28867513459479710 ) ) ;
#1380 = CARTESIAN_POINT ( 'NONE',  ( 0.000000000000000000, 5.999999999999977796, -55.78867513459484684 ) ) ;
#1381 = CARTESIAN_POINT ( 'NONE',  ( 0.000000000000000000, -10.50000000000000888, -8.500000000000007105 ) ) ;
#1382 = CARTESIAN_POINT ( 'NONE',  ( -4.763139720814407951, -2.750000000000016431, -128.5000000000000000 ) ) ;
#1383 = ORIENTED_EDGE ( 'NONE', *, *, #1753, .T. ) ;
#1384 = DIRECTION ( 'NONE',  ( 0.000000000000000000, 0.000000000000000000, 1.000000000000000000 ) ) ;
#1385 = CARTESIAN_POINT ( 'NONE',  ( 17.72617513459489658, -2.499999999999964473, 1.035533905932749299 ) ) ;
#1386 = CARTESIAN_POINT ( 'NONE',  ( 135.0000000000000284, 1.408343819019456570E-15, 11.00000000000000355 ) ) ;
#1387 = CARTESIAN_POINT ( 'NONE',  ( 5.196152422706629359, 3.000000000000002665, -130.4613248654051745 ) ) ;
#1388 = CARTESIAN_POINT ( 'NONE',  ( 6.000000000000000888, -3.330669073875464691E-16, -7.560779664488942560E-35 ) ) ;
#1389 = VERTEX_POINT ( 'NONE', #9592 ) ;
#1390 = CARTESIAN_POINT ( 'NONE',  ( 112.4372167782373708, 0.7662911109079189043, -1.849990392679231599 ) ) ;
#1391 = CARTESIAN_POINT ( 'NONE',  ( -15.49999999999999289, -54.99999999999990763, -7.500000000000007105 ) ) ;
#1392 = CARTESIAN_POINT ( 'NONE',  ( 2.775557561562891351E-14, -6.250000000000061284, -112.8169872981078470 ) ) ;
#1393 = CARTESIAN_POINT ( 'NONE',  ( 19.72617513459489658, -2.499999999999964473, 1.035533905932809473 ) ) ;
#1394 =( BOUNDED_CURVE ( )  B_SPLINE_CURVE ( 2, ( #16594, #11373, #23336, #27901, #20870, #28206, #23487, #25288, #6875 ),
 .UNSPECIFIED., .F., .T. ) 
 B_SPLINE_CURVE_WITH_KNOTS ( ( 3, 2, 2, 2, 3 ),
 ( 0.2916666666666666297, 0.2925925925925926263, 0.2944444444444443976, 0.2962962962962962798, 0.2972222222222222765 ),
 .UNSPECIFIED. ) 
 CURVE ( )  GEOMETRIC_REPRESENTATION_ITEM ( )  RATIONAL_B_SPLINE_CURVE ( ( 0.9330127018922194093, 0.9330127018922154125, 1.000000000000000000, 0.8660254037844388186, 1.000000000000000000, 0.8660254037844388186, 1.000000000000000000, 0.9330127018922154125, 0.9330127018922194093 ) ) 
 REPRESENTATION_ITEM ( '' )  );
#1395 = VECTOR ( 'NONE', #26129, 1000.000000000000000 ) ;
#1396 = CARTESIAN_POINT ( 'NONE',  ( 113.1874999999998437, 1.035533905932779275, 2.500000000000205169 ) ) ;
#1397 = EDGE_LOOP ( 'NONE', ( #6849, #11106, #18173, #7701 ) ) ;
#1398 = CYLINDRICAL_SURFACE ( 'NONE', #13043, 6.000000000000000888 ) ;
#1399 = CARTESIAN_POINT ( 'NONE',  ( 145.0312500000000568, -2.485281374238555774, -6.000000000000005329 ) ) ;
#1400 = EDGE_CURVE ( 'NONE', #12501, #7661, #12527, .T. ) ;
#1401 =( BOUNDED_CURVE ( )  B_SPLINE_CURVE ( 2, ( #21034, #18890, #18282, #25295, #23026, #21774, #7339, #12139, #16745 ),
 .UNSPECIFIED., .F., .F. ) 
 B_SPLINE_CURVE_WITH_KNOTS ( ( 3, 2, 2, 2, 3 ),
 ( 0.5588235294117647189, 0.5661764705882352811, 0.5735294117647058432, 0.5808823529411765163, 0.5882352941176470784 ),
 .UNSPECIFIED. ) 
 CURVE ( )  GEOMETRIC_REPRESENTATION_ITEM ( )  RATIONAL_B_SPLINE_CURVE ( ( 1.000000000000000000, 0.9238795325112867385, 1.000000000000000000, 0.9238795325112867385, 1.000000000000000000, 0.9238795325112867385, 1.000000000000000000, 0.9238795325112867385, 1.000000000000000000 ) ) 
 REPRESENTATION_ITEM ( '' )  );
#1402 = CARTESIAN_POINT ( 'NONE',  ( -5.999999999999971578, 1.607695154586715303, -80.98066243270260145 ) ) ;
#1403 = CARTESIAN_POINT ( 'NONE',  ( -2.775557561562891351E-14, -5.500000000000115463, -48.75000000000001421 ) ) ;
#1404 = CARTESIAN_POINT ( 'NONE',  ( 6.000000000000000888, 1.743066579297358182E-13, -90.08632486540521711 ) ) ;
#1405 = LINE ( 'NONE', #5849, #3370 ) ;
#1406 = EDGE_CURVE ( 'NONE', #15772, #19941, #28840, .T. ) ;
#1407 = CARTESIAN_POINT ( 'NONE',  ( 136.0386751345948255, -5.500000000000005329, 0.000000000000000000 ) ) ;
#1408 = CARTESIAN_POINT ( 'NONE',  ( 5.412658773652712085, -3.125000000000086153, -75.93301270189223828 ) ) ;
#1409 = CARTESIAN_POINT ( 'NONE',  ( 135.8007686613928229, -8.946933464881634990, -7.999999999999145572 ) ) ;
#1410 = CARTESIAN_POINT ( 'NONE',  ( 152.7038997308104342, 2.071067811865468400, 4.999999999999989342 ) ) ;
#1411 = DIRECTION ( 'NONE',  ( -1.000000000000000000, -0.000000000000000000, 0.000000000000000000 ) ) ;
#1412 = CARTESIAN_POINT ( 'NONE',  ( 124.9999999999999432, -65.00000000000000000, 8.000000000000007105 ) ) ;
#1413 = CARTESIAN_POINT ( 'NONE',  ( -5.999999999999963585, 1.780251999655701777E-13, -83.33632486540520290 ) ) ;
#1414 = CYLINDRICAL_SURFACE ( 'NONE', #17751, 5.500000000000000000 ) ;
#1415 = CARTESIAN_POINT ( 'NONE',  ( 113.7886751345947687, -1.999999999999918510, 0.000000000000000000 ) ) ;
#1416 = CARTESIAN_POINT ( 'NONE',  ( 3.175426480543072749, 5.499999999999865885, -135.1250000000000284 ) ) ;
#1417 = CARTESIAN_POINT ( 'NONE',  ( 10.35117513459487704, 2.500000000000084821, 1.035533905932689347 ) ) ;
#1418 = CARTESIAN_POINT ( 'NONE',  ( -5.412658773652739619, 3.124999999999975131, -148.6830127018922099 ) ) ;
#1419 = FACE_OUTER_BOUND ( 'NONE', #6136, .T. ) ;
#1420 = ORIENTED_EDGE ( 'NONE', *, *, #26541, .T. ) ;
#1421 = CARTESIAN_POINT ( 'NONE',  ( 3.175426480543072749, 5.499999999999865885, -60.12500000000000000 ) ) ;
#1422 = CARTESIAN_POINT ( 'NONE',  ( 0.000000000000000000, -5.999999999999991118, -174.4613248654052313 ) ) ;
#1423 = ORIENTED_EDGE ( 'NONE', *, *, #29948, .F. ) ;
#1424 = CARTESIAN_POINT ( 'NONE',  ( 110.9374999999997442, 2.500000000000055067, -1.035533905932388699 ) ) ;
#1425 = CARTESIAN_POINT ( 'NONE',  ( 147.1875000000000284, 4.242640687119269671, 4.242640687119298093 ) ) ;
#1426 = CARTESIAN_POINT ( 'NONE',  ( -5.999999999999956479, -1.607695154586745057, -118.3466878364870496 ) ) ;
#1427 = CARTESIAN_POINT ( 'NONE',  ( 14.68750000000004796, -0.8284271247460552878, -1.999999999999971800 ) ) ;
#1428 = ORIENTED_EDGE ( 'NONE', *, *, #835, .F. ) ;
#1429 = CARTESIAN_POINT ( 'NONE',  ( 136.7812500000000284, 2.485281374238585972, 6.000000000000005329 ) ) ;
#1430 = CARTESIAN_POINT ( 'NONE',  ( 161.3955526468546395, -5.529849536909571484, -2.068640691029946410 ) ) ;
#1431 = ORIENTED_EDGE ( 'NONE', *, *, #24879, .F. ) ;
#1432 = EDGE_CURVE ( 'NONE', #20260, #3651, #22699, .T. ) ;
#1433 = VECTOR ( 'NONE', #26147, 1000.000000000000000 ) ;
#1434 = EDGE_CURVE ( 'NONE', #2600, #448, #13380, .T. ) ;
#1435 = CARTESIAN_POINT ( 'NONE',  ( -4.763139720814407951, -2.750000000000016431, -142.0000000000000284 ) ) ;
#1436 = AXIS2_PLACEMENT_3D ( 'NONE', #24413, #622, #5066 ) ;
#1437 = VERTEX_POINT ( 'NONE', #1415 ) ;
#1438 = CARTESIAN_POINT ( 'NONE',  ( -3.608439182435052128, -6.250000000000110134, -48.44198729810783277 ) ) ;
#1439 = CARTESIAN_POINT ( 'NONE',  ( 15.81250000000000000, 0.8284271247462354770, -2.000000000000151879 ) ) ;
#1440 = ORIENTED_EDGE ( 'NONE', *, *, #20179, .F. ) ;
#1441 = CARTESIAN_POINT ( 'NONE',  ( -4.763139720814407951, 2.749999999999946709, -73.25000000000004263 ) ) ;
#1442 = CARTESIAN_POINT ( 'NONE',  ( 14.68749999999998579, -1.097466725451499370, 2.649519052838298805 ) ) ;
#1443 = CARTESIAN_POINT ( 'NONE',  ( 2.775557561562891351E-14, -6.250000000000061284, -97.18301270189222407 ) ) ;
#1444 = CARTESIAN_POINT ( 'NONE',  ( -3.979146954363663724, -10.25926384964412641, -20.49296196285819249 ) ) ;
#1445 = CARTESIAN_POINT ( 'NONE',  ( 0.000000000000000000, 5.999999999999977796, -106.7886751345948397 ) ) ;
#1446 = CARTESIAN_POINT ( 'NONE',  ( 6.000000000000014211, -1.607695154586730180, -150.7306624327026157 ) ) ;
#1447 = CARTESIAN_POINT ( 'NONE',  ( 3.464101615137757051, -5.999999999999979572, -86.41367513459481131 ) ) ;
#1448 = APPLICATION_PROTOCOL_DEFINITION ( 'draft international standard', 'automotive_design', 1998, #21649 ) ;
#1449 = CARTESIAN_POINT ( 'NONE',  ( 4.763139720814407951, 2.750000000000002665, -153.2500000000000000 ) ) ;
#1450 = CARTESIAN_POINT ( 'NONE',  ( 137.1488248654052313, -3.889087296526011706, -3.889087296526011706 ) ) ;
#1451 = DIRECTION ( 'NONE',  ( -7.147005652999508048E-36, 5.642372883946980038E-36, 1.000000000000000000 ) ) ;
#1452 = UNCERTAINTY_MEASURE_WITH_UNIT (LENGTH_MEASURE( 1.000000000000000082E-05 ), #15146, 'distance_accuracy_value', 'NONE');
#1453 = AXIS2_PLACEMENT_3D ( 'NONE', #14881, #1021, #3029 ) ;
#1454 = CARTESIAN_POINT ( 'NONE',  ( -6.350852961085760029, -1.281975124255709124E-13, -86.62500000000000000 ) ) ;
#1455 = DIRECTION ( 'NONE',  ( 1.000000000000000000, -5.551115123125773458E-17, -1.260129944081490338E-35 ) ) ;
#1456 = CARTESIAN_POINT ( 'NONE',  ( 3.175426480543072749, -5.500000000000105693, -84.62499999999998579 ) ) ;
#1457 = CARTESIAN_POINT ( 'NONE',  ( 6.000000000000000888, 1.743066579297358182E-13, -74.16367513459483973 ) ) ;
#1458 = CARTESIAN_POINT ( 'NONE',  ( 114.6488248654050324, 2.000000000000122125, -0.8284271247459350507 ) ) ;
#1459 = AXIS2_PLACEMENT_3D ( 'NONE', #19531, #5813, #4086 ) ;
#1460 = CARTESIAN_POINT ( 'NONE',  ( 111.7113248654050892, 2.000000000000057288, 0.000000000000000000 ) ) ;
#1461 = CARTESIAN_POINT ( 'NONE',  ( 119.9372167782374277, -0.7662911109077388261, 1.849990392679652151 ) ) ;
#1462 = FACE_OUTER_BOUND ( 'NONE', #8697, .T. ) ;
#1463 = EDGE_LOOP ( 'NONE', ( #15726, #20603, #7769, #24062 ) ) ;
#1464 = FACE_OUTER_BOUND ( 'NONE', #26711, .T. ) ;
#1465 = DIRECTION ( 'NONE',  ( 1.000000000000000000, 0.000000000000000000, 0.000000000000000000 ) ) ;
#1466 = CARTESIAN_POINT ( 'NONE',  ( 118.3752832217622029, 1.849990392679523588, 0.000000000000000000 ) ) ;
#1467 = EDGE_CURVE ( 'NONE', #28105, #1357, #29526, .T. ) ;
#1468 = LINE ( 'NONE', #24665, #22836 ) ;
#1469 = ORIENTED_EDGE ( 'NONE', *, *, #28809, .T. ) ;
#1470 = EDGE_CURVE ( 'NONE', #4270, #27080, #6641, .T. ) ;
#1471 = CARTESIAN_POINT ( 'NONE',  ( -4.763139720814407951, 2.749999999999946709, -97.25000000000000000 ) ) ;
#1472 = AXIS2_PLACEMENT_3D ( 'NONE', #1633, #30044, #4389 ) ;
#1473 = CARTESIAN_POINT ( 'NONE',  ( 5.196152422706629359, 3.000000000000002665, -96.53867513459479710 ) ) ;
#1474 = CARTESIAN_POINT ( 'NONE',  ( 5.412658773652712085, -3.125000000000086153, -114.9330127018922667 ) ) ;
#1475 = ORIENTED_EDGE ( 'NONE', *, *, #16946, .F. ) ;
#1476 = CARTESIAN_POINT ( 'NONE',  ( 6.000000000000000888, 7.762456499804235646E-14, -117.0863248654052171 ) ) ;
#1477 = STYLED_ITEM ( 'NONE', ( #24794 ), #15922 ) ;
#1478 = CARTESIAN_POINT ( 'NONE',  ( 139.6493076922298542, -8.798545334315203803, -8.160000000000000142 ) ) ;
#1479 = DIRECTION ( 'NONE',  ( -7.147005652999508048E-36, 5.642372883946980038E-36, 1.000000000000000000 ) ) ;
#1480 = CARTESIAN_POINT ( 'NONE',  ( -5.412658773652684552, -3.125000000000099920, -52.43301270189226670 ) ) ;
#1481 = ORIENTED_EDGE ( 'NONE', *, *, #23519, .F. ) ;
#1482 = CARTESIAN_POINT ( 'NONE',  ( 5.196152422706629359, 3.000000000000002665, -160.4613248654052029 ) ) ;
#1483 =( BOUNDED_CURVE ( )  B_SPLINE_CURVE ( 2, ( #26051, #4994, #14427, #23764, #21461, #391, #9782, #2846, #28786 ),
 .UNSPECIFIED., .F., .T. ) 
 B_SPLINE_CURVE_WITH_KNOTS ( ( 3, 2, 2, 2, 3 ),
 ( 0.08611111111111113825, 0.08703703703703702388, 0.08888888888888890616, 0.09074074074074078844, 0.09166666666666667407 ),
 .UNSPECIFIED. ) 
 CURVE ( )  GEOMETRIC_REPRESENTATION_ITEM ( )  RATIONAL_B_SPLINE_CURVE ( ( 0.9330127018922194093, 0.9330127018922234061, 1.000000000000000000, 0.8660254037844388186, 1.000000000000000000, 0.8660254037844388186, 1.000000000000000000, 0.9330127018922194093, 0.9330127018922194093 ) ) 
 REPRESENTATION_ITEM ( '' )  );
#1484 = CARTESIAN_POINT ( 'NONE',  ( 146.8199251345948539, -2.278174593052012309, -5.500000000000012434 ) ) ;
#1485 = CARTESIAN_POINT ( 'NONE',  ( 119.0238248654050466, -0.8284271247461453269, 2.000000000000091926 ) ) ;
#1486 = CARTESIAN_POINT ( 'NONE',  ( 0.000000000000000000, 5.499999999999991118, -166.4999999999999716 ) ) ;
#1487 = CARTESIAN_POINT ( 'NONE',  ( 114.4999999999998721, -2.499999999999891198, 0.000000000000000000 ) ) ;
#1488 = CARTESIAN_POINT ( 'NONE',  ( -6.350852961085760029, -1.281975124255709124E-13, -110.6249999999999716 ) ) ;
#1489 = CARTESIAN_POINT ( 'NONE',  ( 105.7738248654049897, 2.000000000000151879, 0.8284271247464157772 ) ) ;
#1490 = CARTESIAN_POINT ( 'NONE',  ( 0.000000000000000000, 5.499999999999991118, -106.5000000000000426 ) ) ;
#1491 = FACE_BOUND ( 'NONE', #4334, .T. ) ;
#1492 = CARTESIAN_POINT ( 'NONE',  ( 135.0000000000000284, -8.851767004199837530, 7.500000047444594919 ) ) ;
#1493 = ORIENTED_EDGE ( 'NONE', *, *, #29535, .F. ) ;
#1494 = CARTESIAN_POINT ( 'NONE',  ( 15.81250000000009237, 1.097466725451619718, 2.649519052838419153 ) ) ;
#1495 = CARTESIAN_POINT ( 'NONE',  ( 115.9374999999998010, 2.500000000000055067, -1.035533905932629173 ) ) ;
#1496 = VECTOR ( 'NONE', #7971, 1000.000000000000000 ) ;
#1497 = CARTESIAN_POINT ( 'NONE',  ( 111.8127832217621460, -1.849990392679441875, 0.7662911109079489913 ) ) ;
#1498 = DIRECTION ( 'NONE',  ( 1.000000000000000000, -5.551115123125773458E-17, -1.260129944081490338E-35 ) ) ;
#1499 = ORIENTED_EDGE ( 'NONE', *, *, #30014, .F. ) ;
#1500 = CARTESIAN_POINT ( 'NONE',  ( 4.763139720814407951, -2.749999999999988454, -158.0000000000000284 ) ) ;
#1501 = PRESENTATION_LAYER_ASSIGNMENT (  '', '', ( #14778 ) ) ;
#1502 = CARTESIAN_POINT ( 'NONE',  ( 2.775557561562891351E-14, -6.250000000000061284, -79.81698729810781856 ) ) ;
#1503 = CARTESIAN_POINT ( 'NONE',  ( 149.6175748654052882, 5.500000000000012434, -2.278174593052012309 ) ) ;
#1504 = ORIENTED_EDGE ( 'NONE', *, *, #4500, .T. ) ;
#1505 = FACE_OUTER_BOUND ( 'NONE', #16602, .T. ) ;
#1506 = EDGE_CURVE ( 'NONE', #10100, #16147, #23761, .T. ) ;
#1507 = AXIS2_PLACEMENT_3D ( 'NONE', #7070, #30110, #16484 ) ;
#1508 = EDGE_LOOP ( 'NONE', ( #12148, #15683, #3081, #29216 ) ) ;
#1509 = CARTESIAN_POINT ( 'NONE',  ( 154.0312500000000568, -2.485281374238555774, -6.000000000000005329 ) ) ;
#1510 = CARTESIAN_POINT ( 'NONE',  ( 3.175426480543072749, -5.500000000000105693, -119.1250000000000142 ) ) ;
#1511 = CARTESIAN_POINT ( 'NONE',  ( 3.608439182435180470, -6.249999999999997335, -137.5580127018922099 ) ) ;
#1512 = ORIENTED_EDGE ( 'NONE', *, *, #19591, .F. ) ;
#1513 = CARTESIAN_POINT ( 'NONE',  ( 156.8363248654052313, 0.000000000000000000, -5.500000000000005329 ) ) ;
#1514 = CARTESIAN_POINT ( 'NONE',  ( -5.412658773652739619, 3.124999999999975131, -123.8169872981078612 ) ) ;
#1515 = CARTESIAN_POINT ( 'NONE',  ( 2.775557561562891351E-14, -6.250000000000061284, -175.8169872981077901 ) ) ;
#1516 = CARTESIAN_POINT ( 'NONE',  ( -3.175426480542816510, 5.499999999999865885, -169.3750000000000853 ) ) ;
#1517 = CARTESIAN_POINT ( 'NONE',  ( -4.999999999999990230, -24.99999999999999289, 8.000000000000007105 ) ) ;
#1518 = AXIS2_PLACEMENT_3D ( 'NONE', #6966, #23719, #12077 ) ;
#1519 = ORIENTED_EDGE ( 'NONE', *, *, #17212, .T. ) ;
#1520 = CARTESIAN_POINT ( 'NONE',  ( 13.25000000000017764, 5.551115123125782702E-14, 1.999999999999890754 ) ) ;
#1521 = LINE ( 'NONE', #3819, #9306 ) ;
#1522 = CARTESIAN_POINT ( 'NONE',  ( 159.6319105802860179, -11.40177967602063269, -3.791719585355142641 ) ) ;
#1523 = CARTESIAN_POINT ( 'NONE',  ( 140.3363248654052029, 0.000000000000000000, -5.500000000000005329 ) ) ;
#1524 = VECTOR ( 'NONE', #23636, 1000.000000000000000 ) ;
#1525 = CARTESIAN_POINT ( 'NONE',  ( 6.000000000000000888, -1.859271017917181981E-14, -46.58632486540520290 ) ) ;
#1526 = CARTESIAN_POINT ( 'NONE',  ( 112.8127832217621886, -1.849990392679441875, 0.7662911109079489913 ) ) ;
#1527 = CARTESIAN_POINT ( 'NONE',  ( 5.412658773652739619, 3.124999999999988898, -65.81698729810780435 ) ) ;
#1528 = CARTESIAN_POINT ( 'NONE',  ( -5.412658773652739619, 3.124999999999975131, -54.81698729810779724 ) ) ;
#1529 = CARTESIAN_POINT ( 'NONE',  ( 136.0000000000000284, 0.000000000000000000, 0.000000000000000000 ) ) ;
#1530 = CARTESIAN_POINT ( 'NONE',  ( -4.763139720814407951, -2.750000000000016431, -52.00000000000004263 ) ) ;
#1531 = CARTESIAN_POINT ( 'NONE',  ( -5.999999999999971578, 1.607695154586715303, -55.48066243270262987 ) ) ;
#1532 = LINE ( 'NONE', #1995, #6368 ) ;
#1533 = CARTESIAN_POINT ( 'NONE',  ( -6.350852961085760029, -1.281975124255709124E-13, -133.1250000000000284 ) ) ;
#1534 = FACE_OUTER_BOUND ( 'NONE', #3335, .T. ) ;
#1535 = EDGE_CURVE ( 'NONE', #19344, #17248, #8802, .T. ) ;
#1536 = ORIENTED_EDGE ( 'NONE', *, *, #23552, .F. ) ;
#1537 = CARTESIAN_POINT ( 'NONE',  ( 24.25000000000010658, -1.873492889144789952, -1.873492889145123019 ) ) ;
#1538 = EDGE_CURVE ( 'NONE', #9651, #18552, #14062, .T. ) ;
#1539 =( BOUNDED_CURVE ( )  B_SPLINE_CURVE ( 2, ( #28814, #7630, #26217, #3313, #14875, #22080, #10113, #21930, #17040 ),
 .UNSPECIFIED., .F., .F. ) 
 B_SPLINE_CURVE_WITH_KNOTS ( ( 3, 2, 2, 2, 3 ),
 ( 0.8916666666666666075, 0.8925925925925926041, 0.8944444444444444864, 0.8962962962962962576, 0.8972222222222222543 ),
 .UNSPECIFIED. ) 
 CURVE ( )  GEOMETRIC_REPRESENTATION_ITEM ( )  RATIONAL_B_SPLINE_CURVE ( ( 0.9330127018922194093, 0.9330127018922154125, 1.000000000000000000, 0.8660254037844388186, 1.000000000000000000, 0.8660254037844388186, 1.000000000000000000, 0.9330127018922154125, 0.9330127018922194093 ) ) 
 REPRESENTATION_ITEM ( '' )  );
#1540 = CARTESIAN_POINT ( 'NONE',  ( 6.000000000000000888, -1.859271017917181981E-14, -58.58632486540521001 ) ) ;
#1541 = DIRECTION ( 'NONE',  ( 1.000000000000000000, -5.551115123125773458E-17, -1.260129944081490338E-35 ) ) ;
#1542 = CARTESIAN_POINT ( 'NONE',  ( 137.8273502691896510, -5.000000000000004441, 0.000000000000000000 ) ) ;
#1543 = ORIENTED_EDGE ( 'NONE', *, *, #25275, .T. ) ;
#1544 = CARTESIAN_POINT ( 'NONE',  ( 113.8122167782374987, 0.7662911109077987781, 1.849990392679652151 ) ) ;
#1545 = CARTESIAN_POINT ( 'NONE',  ( -5.999999999999963585, -1.487416814333745711E-14, -71.33632486540521711 ) ) ;
#1546 = CARTESIAN_POINT ( 'NONE',  ( 113.9761751345945839, -0.8284271247461453269, -1.999999999999791278 ) ) ;
#1547 = CARTESIAN_POINT ( 'NONE',  ( -5.412658773652739619, 3.124999999999975131, -119.3169872981078043 ) ) ;
#1548 = VECTOR ( 'NONE', #5368, 1000.000000000000000 ) ;
#1549 = CARTESIAN_POINT ( 'NONE',  ( 135.0000000000000284, 5.402039670393428139, -2.232486041264207799 ) ) ;
#1550 = EDGE_CURVE ( 'NONE', #22257, #29700, #23095, .T. ) ;
#1551 = EDGE_CURVE ( 'NONE', #30268, #2318, #19624, .T. ) ;
#1552 = CARTESIAN_POINT ( 'NONE',  ( 110.5238248654050608, 0.8284271247463257382, -1.999999999999731104 ) ) ;
#1553 = ORIENTED_EDGE ( 'NONE', *, *, #7638, .F. ) ;
#1554 = DIRECTION ( 'NONE',  ( 1.000000000000000000, -5.551115123125773458E-17, -1.260129944081490338E-35 ) ) ;
#1555 = CARTESIAN_POINT ( 'NONE',  ( 140.9062500000000568, 6.000000000000005329, -2.485281374238555774 ) ) ;
#1556 = ORIENTED_EDGE ( 'NONE', *, *, #13694, .F. ) ;
#1557 = COLOUR_RGB ( '', 0.66274510, 0.83137255, 0.94901961) ;
#1558 = ORIENTED_EDGE ( 'NONE', *, *, #20639, .T. ) ;
#1559 = FILL_AREA_STYLE ('',( #25345 ) ) ;
#1560 = CARTESIAN_POINT ( 'NONE',  ( -6.350852961085760029, -1.281975124255709124E-13, -50.62500000000001421 ) ) ;
#1561 = CARTESIAN_POINT ( 'NONE',  ( 24.43750000000014921, -1.999999999999851674, 0.8284271247462354770 ) ) ;
#1562 =( NAMED_UNIT ( * ) SI_UNIT ( $, .STERADIAN. ) SOLID_ANGLE_UNIT ( ) );
#1563 = CARTESIAN_POINT ( 'NONE',  ( -5.999999999999956479, -1.607695154586745057, -80.26933756729744118 ) ) ;
#1564 = CARTESIAN_POINT ( 'NONE',  ( 5.412658773652712085, -3.125000000000086153, -65.43301270189222407 ) ) ;
#1565 = CARTESIAN_POINT ( 'NONE',  ( 152.2351497308104342, 3.535533905932725318, -3.535533905932725318 ) ) ;
#1566 = CARTESIAN_POINT ( 'NONE',  ( 135.0000000000000284, 1.949781249179022291, 5.142796231657420947 ) ) ;
#1567 = DIRECTION ( 'NONE',  ( 0.000000000000000000, -0.8907235428302476832, 0.4545454545454524764 ) ) ;
#1568 = DIRECTION ( 'NONE',  ( 1.000000000000000000, 0.000000000000000000, 0.000000000000000000 ) ) ;
#1569 = VECTOR ( 'NONE', #12546, 1000.000000000000000 ) ;
#1570 = CARTESIAN_POINT ( 'NONE',  ( 6.000000000000000888, -1.859271017917181981E-14, -93.66367513459481131 ) ) ;
#1571 = CARTESIAN_POINT ( 'NONE',  ( 3.175426480543072749, -5.500000000000105693, -134.1250000000000284 ) ) ;
#1572 = CARTESIAN_POINT ( 'NONE',  ( 2.775557561562891351E-14, 6.250000000000033751, -148.9330127018922383 ) ) ;
#1573 = CARTESIAN_POINT ( 'NONE',  ( 14.22617513459491256, 2.500000000000144773, -1.035533905932689347 ) ) ;
#1574 = VERTEX_POINT ( 'NONE', #20789 ) ;
#1575 = EDGE_CURVE ( 'NONE', #8510, #9581, #30137, .T. ) ;
#1576 = CARTESIAN_POINT ( 'NONE',  ( 3.175426480543072749, 5.499999999999865885, -61.62500000000001421 ) ) ;
#1577 = CARTESIAN_POINT ( 'NONE',  ( 0.000000000000000000, -5.999999999999991118, -76.96132486540518869 ) ) ;
#1578 =( BOUNDED_CURVE ( )  B_SPLINE_CURVE ( 2, ( #24390, #7794, #1038, #19787, #25134, #13365, #5946, #20258, #27140 ),
 .UNSPECIFIED., .F., .T. ) 
 B_SPLINE_CURVE_WITH_KNOTS ( ( 3, 2, 2, 2, 3 ),
 ( 0.07812500000000000000, 0.08593750000000000000, 0.09375000000000000000, 0.1015625000000000000, 0.1093750000000000000 ),
 .UNSPECIFIED. ) 
 CURVE ( )  GEOMETRIC_REPRESENTATION_ITEM ( )  RATIONAL_B_SPLINE_CURVE ( ( 1.000000000000000000, 0.9238795325112867385, 1.000000000000000000, 0.9238795325112867385, 1.000000000000000000, 0.9238795325112867385, 1.000000000000000000, 0.9238795325112867385, 1.000000000000000000 ) ) 
 REPRESENTATION_ITEM ( '' )  );
#1579 = ORIENTED_EDGE ( 'NONE', *, *, #3648, .F. ) ;
#1580 = CARTESIAN_POINT ( 'NONE',  ( 108.5624999999997442, -2.499999999999934719, -1.035533905932568777 ) ) ;
#1581 = CARTESIAN_POINT ( 'NONE',  ( 145.6875000000000284, 4.242640687119269671, 4.242640687119298093 ) ) ;
#1582 = DIRECTION ( 'NONE',  ( 0.000000000000000000, -1.000000000000000000, 0.000000000000000000 ) ) ;
#1583 = AXIS2_PLACEMENT_3D ( 'NONE', #28607, #19132, #14405 ) ;
#1584 = CARTESIAN_POINT ( 'NONE',  ( 105.2113248654051745, -1.999999999999974021, 0.000000000000000000 ) ) ;
#1585 = ADVANCED_FACE ( 'NONE', ( #6941 ), #16360, .T. ) ;
#1586 =( BOUNDED_CURVE ( )  B_SPLINE_CURVE ( 2, ( #26131, #21396, #7254, #25986, #4931, #14362, #2634, #12054, #7541 ),
 .UNSPECIFIED., .F., .T. ) 
 B_SPLINE_CURVE_WITH_KNOTS ( ( 3, 2, 2, 2, 3 ),
 ( 0.4472222222222221877, 0.4481481481481481843, 0.4499999999999999556, 0.4518518518518518379, 0.4527777777777778345 ),
 .UNSPECIFIED. ) 
 CURVE ( )  GEOMETRIC_REPRESENTATION_ITEM ( )  RATIONAL_B_SPLINE_CURVE ( ( 0.9330127018922194093, 0.9330127018922154125, 1.000000000000000000, 0.8660254037844388186, 1.000000000000000000, 0.8660254037844388186, 1.000000000000000000, 0.9330127018922154125, 0.9330127018922194093 ) ) 
 REPRESENTATION_ITEM ( '' )  );
#1587 = EDGE_CURVE ( 'NONE', #23232, #688, #22775, .T. ) ;
#1588 = ORIENTED_EDGE ( 'NONE', *, *, #15099, .T. ) ;
#1589 = CARTESIAN_POINT ( 'NONE',  ( 139.6875000000000284, 4.242640687119269671, 4.242640687119298093 ) ) ;
#1590 = CARTESIAN_POINT ( 'NONE',  ( 161.2720946962140260, -5.187633567512120791, 2.550615076069009834 ) ) ;
#1591 = ORIENTED_EDGE ( 'NONE', *, *, #11046, .F. ) ;
#1592 = CARTESIAN_POINT ( 'NONE',  ( -2.775557561562891351E-14, -5.500000000000115463, -149.2500000000000000 ) ) ;
#1593 = ORIENTED_EDGE ( 'NONE', *, *, #12719, .F. ) ;
#1594 = CARTESIAN_POINT ( 'NONE',  ( 13.75000000000006750, 2.220446049250313081E-13, -2.000000000000001776 ) ) ;
#1595 = ORIENTED_EDGE ( 'NONE', *, *, #20144, .T. ) ;
#1596 = CARTESIAN_POINT ( 'NONE',  ( -4.763139720814407951, 2.749999999999946709, -76.25000000000004263 ) ) ;
#1597 = CARTESIAN_POINT ( 'NONE',  ( 14.43750000000004974, 2.649519052838419153, 1.097466725451439196 ) ) ;
#1598 = CARTESIAN_POINT ( 'NONE',  ( -5.412658773652739619, 3.124999999999975131, -90.18301270189222407 ) ) ;
#1599 =( GEOMETRIC_REPRESENTATION_CONTEXT ( 3 ) GLOBAL_UNCERTAINTY_ASSIGNED_CONTEXT ( ( #9739 ) ) GLOBAL_UNIT_ASSIGNED_CONTEXT ( ( #1638, #26049, #7009 ) ) REPRESENTATION_CONTEXT ( 'NONE', 'WORKASPACE' ) );
#1600 = DIRECTION ( 'NONE',  ( -7.147005652999508048E-36, 5.642372883946980038E-36, 1.000000000000000000 ) ) ;
#1601 = CARTESIAN_POINT ( 'NONE',  ( 147.8363248654052029, 0.000000000000000000, -5.500000000000005329 ) ) ;
#1602 = CARTESIAN_POINT ( 'NONE',  ( 135.1170309136356877, -7.914290706147571797, -8.323885487687906704 ) ) ;
#1603 = FACE_OUTER_BOUND ( 'NONE', #20031, .T. ) ;
#1604 = PRODUCT_CONTEXT ( 'NONE', #13648, 'mechanical' ) ;
#1605 = CARTESIAN_POINT ( 'NONE',  ( 4.763139720814407951, 2.750000000000002665, -156.2500000000000000 ) ) ;
#1606 = CARTESIAN_POINT ( 'NONE',  ( 17.89882486540517093, 1.035533905932749299, 2.499999999999964473 ) ) ;
#1607 = CARTESIAN_POINT ( 'NONE',  ( -3.847734726282651341, 4.353436196510543255, -179.9999999999999716 ) ) ;
#1608 = EDGE_CURVE ( 'NONE', #11104, #7154, #629, .T. ) ;
#1609 = CARTESIAN_POINT ( 'NONE',  ( 4.763139720814407951, -2.749999999999988454, -84.50000000000001421 ) ) ;
#1610 = CARTESIAN_POINT ( 'NONE',  ( -5.999999999999963585, 8.134310703387671600E-14, -140.9136751345947971 ) ) ;
#1611 = CARTESIAN_POINT ( 'NONE',  ( -3.175426480542816510, -5.500000000000057732, -74.37500000000000000 ) ) ;
#1612 = TOROIDAL_SURFACE ( 'NONE', #14425, 6.000000000000000888, 5.000000000000000888 ) ;
#1613 = CARTESIAN_POINT ( 'NONE',  ( 0.000000000000000000, -5.999999999999991118, -120.4613248654052313 ) ) ;
#1614 = CARTESIAN_POINT ( 'NONE',  ( 151.7023502691896510, 0.000000000000000000, -5.000000000000004441 ) ) ;
#1615 = CARTESIAN_POINT ( 'NONE',  ( -5.196152422706573404, -3.000000000000002665, -108.7113248654052455 ) ) ;
#1616 = CARTESIAN_POINT ( 'NONE',  ( 0.000000000000000000, -5.999999999999991118, -149.5386751345948539 ) ) ;
#1617 = CARTESIAN_POINT ( 'NONE',  ( 20.81250000000014211, 0.8284271247461753029, -2.000000000000091926 ) ) ;
#1618 = DIRECTION ( 'NONE',  ( 0.000000000000000000, -1.000000000000000000, 0.000000000000000000 ) ) ;
#1619 = CARTESIAN_POINT ( 'NONE',  ( 150.5550748654052313, -5.500000000000012434, -2.278174593052012309 ) ) ;
#1620 = EDGE_CURVE ( 'NONE', #1154, #14874, #25896, .T. ) ;
#1621 = CARTESIAN_POINT ( 'NONE',  ( 5.999999999999949374, 1.607695154586804565, -75.59668783648704959 ) ) ;
#1622 = ORIENTED_EDGE ( 'NONE', *, *, #4777, .T. ) ;
#1623 = CARTESIAN_POINT ( 'NONE',  ( 157.4062500000000284, 6.000000000000005329, -2.485281374238555774 ) ) ;
#1624 = CARTESIAN_POINT ( 'NONE',  ( -0.004063854759415918595, -15.42149627498952569, 6.273580390957694597 ) ) ;
#1625 = ORIENTED_EDGE ( 'NONE', *, *, #20597, .F. ) ;
#1626 = ORIENTED_EDGE ( 'NONE', *, *, #5088, .F. ) ;
#1627 = CARTESIAN_POINT ( 'NONE',  ( -3.175426480542816510, -5.500000000000057732, -101.3750000000000000 ) ) ;
#1628 = CARTESIAN_POINT ( 'NONE',  ( 16.68750000000013856, -1.097466725451439196, 2.649519052838178457 ) ) ;
#1629 = CARTESIAN_POINT ( 'NONE',  ( 5.999999999999949374, 1.607695154586804565, -96.59668783648702117 ) ) ;
#1630 = CARTESIAN_POINT ( 'NONE',  ( 7.216878364870455975, -6.409875621278545621E-14, -113.3080127018922241 ) ) ;
#1631 = AXIS2_PLACEMENT_3D ( 'NONE', #14570, #21174, #9946 ) ;
#1632 = CARTESIAN_POINT ( 'NONE',  ( 5.196152422706629359, 3.000000000000002665, -140.9613248654052597 ) ) ;
#1633 = CARTESIAN_POINT ( 'NONE',  ( 5.551115123125782702E-14, 1.999999999999890754, -200.0000000000000000 ) ) ;
#1634 = CARTESIAN_POINT ( 'NONE',  ( 3.464101615137757051, -5.999999999999979572, -143.4136751345948255 ) ) ;
#1635 = CARTESIAN_POINT ( 'NONE',  ( 5.412658773652712085, -3.125000000000086153, -51.93301270189220986 ) ) ;
#1636 = ORIENTED_EDGE ( 'NONE', *, *, #13213, .F. ) ;
#1637 = CARTESIAN_POINT ( 'NONE',  ( 116.0000000000000142, 6.735557395310442023E-16, 5.500000000000000000 ) ) ;
#1638 =( LENGTH_UNIT ( ) NAMED_UNIT ( * ) SI_UNIT ( .MILLI., .METRE. ) );
#1639 = CARTESIAN_POINT ( 'NONE',  ( 157.4136751345948539, 0.000000000000000000, -5.500000000000005329 ) ) ;
#1640 = CARTESIAN_POINT ( 'NONE',  ( 5.196152422706629359, 3.000000000000002665, -136.4613248654051745 ) ) ;
#1641 = CARTESIAN_POINT ( 'NONE',  ( -3.175426480542816510, 5.499999999999865885, -161.8750000000000568 ) ) ;
#1642 = CARTESIAN_POINT ( 'NONE',  ( 114.6874999999997300, -1.035533905932689347, -2.499999999999784173 ) ) ;
#1643 = CARTESIAN_POINT ( 'NONE',  ( -0.07850599468832326899, -14.93747518635459137, 8.093769840972308671 ) ) ;
#1644 = ADVANCED_FACE ( 'NONE', ( #11569 ), #25657, .T. ) ;
#1645 = CARTESIAN_POINT ( 'NONE',  ( 6.350852961086080661, -9.614813431917819062E-14, -109.8750000000000426 ) ) ;
#1646 = CARTESIAN_POINT ( 'NONE',  ( 106.2113248654051745, -1.999999999999946265, 0.000000000000000000 ) ) ;
#1647 = CARTESIAN_POINT ( 'NONE',  ( 6.000000000000026645, -1.607695154586707753, -122.2306624327026014 ) ) ;
#1648 = EDGE_CURVE ( 'NONE', #20340, #20437, #27789, .T. ) ;
#1649 = CARTESIAN_POINT ( 'NONE',  ( 0.000000000000000000, 5.499999999999991118, -99.00000000000002842 ) ) ;
#1650 = CARTESIAN_POINT ( 'NONE',  ( -5.999999999999962697, 3.323446944526963891E-14, -151.4136751345948255 ) ) ;
#1651 = CARTESIAN_POINT ( 'NONE',  ( 141.1011751345948539, 3.889087296526011706, -3.889087296526011706 ) ) ;
#1652 = CYLINDRICAL_SURFACE ( 'NONE', #16550, 30.00000000000000000 ) ;
#1653 = VERTEX_POINT ( 'NONE', #18617 ) ;
#1654 = CARTESIAN_POINT ( 'NONE',  ( 14.06250000000011546, -2.649519052838238409, 1.097466725451559322 ) ) ;
#1655 = CARTESIAN_POINT ( 'NONE',  ( 116.0624999999999005, 2.500000000000055067, 1.035533905932929599 ) ) ;
#1656 = CARTESIAN_POINT ( 'NONE',  ( 108.8752832217621744, -1.849990392679468076, 1.110223024625156540E-13 ) ) ;
#1657 = CARTESIAN_POINT ( 'NONE',  ( 107.7738248654050466, 2.000000000000061728, 0.8284271247463557142 ) ) ;
#1658 = EDGE_LOOP ( 'NONE', ( #28483, #28368, #823, #7689 ) ) ;
#1659 = LINE ( 'NONE', #27591, #6925 ) ;
#1660 = TOROIDAL_SURFACE ( 'NONE', #18861, 15.99999999999999289, 1.000000000000000000 ) ;
#1661 = CARTESIAN_POINT ( 'NONE',  ( 108.3122167782374135, -0.7662911109077388261, -1.849990392679351725 ) ) ;
#1662 = CARTESIAN_POINT ( 'NONE',  ( 3.608439182435180470, 6.249999999999982236, -89.69198729810783277 ) ) ;
#1663 = CARTESIAN_POINT ( 'NONE',  ( 6.000000000000000888, 7.762456499804234384E-14, -129.0863248654052029 ) ) ;
#1664 = VERTEX_POINT ( 'NONE', #13570 ) ;
#1665 = CARTESIAN_POINT ( 'NONE',  ( -3.978158145384737221, 10.25965056898454009, -29.50791791133369912 ) ) ;
#1666 = CARTESIAN_POINT ( 'NONE',  ( 3.175426480543072749, 5.499999999999865885, -151.6250000000000284 ) ) ;
#1667 = EDGE_LOOP ( 'NONE', ( #23038, #23188, #19873, #8884 ) ) ;
#1668 = CARTESIAN_POINT ( 'NONE',  ( 155.9062500000000853, 6.000000000000005329, -2.485281374238555774 ) ) ;
#1669 = CARTESIAN_POINT ( 'NONE',  ( -2.775557561562891351E-14, -5.500000000000115463, -125.2500000000000284 ) ) ;
#1670 =( BOUNDED_CURVE ( )  B_SPLINE_CURVE ( 2, ( #12028, #23816, #21367, #16488, #25814, #9694, #28398, #21524, #449 ),
 .UNSPECIFIED., .F., .T. ) 
 B_SPLINE_CURVE_WITH_KNOTS ( ( 3, 2, 2, 2, 3 ),
 ( 0.7694444444444443754, 0.7703703703703703720, 0.7722222222222222543, 0.7740740740740740256, 0.7750000000000000222 ),
 .UNSPECIFIED. ) 
 CURVE ( )  GEOMETRIC_REPRESENTATION_ITEM ( )  RATIONAL_B_SPLINE_CURVE ( ( 0.9330127018922194093, 0.9330127018922154125, 1.000000000000000000, 0.8660254037844388186, 1.000000000000000000, 0.8660254037844388186, 1.000000000000000000, 0.9330127018922154125, 0.9330127018922194093 ) ) 
 REPRESENTATION_ITEM ( '' )  );
#1671 = CARTESIAN_POINT ( 'NONE',  ( 7.216878364870455975, -6.409875621278545621E-14, -138.8080127018922667 ) ) ;
#1672 = VERTEX_POINT ( 'NONE', #27635 ) ;
#1673 = CARTESIAN_POINT ( 'NONE',  ( 6.000000000000000000, 2.951592740943527306E-14, -156.6636751345948255 ) ) ;
#1674 = CARTESIAN_POINT ( 'NONE',  ( -5.412658773652739619, 3.124999999999975131, -120.8169872981078612 ) ) ;
#1675 = CARTESIAN_POINT ( 'NONE',  ( 7.216878364870455975, -6.409875621278545621E-14, -178.4419872981078470 ) ) ;
#1676 = CARTESIAN_POINT ( 'NONE',  ( -4.763139720814407951, 2.749999999999946709, -172.2500000000000000 ) ) ;
#1677 = CARTESIAN_POINT ( 'NONE',  ( 159.9406005586360209, -11.50931141900650978, 3.432783163228085410 ) ) ;
#1678 = LINE ( 'NONE', #14418, #25045 ) ;
#1679 = ORIENTED_EDGE ( 'NONE', *, *, #24279, .T. ) ;
#1680 = CARTESIAN_POINT ( 'NONE',  ( 162.0000000000000284, 0.000000000000000000, 0.000000000000000000 ) ) ;
#1681 = CARTESIAN_POINT ( 'NONE',  ( 141.0000000000000284, -12.00000000000001066, 4.000000000000003553 ) ) ;
#1682 = CARTESIAN_POINT ( 'NONE',  ( 159.2682291426874599, -12.02340987637674097, -3.972341123820091191 ) ) ;
#1683 = CARTESIAN_POINT ( 'NONE',  ( -5.999999999999963585, -1.487416814333745711E-14, -128.3363248654052029 ) ) ;
#1684 = DIRECTION ( 'NONE',  ( -7.147005652999508048E-36, 5.642372883946980038E-36, 1.000000000000000000 ) ) ;
#1685 = CARTESIAN_POINT ( 'NONE',  ( 3.608439182435180470, -6.249999999999997335, -76.69198729810784698 ) ) ;
#1686 = CARTESIAN_POINT ( 'NONE',  ( 5.412658773652712085, -3.125000000000086153, -60.06698729810783277 ) ) ;
#1687 = CARTESIAN_POINT ( 'NONE',  ( -3.464101615137757051, -5.999999999999979572, -121.1636751345947829 ) ) ;
#1688 = CARTESIAN_POINT ( 'NONE',  ( -6.350852961085760029, -1.281975124255709124E-13, -49.12500000000000711 ) ) ;
#1689 = CARTESIAN_POINT ( 'NONE',  ( -4.999999999999990230, -55.00000000000002132, 8.000000000000007105 ) ) ;
#1690 = DIRECTION ( 'NONE',  ( -1.734723475976824844E-16, 1.000000000000000000, 0.000000000000000000 ) ) ;
#1691 = EDGE_CURVE ( 'NONE', #24822, #4865, #27940, .T. ) ;
#1692 = CARTESIAN_POINT ( 'NONE',  ( 4.763139720814407951, 2.750000000000002665, -127.7500000000000284 ) ) ;
#1693 = CARTESIAN_POINT ( 'NONE',  ( -5.196152422706601826, 2.999999999999975131, -50.46132486540522422 ) ) ;
#1694 = ORIENTED_EDGE ( 'NONE', *, *, #28303, .T. ) ;
#1695 = CARTESIAN_POINT ( 'NONE',  ( -6.000000000000060396, -1.607695154586566089, -119.2693375672974554 ) ) ;
#1696 = CARTESIAN_POINT ( 'NONE',  ( 160.4925748654052597, 2.278174593051894625, 5.500000000000129674 ) ) ;
#1697 = CARTESIAN_POINT ( 'NONE',  ( 138.4836002691896510, 4.999999999999989342, -2.071067811865468400 ) ) ;
#1698 = CARTESIAN_POINT ( 'NONE',  ( 6.000000000000000888, -1.607695154586752384, -147.7306624327026157 ) ) ;
#1699 = VERTEX_POINT ( 'NONE', #6614 ) ;
#1700 = CARTESIAN_POINT ( 'NONE',  ( 108.6247167782375271, 1.849990392679551343, 0.000000000000000000 ) ) ;
#1701 =( LENGTH_UNIT ( ) NAMED_UNIT ( * ) SI_UNIT ( .MILLI., .METRE. ) );
#1702 = CARTESIAN_POINT ( 'NONE',  ( 15.02382486540530238, -1.035533905932568999, 2.499999999999784173 ) ) ;
#1703 = CARTESIAN_POINT ( 'NONE',  ( -5.412658773652739619, 3.124999999999975131, -116.3169872981078043 ) ) ;
#1704 = CARTESIAN_POINT ( 'NONE',  ( 140.5126264503620916, -11.05212133306707578, -4.674908800639064665 ) ) ;
#1705 = CARTESIAN_POINT ( 'NONE',  ( 6.000000000000000888, -1.859271017917181981E-14, -135.6636751345948255 ) ) ;
#1706 = VERTEX_POINT ( 'NONE', #21217 ) ;
#1707 = DIRECTION ( 'NONE',  ( -7.147005652999508048E-36, 5.642372883946980038E-36, 1.000000000000000000 ) ) ;
#1708 = CARTESIAN_POINT ( 'NONE',  ( 139.1250000000000284, 0.000000000000000000, -6.000000000000005329 ) ) ;
#1709 = B_SPLINE_CURVE_WITH_KNOTS ( 'NONE', 3,
 ( #26383, #5330, #29279, #1643, #20388, #13063, #15828, #11199 ),
 .UNSPECIFIED., .F., .F.,
 ( 4, 2, 2, 4 ),
 ( 0.000000000000000000, 0.0005811766152209535885, 0.0008717649228314284853, 0.001162353230441903491 ),
 .UNSPECIFIED. ) ;
#1710 = VERTEX_POINT ( 'NONE', #9537 ) ;
#1711 = EDGE_LOOP ( 'NONE', ( #1006, #16931, #8148, #24469 ) ) ;
#1712 = EDGE_CURVE ( 'NONE', #16735, #152, #4458, .T. ) ;
#1713 = CARTESIAN_POINT ( 'NONE',  ( 4.763139720814407951, -2.749999999999988454, -47.00000000000004263 ) ) ;
#1714 = CARTESIAN_POINT ( 'NONE',  ( 22.31250000000002842, -0.8284271247460552878, 2.000000000000031530 ) ) ;
#1715 = CARTESIAN_POINT ( 'NONE',  ( 117.5386751345946692, 5.551115123125782702E-14, 2.000000000000223821 ) ) ;
#1716 = CARTESIAN_POINT ( 'NONE',  ( 136.3199251345947971, -2.278174593052089136, -5.499999999999934275 ) ) ;
#1717 = CARTESIAN_POINT ( 'NONE',  ( 5.412658773652712085, -3.125000000000086153, -66.93301270189222407 ) ) ;
#1718 = CARTESIAN_POINT ( 'NONE',  ( 152.4226497308104058, 5.000000000000004441, 0.000000000000000000 ) ) ;
#1719 = CARTESIAN_POINT ( 'NONE',  ( 0.000000000000000000, 0.000000000000000000, 0.000000000000000000 ) ) ;
#1720 = CARTESIAN_POINT ( 'NONE',  ( 140.0000000000000284, -12.00000000000001066, 4.000000000000003553 ) ) ;
#1721 = CARTESIAN_POINT ( 'NONE',  ( 12.03867513459491789, 1.665334536937734811E-13, -2.500000000000057732 ) ) ;
#1722 = SURFACE_STYLE_USAGE ( .BOTH. , #13434 ) ;
#1723 =( BOUNDED_SURFACE ( )  B_SPLINE_SURFACE ( 3, 2, ( 
 ( #19669, #7676, #22126 ),
 ( #29316, #5811, #5365 ),
 ( #17087, #7974, #15069 ),
 ( #1068, #26414, #10458 ),
 ( #14773, #8274, #15228 ),
 ( #17688, #27014, #5979 ) ),
 .UNSPECIFIED., .F., .F., .F. ) 
 B_SPLINE_SURFACE_WITH_KNOTS ( ( 4, 2, 4 ),
 ( 3, 3 ),
 ( 0.02423702093288230414, 0.02523827330272541969, 0.02623952567256853524 ),
 ( 0.000000000000000000, 1.000000000000000000 ),
 .UNSPECIFIED. ) 
 GEOMETRIC_REPRESENTATION_ITEM ( )  RATIONAL_B_SPLINE_SURFACE ( (
 ( 1.000000000000000000, 0.7071067811865475727, 1.000000000000000000),
 ( 1.000000000000000000, 0.7329025660702759293, 1.000000000000000000),
 ( 1.000000000000000000, 0.7587231434688260778, 1.000000000000000000),
 ( 1.000000000000000000, 0.8097046771148294075, 1.000000000000000000),
 ( 1.000000000000000000, 0.8349103174451857345, 1.000000000000000000),
 ( 1.000000000000000000, 0.8593225670956807782, 1.000000000000000000) ) ) 
 REPRESENTATION_ITEM ( '' )  SURFACE ( )  );
#1724 = CARTESIAN_POINT ( 'NONE',  ( 106.5386751345947971, 1.110223024625156540E-13, 2.000000000000001776 ) ) ;
#1725 = EDGE_CURVE ( 'NONE', #12068, #283, #5873, .T. ) ;
#1726 = CARTESIAN_POINT ( 'NONE',  ( -6.350852961085760029, -1.281975124255709124E-13, -124.1250000000000426 ) ) ;
#1727 = CYLINDRICAL_SURFACE ( 'NONE', #6676, 2.499999999999999112 ) ;
#1728 = ORIENTED_EDGE ( 'NONE', *, *, #3030, .F. ) ;
#1729 = CARTESIAN_POINT ( 'NONE',  ( 6.350852961086080661, -9.614813431917819062E-14, -64.87500000000001421 ) ) ;
#1730 = CARTESIAN_POINT ( 'NONE',  ( 0.000000000000000000, 5.999999999999977796, -124.2113248654052029 ) ) ;
#1731 = CYLINDRICAL_SURFACE ( 'NONE', #14058, 6.000000000000000888 ) ;
#1732 = VERTEX_POINT ( 'NONE', #11419 ) ;
#1733 = VECTOR ( 'NONE', #1707, 1000.000000000000000 ) ;
#1734 = CARTESIAN_POINT ( 'NONE',  ( 107.3749999999999574, -1.767766952966293159, 1.767766952966431937 ) ) ;
#1735 = CARTESIAN_POINT ( 'NONE',  ( 145.4062500000000284, 6.000000000000005329, -2.485281374238556218 ) ) ;
#1736 = CARTESIAN_POINT ( 'NONE',  ( 6.000000000000000888, 7.762456499804235646E-14, -119.1636751345948113 ) ) ;
#1737 = DIRECTION ( 'NONE',  ( 0.000000000000000000, 0.000000000000000000, 1.000000000000000000 ) ) ;
#1738 = VERTEX_POINT ( 'NONE', #23375 ) ;
#1739 = VECTOR ( 'NONE', #11454, 1000.000000000000000 ) ;
#1740 = CARTESIAN_POINT ( 'NONE',  ( 6.350852961086080661, -9.614813431917819062E-14, -144.3750000000000568 ) ) ;
#1741 = ORIENTED_EDGE ( 'NONE', *, *, #4930, .T. ) ;
#1742 = CARTESIAN_POINT ( 'NONE',  ( 11.93750000000008527, 2.000000000000091926, -0.8284271247462354770 ) ) ;
#1743 = ORIENTED_EDGE ( 'NONE', *, *, #5754, .F. ) ;
#1744 = EDGE_CURVE ( 'NONE', #13355, #26790, #5902, .T. ) ;
#1745 = CARTESIAN_POINT ( 'NONE',  ( 4.763139720814407951, -2.749999999999988454, -72.50000000000001421 ) ) ;
#1746 = CARTESIAN_POINT ( 'NONE',  ( 18.16367513459488237, 1.767766952966487448, -1.767766952966487448 ) ) ;
#1747 = CARTESIAN_POINT ( 'NONE',  ( -7.216878364870328078, 0.000000000000000000, -88.55801270189223828 ) ) ;
#1748 = TOROIDAL_SURFACE ( 'NONE', #18963, 16.00000000000000000, 1.000000000000000000 ) ;
#1749 = CARTESIAN_POINT ( 'NONE',  ( -3.677985992802528692, -10.37237449091587038, -20.24368265486285168 ) ) ;
#1750 = CARTESIAN_POINT ( 'NONE',  ( 6.000000000000000888, 1.743066579297358182E-13, -107.1636751345948539 ) ) ;
#1751 = CARTESIAN_POINT ( 'NONE',  ( 112.8511751345945981, -1.999999999999941602, -0.8284271247459952248 ) ) ;
#1752 = CARTESIAN_POINT ( 'NONE',  ( 0.000000000000000000, 0.000000000000000000, 0.000000000000000000 ) ) ;
#1753 = EDGE_CURVE ( 'NONE', #6341, #1235, #24733, .T. ) ;
#1754 = APPLICATION_PROTOCOL_DEFINITION ( 'draft international standard', 'automotive_design', 1998, #14794 ) ;
#1755 =( BOUNDED_CURVE ( )  B_SPLINE_CURVE ( 2, ( #27471, #3832, #22448, #22601, #16026, #4300, #10791, #6447, #13718 ),
 .UNSPECIFIED., .F., .T. ) 
 B_SPLINE_CURVE_WITH_KNOTS ( ( 3, 2, 2, 2, 3 ),
 ( 0.3194444444444444753, 0.3203703703703703609, 0.3222222222222222432, 0.3240740740740740700, 0.3250000000000000111 ),
 .UNSPECIFIED. ) 
 CURVE ( )  GEOMETRIC_REPRESENTATION_ITEM ( )  RATIONAL_B_SPLINE_CURVE ( ( 0.9330127018922194093, 0.9330127018922214077, 1.000000000000000000, 0.8660254037844388186, 1.000000000000000000, 0.8660254037844388186, 1.000000000000000000, 0.9330127018922194093, 0.9330127018922194093 ) ) 
 REPRESENTATION_ITEM ( '' )  );
#1756 = CARTESIAN_POINT ( 'NONE',  ( 3.175426480543072749, 5.499999999999865885, -153.1250000000000853 ) ) ;
#1757 = CARTESIAN_POINT ( 'NONE',  ( 139.5000000000000284, -9.165151389911676105, -8.000000000000007105 ) ) ;
#1758 = CARTESIAN_POINT ( 'NONE',  ( 156.2738248654052029, -3.889087296526011706, 3.889087296526011706 ) ) ;
#1759 = AXIS2_PLACEMENT_3D ( 'NONE', #7502, #24234, #23956 ) ;
#1760 = CARTESIAN_POINT ( 'NONE',  ( -4.763139720814407951, -2.750000000000016431, -88.00000000000002842 ) ) ;
#1761 = CARTESIAN_POINT ( 'NONE',  ( -4.763139720814407951, 2.749999999999946709, -74.75000000000004263 ) ) ;
#1762 = CARTESIAN_POINT ( 'NONE',  ( 149.4523502691896510, 0.000000000000000000, 5.000000000000004441 ) ) ;
#1763 = CARTESIAN_POINT ( 'NONE',  ( -5.999999999999963585, 1.780251999655701777E-13, -51.83632486540522422 ) ) ;
#1764 = CARTESIAN_POINT ( 'NONE',  ( 104.8415063509460055, -1.908493649053821795, 1.110223024625156540E-13 ) ) ;
#1765 = CARTESIAN_POINT ( 'NONE',  ( -5.999999999999956479, -1.607695154586745057, -76.34668783648700696 ) ) ;
#1766 = DIRECTION ( 'NONE',  ( 0.000000000000000000, -1.000000000000000000, 0.000000000000000000 ) ) ;
#1767 = CARTESIAN_POINT ( 'NONE',  ( 20.12500000000011369, 1.414213562373201061, 1.414213562373034527 ) ) ;
#1768 = CARTESIAN_POINT ( 'NONE',  ( 5.999999999999974243, 1.607695154586759934, -119.0966878364870354 ) ) ;
#1769 = CARTESIAN_POINT ( 'NONE',  ( -5.196152422706601826, 2.999999999999975131, -134.4613248654051745 ) ) ;
#1770 = CARTESIAN_POINT ( 'NONE',  ( 6.000000000000000888, -3.330669073875464691E-16, -7.560779664488942560E-35 ) ) ;
#1771 = ORIENTED_EDGE ( 'NONE', *, *, #19013, .T. ) ;
#1772 = CARTESIAN_POINT ( 'NONE',  ( 155.3437500000000284, -6.000000000000005329, -2.485281374238555774 ) ) ;
#1773 = CARTESIAN_POINT ( 'NONE',  ( 14.77382486540530770, 2.500000000000144773, 1.035533905932689347 ) ) ;
#1774 = CARTESIAN_POINT ( 'NONE',  ( 116.1252832217622881, -5.551115123125782702E-14, -1.849990392679412565 ) ) ;
#1775 = CARTESIAN_POINT ( 'NONE',  ( -3.464101615137725076, 5.999999999999979572, -157.0863248654051745 ) ) ;
#1776 = ORIENTED_EDGE ( 'NONE', *, *, #20790, .T. ) ;
#1777 = AXIS2_PLACEMENT_3D ( 'NONE', #6671, #27688, #16241 ) ;
#1778 = EDGE_LOOP ( 'NONE', ( #21927, #2761, #24888, #28248 ) ) ;
#1779 = EDGE_CURVE ( 'NONE', #25181, #20028, #27857, .T. ) ;
#1780 = CARTESIAN_POINT ( 'NONE',  ( 4.763139720814407951, -2.749999999999988454, -101.0000000000000284 ) ) ;
#1781 = LINE ( 'NONE', #29587, #20442 ) ;
#1782 = CARTESIAN_POINT ( 'NONE',  ( 3.608439182435180470, 6.249999999999982236, -104.0580127018922383 ) ) ;
#1783 = SURFACE_SIDE_STYLE ('',( #1942 ) ) ;
#1784 = CARTESIAN_POINT ( 'NONE',  ( -3.175426480542816510, 5.499999999999865885, -163.3750000000000568 ) ) ;
#1785 = CARTESIAN_POINT ( 'NONE',  ( 5.412658773652712085, -3.125000000000086153, -53.43301270189226670 ) ) ;
#1786 = FACE_OUTER_BOUND ( 'NONE', #8972, .T. ) ;
#1787 = ORIENTED_EDGE ( 'NONE', *, *, #19661, .F. ) ;
#1788 = EDGE_CURVE ( 'NONE', #688, #9162, #25493, .T. ) ;
#1789 = CARTESIAN_POINT ( 'NONE',  ( 0.000000000000000000, 0.000000000000000000, 0.000000000000000000 ) ) ;
#1790 = CARTESIAN_POINT ( 'NONE',  ( 6.350852961086080661, -9.614813431917819062E-14, -159.3750000000000284 ) ) ;
#1791 = CARTESIAN_POINT ( 'NONE',  ( 115.4999999999998153, -2.499999999999891198, 0.000000000000000000 ) ) ;
#1792 = AXIS2_PLACEMENT_3D ( 'NONE', #5987, #22896, #8917 ) ;
#1793 = CARTESIAN_POINT ( 'NONE',  ( 10.39882486540515849, -1.035533905932629173, -2.500000000000024425 ) ) ;
#1794 = CARTESIAN_POINT ( 'NONE',  ( 4.763139720814407951, -2.749999999999988454, -105.5000000000000426 ) ) ;
#1795 = CARTESIAN_POINT ( 'NONE',  ( 106.0863248654050750, -1.414213562373090038, 1.414213562373145550 ) ) ;
#1796 = CARTESIAN_POINT ( 'NONE',  ( 146.2425748654051745, -2.278174593052290753, -5.499999999999732658 ) ) ;
#1797 = CARTESIAN_POINT ( 'NONE',  ( 3.175426480543072749, -5.500000000000105693, -101.1250000000000000 ) ) ;
#1798 = CARTESIAN_POINT ( 'NONE',  ( 159.5773502691896510, 5.000000000000004441, 0.000000000000000000 ) ) ;
#1799 = CARTESIAN_POINT ( 'NONE',  ( -3.464101615137725076, 5.999999999999979572, -162.1636751345948824 ) ) ;
#1800 = CARTESIAN_POINT ( 'NONE',  ( -0.06962969976386645943, -14.74801126815780528, 8.209584733985920479 ) ) ;
#1801 = VERTEX_POINT ( 'NONE', #30414 ) ;
#1802 = CARTESIAN_POINT ( 'NONE',  ( 11.62500000000010658, 2.649519052838444910, -1.110223024625156540E-13 ) ) ;
#1803 = CARTESIAN_POINT ( 'NONE',  ( 117.2499999999998721, 0.000000000000000000, 2.499999999999946709 ) ) ;
#1804 = CARTESIAN_POINT ( 'NONE',  ( 111.5002832217621602, 1.308140751793723799, 1.308140751793640533 ) ) ;
#1805 = CARTESIAN_POINT ( 'NONE',  ( 108.0863248654051603, -1.414213562373062283, 1.414213562373367594 ) ) ;
#1806 = VERTEX_POINT ( 'NONE', #14612 ) ;
#1807 = DIRECTION ( 'NONE',  ( -1.000000000000000000, -6.938893903907222067E-15, 0.000000000000000000 ) ) ;
#1808 = CARTESIAN_POINT ( 'NONE',  ( 108.8747167782374987, 0.000000000000000000, 1.849990392679523588 ) ) ;
#1809 = CARTESIAN_POINT ( 'NONE',  ( -3.608439182435115633, 6.249999999999965361, -89.44198729810784698 ) ) ;
#1810 = EDGE_LOOP ( 'NONE', ( #11720, #30071, #1258, #8892 ) ) ;
#1811 = VECTOR ( 'NONE', #9109, 1000.000000000000000 ) ;
#1812 = CARTESIAN_POINT ( 'NONE',  ( 5.196152422706629359, -2.999999999999988898, -65.28867513459479710 ) ) ;
#1813 = AXIS2_PLACEMENT_3D ( 'NONE', #14799, #12808, #24141 ) ;
#1814 = ORIENTED_EDGE ( 'NONE', *, *, #25969, .F. ) ;
#1815 = CARTESIAN_POINT ( 'NONE',  ( 156.3750000000000284, 0.000000000000000000, 6.000000000000005329 ) ) ;
#1816 = ORIENTED_EDGE ( 'NONE', *, *, #5303, .T. ) ;
#1817 = EDGE_CURVE ( 'NONE', #9159, #21560, #599, .T. ) ;
#1818 = CARTESIAN_POINT ( 'NONE',  ( -2.775557561562891351E-14, -5.500000000000115463, -117.7500000000000284 ) ) ;
#1819 = CARTESIAN_POINT ( 'NONE',  ( 10.37500000000005151, -1.414213562373034527, 1.414213562372756972 ) ) ;
#1820 = EDGE_CURVE ( 'NONE', #30157, #28361, #13821, .T. ) ;
#1821 = CARTESIAN_POINT ( 'NONE',  ( 2.775557561562891351E-14, -6.250000000000061284, -128.6830127018922383 ) ) ;
#1822 = ORIENTED_EDGE ( 'NONE', *, *, #29117, .T. ) ;
#1823 = CARTESIAN_POINT ( 'NONE',  ( -4.999999999999990230, -55.00000000000002132, 7.500000000000007105 ) ) ;
#1824 = CARTESIAN_POINT ( 'NONE',  ( -5.412658773652684552, -3.125000000000099920, -126.5669872981078328 ) ) ;
#1825 = CARTESIAN_POINT ( 'NONE',  ( -5.412658773652684552, -3.125000000000099920, -176.0669872981078186 ) ) ;
#1826 = CARTESIAN_POINT ( 'NONE',  ( 116.0000000000000142, 0.000000000000000000, 0.000000000000000000 ) ) ;
#1827 = VERTEX_POINT ( 'NONE', #9692 ) ;
#1828 = CARTESIAN_POINT ( 'NONE',  ( 11.62499999999999645, -1.414213562373090038, -1.414213562373090038 ) ) ;
#1829 = CARTESIAN_POINT ( 'NONE',  ( 0.1950273200666285678, -15.66255992321438129, -7.807776097887585642 ) ) ;
#1830 = DIRECTION ( 'NONE',  ( -7.147005652999508048E-36, 5.642372883946980038E-36, 1.000000000000000000 ) ) ;
#1831 = CARTESIAN_POINT ( 'NONE',  ( 5.196152422706629359, 3.000000000000002665, -90.53867513459485394 ) ) ;
#1832 = DIRECTION ( 'NONE',  ( 0.000000000000000000, 0.000000000000000000, 1.000000000000000000 ) ) ;
#1833 = FACE_OUTER_BOUND ( 'NONE', #5210, .T. ) ;
#1834 = CARTESIAN_POINT ( 'NONE',  ( 112.6877832217621034, -0.7662911109076184779, 1.849990392679652151 ) ) ;
#1835 = AXIS2_PLACEMENT_3D ( 'NONE', #27414, #24668, #6086 ) ;
#1836 = CARTESIAN_POINT ( 'NONE',  ( -3.608439182435052128, -6.250000000000110134, -72.44198729810781856 ) ) ;
#1837 = CARTESIAN_POINT ( 'NONE',  ( 3.608439182435180470, -6.249999999999997335, -58.69198729810781856 ) ) ;
#1838 = DIRECTION ( 'NONE',  ( 1.000000000000000000, -6.938893903907221278E-15, 0.000000000000000000 ) ) ;
#1839 = CARTESIAN_POINT ( 'NONE',  ( -3.175426480542816510, -5.500000000000057732, -48.87500000000001421 ) ) ;
#1840 = CARTESIAN_POINT ( 'NONE',  ( -1.000000000000002665, -9.000000000000007105, -4.000000000000005329 ) ) ;
#1841 = DIRECTION ( 'NONE',  ( -1.000000000000000000, 5.551115123125774690E-17, 0.000000000000000000 ) ) ;
#1842 = AXIS2_PLACEMENT_3D ( 'NONE', #17174, #24348, #2706 ) ;
#1843 = CARTESIAN_POINT ( 'NONE',  ( 0.000000000000000000, 5.499999999999991118, -118.5000000000000568 ) ) ;
#1844 = CARTESIAN_POINT ( 'NONE',  ( 104.7401757384972143, -1.604125865985250865, -0.9294237407942756990 ) ) ;
#1845 = ORIENTED_EDGE ( 'NONE', *, *, #4106, .T. ) ;
#1846 = CARTESIAN_POINT ( 'NONE',  ( 21.12500000000011724, -2.649519052838222866, 0.000000000000000000 ) ) ;
#1847 = CARTESIAN_POINT ( 'NONE',  ( 6.000000000000000888, 7.762456499804234384E-14, -123.0863248654052313 ) ) ;
#1848 = CARTESIAN_POINT ( 'NONE',  ( 139.6086002691896795, -2.071067811865468400, -4.999999999999989342 ) ) ;
#1849 = ORIENTED_EDGE ( 'NONE', *, *, #13796, .T. ) ;
#1850 = CARTESIAN_POINT ( 'NONE',  ( 109.5622167782374277, 1.849990392679501827, -0.7662911109077087390 ) ) ;
#1851 = CARTESIAN_POINT ( 'NONE',  ( 112.1247167782376124, -1.849990392679579099, 1.110223024625156540E-13 ) ) ;
#1852 = CARTESIAN_POINT ( 'NONE',  ( -3.608439182435052128, -6.250000000000110134, -117.4419872981078328 ) ) ;
#1853 = CARTESIAN_POINT ( 'NONE',  ( -6.000000000000007105, -1.607695154586655129, -110.2693375672973986 ) ) ;
#1854 =( BOUNDED_CURVE ( )  B_SPLINE_CURVE ( 2, ( #28256, #9546, #6919, #16345, #11730, #3, #9388, #11888, #18938 ),
 .UNSPECIFIED., .F., .T. ) 
 B_SPLINE_CURVE_WITH_KNOTS ( ( 3, 2, 2, 2, 3 ),
 ( 0.3125000000000007772, 0.3187500000000005329, 0.3250000000000003442, 0.3312500000000000444, 0.3374999999999998557 ),
 .UNSPECIFIED. ) 
 CURVE ( )  GEOMETRIC_REPRESENTATION_ITEM ( )  RATIONAL_B_SPLINE_CURVE ( ( 0.9999999999999905631, 0.9238795325112961754, 1.000000000000000000, 0.9238795325112867385, 1.000000000000000000, 0.9238795325112867385, 1.000000000000000000, 0.9238795325112887369, 0.9999999999999980016 ) ) 
 REPRESENTATION_ITEM ( '' )  );
#1855 = CARTESIAN_POINT ( 'NONE',  ( 110.3988248654048760, -0.8284271247461453269, -1.999999999999731104 ) ) ;
#1856 = ORIENTED_EDGE ( 'NONE', *, *, #21549, .F. ) ;
#1857 = ORIENTED_EDGE ( 'NONE', *, *, #20790, .F. ) ;
#1858 = CARTESIAN_POINT ( 'NONE',  ( 160.0000000000000000, -12.58734484189959879, 3.130213737083505698 ) ) ;
#1859 = CARTESIAN_POINT ( 'NONE',  ( 142.5937500000000568, 6.000000000000005329, 2.485281374238585972 ) ) ;
#1860 = AXIS2_PLACEMENT_3D ( 'NONE', #30009, #23122, #20498 ) ;
#1861 = EDGE_CURVE ( 'NONE', #21664, #269, #5048, .T. ) ;
#1862 = CARTESIAN_POINT ( 'NONE',  ( 5.412658773652739619, 3.124999999999988898, -149.8169872981078186 ) ) ;
#1863 = ORIENTED_EDGE ( 'NONE', *, *, #20873, .T. ) ;
#1864 =( NAMED_UNIT ( * ) SI_UNIT ( $, .STERADIAN. ) SOLID_ANGLE_UNIT ( ) );
#1865 = CARTESIAN_POINT ( 'NONE',  ( 119.9999999999999289, 2.500000000000057732, 1.110223024625156540E-13 ) ) ;
#1866 = CARTESIAN_POINT ( 'NONE',  ( 23.56250000000009948, -1.999999999999851674, -0.8284271247462354770 ) ) ;
#1867 = FACE_OUTER_BOUND ( 'NONE', #29364, .T. ) ;
#1868 = DIRECTION ( 'NONE',  ( 0.000000000000000000, 0.000000000000000000, -1.000000000000000000 ) ) ;
#1869 = CARTESIAN_POINT ( 'NONE',  ( -3.608439182435115633, 6.249999999999965361, -67.80801270189226670 ) ) ;
#1870 = CARTESIAN_POINT ( 'NONE',  ( 143.7976497308104058, 0.000000000000000000, 5.000000000000004441 ) ) ;
#1871 = CARTESIAN_POINT ( 'NONE',  ( 3.464101615137852974, 5.999999999999884537, -177.4136751345947971 ) ) ;
#1872 = CYLINDRICAL_SURFACE ( 'NONE', #16767, 6.000000000000000888 ) ;
#1873 = CARTESIAN_POINT ( 'NONE',  ( 3.464101615137757051, -5.999999999999979572, -155.4136751345947687 ) ) ;
#1874 = CARTESIAN_POINT ( 'NONE',  ( 129.9999999999998010, -89.00000000000001421, 4.000000000000003553 ) ) ;
#1875 = CARTESIAN_POINT ( 'NONE',  ( 109.0624999999997584, 2.500000000000054623, 1.035533905932809473 ) ) ;
#1876 = CARTESIAN_POINT ( 'NONE',  ( 106.7261751345945413, -1.999999999999941602, 0.8284271247462955401 ) ) ;
#1877 = CARTESIAN_POINT ( 'NONE',  ( 4.763139720814407951, 2.750000000000002665, -126.2500000000000284 ) ) ;
#1878 = CARTESIAN_POINT ( 'NONE',  ( 116.0000000000000142, 0.000000000000000000, -5.500000000000000000 ) ) ;
#1879 = DIRECTION ( 'NONE',  ( -1.000000000000000000, -1.665334536937731113E-16, 1.526556658859586792E-16 ) ) ;
#1880 = ORIENTED_EDGE ( 'NONE', *, *, #14063, .T. ) ;
#1881 = CARTESIAN_POINT ( 'NONE',  ( 6.350852961086080661, -9.614813431917819062E-14, -58.87500000000004974 ) ) ;
#1882 = CARTESIAN_POINT ( 'NONE',  ( 3.464101615137757051, -5.999999999999979572, -153.9136751345947971 ) ) ;
#1883 = CARTESIAN_POINT ( 'NONE',  ( 6.000000000000000888, 1.743066579297358182E-13, -70.58632486540523132 ) ) ;
#1884 = CARTESIAN_POINT ( 'NONE',  ( 6.000000000000014211, -1.607695154586730180, -162.7306624327026725 ) ) ;
#1885 = EDGE_LOOP ( 'NONE', ( #8262, #17030, #26038, #26441 ) ) ;
#1886 = CARTESIAN_POINT ( 'NONE',  ( 106.4999999999999147, -2.499999999999946709, 1.110223024625156540E-13 ) ) ;
#1887 = CARTESIAN_POINT ( 'NONE',  ( 147.5625000000000284, -4.242640687119298093, 4.242640687119298093 ) ) ;
#1888 = CARTESIAN_POINT ( 'NONE',  ( 160.7409933946964031, -11.42047333460522474, -3.685613295175590665 ) ) ;
#1889 = EDGE_CURVE ( 'NONE', #14191, #4494, #24102, .T. ) ;
#1890 = CARTESIAN_POINT ( 'NONE',  ( 108.2886751345946834, 2.000000000000057288, 2.220446049250313081E-13 ) ) ;
#1891 = CARTESIAN_POINT ( 'NONE',  ( 141.0937500000000000, 6.000000000000005329, 2.485281374238585972 ) ) ;
#1892 = CARTESIAN_POINT ( 'NONE',  ( 119.6874999999998010, -1.035533905932809473, -2.499999999999784173 ) ) ;
#1893 = SHAPE_REPRESENTATION ( 'Handle knob', ( #18805 ), #12932 ) ;
#1894 = CARTESIAN_POINT ( 'NONE',  ( 6.350852961086080661, -9.614813431917819062E-14, -139.8750000000000568 ) ) ;
#1895 = EDGE_CURVE ( 'NONE', #29849, #22223, #25723, .T. ) ;
#1896 = ORIENTED_EDGE ( 'NONE', *, *, #30228, .T. ) ;
#1897 = CARTESIAN_POINT ( 'NONE',  ( 13.37500000000019185, -1.414213562372979016, 1.414213562372979016 ) ) ;
#1898 = ORIENTED_EDGE ( 'NONE', *, *, #21254, .T. ) ;
#1899 = CARTESIAN_POINT ( 'NONE',  ( 0.000000000000000000, 5.499999999999991118, -69.00000000000000000 ) ) ;
#1900 = CARTESIAN_POINT ( 'NONE',  ( -5.196152422706573404, -3.000000000000002665, -164.7886751345948255 ) ) ;
#1901 = CARTESIAN_POINT ( 'NONE',  ( 7.216878364870455975, -6.409875621278545621E-14, -90.80801270189223828 ) ) ;
#1902 = CARTESIAN_POINT ( 'NONE',  ( 10.31249999999998934, -0.8284271247461753029, 1.999999999999911626 ) ) ;
#1903 = CARTESIAN_POINT ( 'NONE',  ( 119.9999999999999574, -0.4876318259219858398, 1.939643060552387333 ) ) ;
#1904 = CARTESIAN_POINT ( 'NONE',  ( -3.464101615137725076, 5.999999999999979572, -106.6636751345948397 ) ) ;
#1905 = CARTESIAN_POINT ( 'NONE',  ( 112.9761751345945981, -0.8284271247461153509, -1.999999999999610978 ) ) ;
#1906 = CARTESIAN_POINT ( 'NONE',  ( 0.000000000000000000, 0.000000000000000000, 0.000000000000000000 ) ) ;
#1907 = CARTESIAN_POINT ( 'NONE',  ( 119.2502832217621886, 1.308140751793612777, -1.308140751793418488 ) ) ;
#1908 = DIRECTION ( 'NONE',  ( -2.418687190290953473E-16, 0.3950055220923761601, -0.9186787455452148921 ) ) ;
#1909 = CARTESIAN_POINT ( 'NONE',  ( 3.175426480543072749, -5.500000000000105693, -144.6250000000000000 ) ) ;
#1910 = DIRECTION ( 'NONE',  ( -0.000000000000000000, -0.000000000000000000, -1.000000000000000000 ) ) ;
#1911 = CARTESIAN_POINT ( 'NONE',  ( -6.350852961085760029, -1.281975124255709124E-13, -142.1250000000000000 ) ) ;
#1912 = CARTESIAN_POINT ( 'NONE',  ( 5.412658773652739619, 3.124999999999988898, -159.6830127018922099 ) ) ;
#1913 = DIRECTION ( 'NONE',  ( 1.000000000000000000, -5.551115123125773458E-17, -1.260129944081490338E-35 ) ) ;
#1914 = CYLINDRICAL_SURFACE ( 'NONE', #18404, 6.000000000000000888 ) ;
#1915 = CARTESIAN_POINT ( 'NONE',  ( 4.763139720814407951, -2.749999999999988454, -77.00000000000001421 ) ) ;
#1916 = CYLINDRICAL_SURFACE ( 'NONE', #246, 1.000000000000000000 ) ;
#1917 = CARTESIAN_POINT ( 'NONE',  ( -3.175426480542816510, 5.499999999999865885, -73.37500000000000000 ) ) ;
#1918 = CARTESIAN_POINT ( 'NONE',  ( 0.000000000000000000, 0.000000000000000000, 0.000000000000000000 ) ) ;
#1919 = DIRECTION ( 'NONE',  ( -7.147005652999508048E-36, 5.642372883946980038E-36, 1.000000000000000000 ) ) ;
#1920 = DIRECTION ( 'NONE',  ( -7.147005652999508048E-36, 5.642372883946980038E-36, 1.000000000000000000 ) ) ;
#1921 = EDGE_CURVE ( 'NONE', #12335, #28542, #1586, .T. ) ;
#1922 = DIRECTION ( 'NONE',  ( 0.000000000000000000, -1.000000000000000000, 0.000000000000000000 ) ) ;
#1923 = PRESENTATION_STYLE_ASSIGNMENT (( #23590 ) ) ;
#1924 = CARTESIAN_POINT ( 'NONE',  ( 19.68750000000015632, -0.8284271247461152399, -1.999999999999971800 ) ) ;
#1925 = EDGE_CURVE ( 'NONE', #28690, #12627, #5379, .T. ) ;
#1926 = CARTESIAN_POINT ( 'NONE',  ( 5.196152422706629359, 3.000000000000002665, -55.46132486540522422 ) ) ;
#1927 = CARTESIAN_POINT ( 'NONE',  ( 116.4997167782376266, 1.308140751793640533, -1.308140751793640533 ) ) ;
#1928 = DIRECTION ( 'NONE',  ( 0.000000000000000000, 0.000000000000000000, -1.000000000000000000 ) ) ;
#1929 = ORIENTED_EDGE ( 'NONE', *, *, #6081, .F. ) ;
#1930 = CIRCLE ( 'NONE', #21567, 11.00000000000000355 ) ;
#1931 = CARTESIAN_POINT ( 'NONE',  ( 154.1250000000000284, 0.000000000000000000, -6.000000000000005329 ) ) ;
#1932 = CARTESIAN_POINT ( 'NONE',  ( -3.464101615137757051, -5.999999999999979572, -157.1636751345947971 ) ) ;
#1933 = CARTESIAN_POINT ( 'NONE',  ( -5.999999999999963585, 0.000000000000000000, -179.3363248654052313 ) ) ;
#1934 = ORIENTED_EDGE ( 'NONE', *, *, #2161, .T. ) ;
#1935 = VERTEX_POINT ( 'NONE', #329 ) ;
#1936 = EDGE_CURVE ( 'NONE', #25911, #13576, #10683, .T. ) ;
#1937 = EDGE_CURVE ( 'NONE', #15812, #4583, #4725, .T. ) ;
#1938 = ORIENTED_EDGE ( 'NONE', *, *, #29081, .F. ) ;
#1939 = CARTESIAN_POINT ( 'NONE',  ( -4.763139720814407951, 2.749999999999946709, -95.75000000000000000 ) ) ;
#1940 =( BOUNDED_CURVE ( )  B_SPLINE_CURVE ( 2, ( #3758, #16104, #27701, #6682, #23138, #6828, #7134 ),
 .UNSPECIFIED., .F., .T. ) 
 B_SPLINE_CURVE_WITH_KNOTS ( ( 3, 2, 2, 3 ),
 ( 0.02366385240269184426, 0.02499999999999995975, 0.03124999999999976755, 0.03749999999999957534 ),
 .UNSPECIFIED. ) 
 CURVE ( )  GEOMETRIC_REPRESENTATION_ITEM ( )  RATIONAL_B_SPLINE_CURVE ( ( 0.9744113160502365645, 0.9837266912414370790, 1.000000000000000000, 0.9238795325112867385, 1.000000000000000000, 0.9238795325112918455, 0.9999999999999948930 ) ) 
 REPRESENTATION_ITEM ( '' )  );
#1941 = CARTESIAN_POINT ( 'NONE',  ( 7.216878364870455975, -6.409875621278545621E-14, -105.8080127018922525 ) ) ;
#1942 = SURFACE_STYLE_FILL_AREA ( #6545 ) ;
#1943 = CARTESIAN_POINT ( 'NONE',  ( 107.2886751345947118, 2.000000000000085265, 1.110223024625156540E-13 ) ) ;
#1944 = CARTESIAN_POINT ( 'NONE',  ( -2.775557561562891351E-14, -5.500000000000115463, -162.7500000000000000 ) ) ;
#1945 = CARTESIAN_POINT ( 'NONE',  ( 1.581364418632522639, -10.89278420593270447, -30.80148057605385503 ) ) ;
#1946 = AXIS2_PLACEMENT_3D ( 'NONE', #13470, #19888, #10701 ) ;
#1947 = ORIENTED_EDGE ( 'NONE', *, *, #20230, .F. ) ;
#1948 = CYLINDRICAL_SURFACE ( 'NONE', #24486, 6.000000000000000888 ) ;
#1949 = CYLINDRICAL_SURFACE ( 'NONE', #13935, 6.000000000000000888 ) ;
#1950 = CIRCLE ( 'NONE', #25490, 1.000000000000000000 ) ;
#1951 = CARTESIAN_POINT ( 'NONE',  ( -2.775557561562891351E-14, -5.500000000000115463, -174.7500000000000284 ) ) ;
#1952 = CARTESIAN_POINT ( 'NONE',  ( 23.41367513459491434, 1.767766952966487448, 1.767766952966098870 ) ) ;
#1953 = CARTESIAN_POINT ( 'NONE',  ( 4.763139720814407951, 2.750000000000002665, -159.2500000000000000 ) ) ;
#1954 = AXIS2_PLACEMENT_3D ( 'NONE', #14886, #23796, #2730 ) ;
#1955 = CARTESIAN_POINT ( 'NONE',  ( 115.0624999999998153, 2.499999999999994671, 1.035533905932929599 ) ) ;
#1956 = CARTESIAN_POINT ( 'NONE',  ( -4.763139720814407951, 2.749999999999946709, -112.2500000000000142 ) ) ;
#1957 = CYLINDRICAL_SURFACE ( 'NONE', #10992, 6.000000000000000888 ) ;
#1958 = CARTESIAN_POINT ( 'NONE',  ( -19.49999999999998224, -25.00000000000010658, 7.500000000000007105 ) ) ;
#1959 = CARTESIAN_POINT ( 'NONE',  ( 3.175426480543072749, 5.499999999999865885, -96.12500000000004263 ) ) ;
#1960 = CARTESIAN_POINT ( 'NONE',  ( 159.0148502691896510, -3.535533905932725318, -3.535533905932725318 ) ) ;
#1961 = CARTESIAN_POINT ( 'NONE',  ( 0.8347181576680260395, -15.41331385233628382, 8.287403863818649796 ) ) ;
#1962 = ORIENTED_EDGE ( 'NONE', *, *, #10188, .T. ) ;
#1963 = CARTESIAN_POINT ( 'NONE',  ( 10.43750000000010658, 1.097466725451619718, -2.649519052838358757 ) ) ;
#1964 = CARTESIAN_POINT ( 'NONE',  ( 116.7499999999997584, 1.665334536937734811E-13, -2.499999999999724665 ) ) ;
#1965 = EDGE_CURVE ( 'NONE', #20877, #1086, #237, .T. ) ;
#1966 = CARTESIAN_POINT ( 'NONE',  ( 16.53867513459489302, 5.551115123125782702E-14, 2.500000000000002220 ) ) ;
#1967 = CARTESIAN_POINT ( 'NONE',  ( 157.7886751345948255, 5.500000000000005329, 0.000000000000000000 ) ) ;
#1968 = ORIENTED_EDGE ( 'NONE', *, *, #5524, .F. ) ;
#1969 = CARTESIAN_POINT ( 'NONE',  ( 110.0863248654050466, -1.414213562373090038, 1.414213562373256572 ) ) ;
#1970 = CARTESIAN_POINT ( 'NONE',  ( 3.608439182435180470, -6.249999999999997335, -90.19198729810784698 ) ) ;
#1971 = MECHANICAL_DESIGN_GEOMETRIC_PRESENTATION_REPRESENTATION (  '', ( #20620 ), #8337 ) ;
#1972 = ORIENTED_EDGE ( 'NONE', *, *, #12405, .F. ) ;
#1973 = ADVANCED_FACE ( 'NONE', ( #27029 ), #15723, .F. ) ;
#1974 = EDGE_CURVE ( 'NONE', #21999, #20568, #22925, .T. ) ;
#1975 = CARTESIAN_POINT ( 'NONE',  ( 148.6875000000000284, 4.242640687119269671, 4.242640687119298093 ) ) ;
#1976 = CARTESIAN_POINT ( 'NONE',  ( 6.350852961086080661, -9.614813431917819062E-14, -120.3750000000000142 ) ) ;
#1977 = CARTESIAN_POINT ( 'NONE',  ( 23.81250000000003553, -2.649519052838298805, 1.097466725451559322 ) ) ;
#1978 = CARTESIAN_POINT ( 'NONE',  ( -5.412658773652684552, -3.125000000000099920, -131.9330127018922383 ) ) ;
#1979 = EDGE_LOOP ( 'NONE', ( #12993, #26078, #15721, #25258 ) ) ;
#1980 = CARTESIAN_POINT ( 'NONE',  ( 157.1175748654052029, 5.500000000000012434, -2.278174593052012309 ) ) ;
#1981 = CARTESIAN_POINT ( 'NONE',  ( 5.412658773652712085, -3.125000000000086153, -166.5669872981078186 ) ) ;
#1982 = CARTESIAN_POINT ( 'NONE',  ( -5.412658773652739619, 3.124999999999975131, -177.8169872981077901 ) ) ;
#1983 = CARTESIAN_POINT ( 'NONE',  ( 5.196152422706629359, 3.000000000000002665, -147.5386751345948539 ) ) ;
#1984 = VERTEX_POINT ( 'NONE', #1540 ) ;
#1985 = CARTESIAN_POINT ( 'NONE',  ( 111.1011751345945413, 0.8284271247462654530, -1.999999999999851674 ) ) ;
#1986 = CARTESIAN_POINT ( 'NONE',  ( 109.6011751345946266, -0.8284271247461453269, 2.000000000000212275 ) ) ;
#1987 = DIRECTION ( 'NONE',  ( 1.000000000000000000, 0.000000000000000000, 0.000000000000000000 ) ) ;
#1988 = CARTESIAN_POINT ( 'NONE',  ( -0.5000000000000004441, -15.00000000000001421, 8.000000000000007105 ) ) ;
#1989 = CARTESIAN_POINT ( 'NONE',  ( 110.2502832217623165, 1.308140751793640533, -1.308140751793640533 ) ) ;
#1990 = CARTESIAN_POINT ( 'NONE',  ( 7.216878364870455975, -6.409875621278545621E-14, -74.94198729810783277 ) ) ;
#1991 = CARTESIAN_POINT ( 'NONE',  ( 5.412658773652712085, -3.125000000000086153, -61.56698729810783277 ) ) ;
#1992 = CARTESIAN_POINT ( 'NONE',  ( 5.999999999999949374, 1.607695154586804565, -111.0193375672974270 ) ) ;
#1993 = CARTESIAN_POINT ( 'NONE',  ( 3.175426480543072749, -5.500000000000105693, -50.12500000000001421 ) ) ;
#1994 = CARTESIAN_POINT ( 'NONE',  ( 5.196152422706629359, 3.000000000000002665, -103.4613248654052171 ) ) ;
#1995 = CARTESIAN_POINT ( 'NONE',  ( -2.081668171172168020E-16, -5.204170427930420051E-17, 2.499999999999999112 ) ) ;
#1996 = VECTOR ( 'NONE', #2689, 1000.000000000000000 ) ;
#1997 = CARTESIAN_POINT ( 'NONE',  ( 160.4913278202574247, -11.31223276408536549, -4.005158905402271152 ) ) ;
#1998 = CARTESIAN_POINT ( 'NONE',  ( 3.175426480543072749, 5.499999999999865885, -124.6250000000000426 ) ) ;
#1999 = CARTESIAN_POINT ( 'NONE',  ( -3.175426480542816510, 5.499999999999865885, -155.8750000000000000 ) ) ;
#2000 = DIRECTION ( 'NONE',  ( -1.067522139062651904E-16, 1.000000000000000000, 0.000000000000000000 ) ) ;
#2001 = CARTESIAN_POINT ( 'NONE',  ( 139.5000000000000000, -9.165151389911669000, 8.500000000000007105 ) ) ;
#2002 = VERTEX_POINT ( 'NONE', #12956 ) ;
#2003 = CARTESIAN_POINT ( 'NONE',  ( 20.68750000000014211, 2.649519052838478661, 1.097466725451559322 ) ) ;
#2004 = EDGE_CURVE ( 'NONE', #15491, #16271, #6300, .T. ) ;
#2005 = CARTESIAN_POINT ( 'NONE',  ( -15.49999999999999289, -54.99999999999990763, -8.000000000000007105 ) ) ;
#2006 = CARTESIAN_POINT ( 'NONE',  ( 136.2336002691896510, -4.999999999999989342, 2.071067811865468400 ) ) ;
#2007 = VECTOR ( 'NONE', #20605, 1000.000000000000000 ) ;
#2008 = ORIENTED_EDGE ( 'NONE', *, *, #12210, .F. ) ;
#2009 = CARTESIAN_POINT ( 'NONE',  ( 110.4997167782375698, 1.308140751793668288, -1.308140751793640533 ) ) ;
#2010 = CARTESIAN_POINT ( 'NONE',  ( 5.196152422706629359, -2.999999999999988898, -114.7886751345948397 ) ) ;
#2011 = CARTESIAN_POINT ( 'NONE',  ( 113.8122167782374987, 0.7662911109077987781, 1.849990392679652151 ) ) ;
#2012 = CARTESIAN_POINT ( 'NONE',  ( -5.412658773652684552, -3.125000000000099920, -119.0669872981078328 ) ) ;
#2013 = CARTESIAN_POINT ( 'NONE',  ( 0.000000000000000000, -5.999999999999991118, -176.5386751345948824 ) ) ;
#2014 = ADVANCED_FACE ( 'NONE', ( #5994 ), #15569, .T. ) ;
#2015 = CYLINDRICAL_SURFACE ( 'NONE', #15261, 2.499999999999999112 ) ;
#2016 = EDGE_LOOP ( 'NONE', ( #10257, #16667, #23258, #28613 ) ) ;
#2017 = ORIENTED_EDGE ( 'NONE', *, *, #19492, .F. ) ;
#2018 = CYLINDRICAL_SURFACE ( 'NONE', #13549, 6.000000000000000888 ) ;
#2019 = CARTESIAN_POINT ( 'NONE',  ( 135.6562500000000284, -6.000000000000005329, 2.485281374238555774 ) ) ;
#2020 = AXIS2_PLACEMENT_3D ( 'NONE', #19418, #29051, #7422 ) ;
#2021 = AXIS2_PLACEMENT_3D ( 'NONE', #30364, #25131, #4096 ) ;
#2022 = CARTESIAN_POINT ( 'NONE',  ( 5.412658773652712085, -3.125000000000086153, -150.0669872981078470 ) ) ;
#2023 = AXIS2_PLACEMENT_3D ( 'NONE', #27438, #18124, #1807 ) ;
#2024 = AXIS2_PLACEMENT_3D ( 'NONE', #28082, #5188, #588 ) ;
#2025 = DIRECTION ( 'NONE',  ( -1.000000000000000000, 3.469446951953694061E-16, -0.000000000000000000 ) ) ;
#2026 = CARTESIAN_POINT ( 'NONE',  ( 22.06250000000015632, 2.000000000000212275, 0.8284271247461753029 ) ) ;
#2027 = SURFACE_SIDE_STYLE ('',( #25198 ) ) ;
#2028 = CARTESIAN_POINT ( 'NONE',  ( -5.196152422706573404, -3.000000000000002665, -137.7886751345947971 ) ) ;
#2029 = CARTESIAN_POINT ( 'NONE',  ( 5.412658773652712085, -3.125000000000086153, -71.43301270189222407 ) ) ;
#2030 = CARTESIAN_POINT ( 'NONE',  ( 134.9985123063133869, -7.386692690749734780, -8.423607852771413107 ) ) ;
#2031 = CARTESIAN_POINT ( 'NONE',  ( 142.4851497308104058, -3.535533905932725318, 3.535533905932725318 ) ) ;
#2032 = CARTESIAN_POINT ( 'NONE',  ( 0.000000000000000000, 11.00000000000001066, 3.000000000000002665 ) ) ;
#2033 = CARTESIAN_POINT ( 'NONE',  ( -3.464101615137757051, -5.999999999999979572, -161.0863248654052313 ) ) ;
#2034 = CARTESIAN_POINT ( 'NONE',  ( 5.196152422706629359, -2.999999999999988898, -146.2886751345948824 ) ) ;
#2035 = CARTESIAN_POINT ( 'NONE',  ( 12.35117513459494099, 2.500000000000084821, 1.035533905932749299 ) ) ;
#2036 = CARTESIAN_POINT ( 'NONE',  ( 6.000000000000000888, -3.330669073875464691E-16, -7.560779664488942560E-35 ) ) ;
#2037 = CARTESIAN_POINT ( 'NONE',  ( 111.3124999999998295, -1.035533905932629173, 2.500000000000325517 ) ) ;
#2038 = CARTESIAN_POINT ( 'NONE',  ( 6.000000000000000888, -3.330669073875464691E-16, -7.560779664488942560E-35 ) ) ;
#2039 =( BOUNDED_CURVE ( )  B_SPLINE_CURVE ( 2, ( #2859, #12280, #17173, #23772, #5304, #24059, #4862, #5450, #14858 ),
 .UNSPECIFIED., .F., .T. ) 
 B_SPLINE_CURVE_WITH_KNOTS ( ( 3, 2, 2, 2, 3 ),
 ( 0.4083333333333333259, 0.4092592592592592671, 0.4111111111111110938, 0.4129629629629629761, 0.4138888888888888618 ),
 .UNSPECIFIED. ) 
 CURVE ( )  GEOMETRIC_REPRESENTATION_ITEM ( )  RATIONAL_B_SPLINE_CURVE ( ( 0.9330127018922194093, 0.9330127018922194093, 1.000000000000000000, 0.8660254037844388186, 1.000000000000000000, 0.8660254037844388186, 1.000000000000000000, 0.9330127018922214077, 0.9330127018922194093 ) ) 
 REPRESENTATION_ITEM ( '' )  );
#2040 = CARTESIAN_POINT ( 'NONE',  ( 6.350852961086080661, -9.614813431917819062E-14, -120.3750000000000426 ) ) ;
#2041 = CARTESIAN_POINT ( 'NONE',  ( 108.7113248654051176, 2.000000000000057288, 0.000000000000000000 ) ) ;
#2042 = CARTESIAN_POINT ( 'NONE',  ( 2.775557561562891351E-14, 6.250000000000033751, -142.9330127018922383 ) ) ;
#2043 = PRESENTATION_STYLE_ASSIGNMENT (( #27968 ) ) ;
#2044 = ORIENTED_EDGE ( 'NONE', *, *, #19178, .T. ) ;
#2045 = COLOUR_RGB ( '', 0.09019608, 0.27058824, 0.51372549) ;
#2046 = EDGE_CURVE ( 'NONE', #29814, #10891, #21251, .T. ) ;
#2047 = CARTESIAN_POINT ( 'NONE',  ( 3.175426480543072749, 5.499999999999865885, -58.62499999999999289 ) ) ;
#2048 = DIRECTION ( 'NONE',  ( -7.147005652999508048E-36, 5.642372883946980038E-36, 1.000000000000000000 ) ) ;
#2049 = CARTESIAN_POINT ( 'NONE',  ( 0.000000000000000000, 3.114577045054885743E-15, -17.50000000000004619 ) ) ;
#2050 = EDGE_CURVE ( 'NONE', #30268, #19941, #19982, .T. ) ;
#2051 =( BOUNDED_CURVE ( )  B_SPLINE_CURVE ( 2, ( #6170, #20309, #10807, #6006, #6465, #18175, #15582, #23078, #24895 ),
 .UNSPECIFIED., .F., .T. ) 
 B_SPLINE_CURVE_WITH_KNOTS ( ( 3, 2, 2, 2, 3 ),
 ( 0.1874999999999996947, 0.1937499999999994504, 0.1999999999999991784, 0.2062499999999990452, 0.2124999999999988010 ),
 .UNSPECIFIED. ) 
 CURVE ( )  GEOMETRIC_REPRESENTATION_ITEM ( )  RATIONAL_B_SPLINE_CURVE ( ( 1.000000000000003775, 0.9238795325112830747, 1.000000000000000000, 0.9238795325112867385, 1.000000000000000000, 0.9238795325112867385, 1.000000000000000000, 0.9238795325113016155, 0.9999999999999851230 ) ) 
 REPRESENTATION_ITEM ( '' )  );
#2052 = ORIENTED_EDGE ( 'NONE', *, *, #20488, .F. ) ;
#2053 = AXIS2_PLACEMENT_3D ( 'NONE', #21662, #12021, #441 ) ;
#2054 = CARTESIAN_POINT ( 'NONE',  ( 105.6874999999997442, -1.035533905932659149, -2.499999999999724221 ) ) ;
#2055 = CARTESIAN_POINT ( 'NONE',  ( 139.1250000000000284, 0.000000000000000000, -6.000000000000005329 ) ) ;
#2056 = CARTESIAN_POINT ( 'NONE',  ( 160.0000000000000284, -12.64911064067350566, -3.000000000000002665 ) ) ;
#2057 = CARTESIAN_POINT ( 'NONE',  ( 12.50000000000012257, -1.999999999999835243, 0.000000000000000000 ) ) ;
#2058 = DIRECTION ( 'NONE',  ( -1.000000000000000000, -1.665334536937731113E-16, 1.526556658859586792E-16 ) ) ;
#2059 = CARTESIAN_POINT ( 'NONE',  ( 138.1875000000000284, 4.242640687119269671, 4.242640687119298093 ) ) ;
#2060 = CARTESIAN_POINT ( 'NONE',  ( 116.7886751345947687, -2.000000000000001776, 0.000000000000000000 ) ) ;
#2061 = VERTEX_POINT ( 'NONE', #13408 ) ;
#2062 = CIRCLE ( 'NONE', #19237, 0.5000000000000000000 ) ;
#2063 = CARTESIAN_POINT ( 'NONE',  ( -6.350852961085760029, -1.281975124255709124E-13, -136.1250000000000568 ) ) ;
#2064 = ORIENTED_EDGE ( 'NONE', *, *, #12820, .T. ) ;
#2065 = CARTESIAN_POINT ( 'NONE',  ( 13.62500000000016520, -1.414213562372923505, -1.414213562373145550 ) ) ;
#2066 = ORIENTED_EDGE ( 'NONE', *, *, #14089, .F. ) ;
#2067 = CARTESIAN_POINT ( 'NONE',  ( -3.175426480542816510, -5.500000000000057732, -63.87500000000001421 ) ) ;
#2068 = CIRCLE ( 'NONE', #29054, 1.000000000000000888 ) ;
#2069 = CARTESIAN_POINT ( 'NONE',  ( 19.99999999999998934, 1.156842902448957494E-15, -6.500000000000016875 ) ) ;
#2070 = CARTESIAN_POINT ( 'NONE',  ( -0.7071067811865482389, -9.585786437626913070, -4.000000000000004441 ) ) ;
#2071 = CARTESIAN_POINT ( 'NONE',  ( 116.0000000000000142, 0.000000000000000000, 0.000000000000000000 ) ) ;
#2072 = CARTESIAN_POINT ( 'NONE',  ( 0.000000000000000000, 0.000000000000000000, 5.000000000000004441 ) ) ;
#2073 = CARTESIAN_POINT ( 'NONE',  ( 118.8127832217620465, -1.849990392679381701, 0.7662911109078287542 ) ) ;
#2074 = DIRECTION ( 'NONE',  ( 1.000000000000000000, 0.000000000000000000, 0.000000000000000000 ) ) ;
#2075 = CARTESIAN_POINT ( 'NONE',  ( 3.175426480543072749, 5.499999999999865885, -147.1250000000000284 ) ) ;
#2076 = CARTESIAN_POINT ( 'NONE',  ( -14.99999999999999289, -25.00000000000007816, 8.000000000000007105 ) ) ;
#2077 = CARTESIAN_POINT ( 'NONE',  ( -7.216878364870328078, 0.000000000000000000, -157.5580127018922383 ) ) ;
#2078 = CARTESIAN_POINT ( 'NONE',  ( -4.763139720814407951, 2.749999999999946709, -76.25000000000004263 ) ) ;
#2079 =( LENGTH_UNIT ( ) NAMED_UNIT ( * ) SI_UNIT ( .MILLI., .METRE. ) );
#2080 = CARTESIAN_POINT ( 'NONE',  ( 3.175426480543072749, 5.499999999999865885, -76.62500000000001421 ) ) ;
#2081 = EDGE_CURVE ( 'NONE', #17791, #22266, #26800, .T. ) ;
#2082 = CARTESIAN_POINT ( 'NONE',  ( -5.999999999999963585, -1.487416814333745711E-14, -154.4136751345947971 ) ) ;
#2083 = CARTESIAN_POINT ( 'NONE',  ( 147.3898502691896510, 3.535533905932725318, -3.535533905932725318 ) ) ;
#2084 = CARTESIAN_POINT ( 'NONE',  ( -5.999999999999963585, -1.487416814333745711E-14, -88.41367513459482552 ) ) ;
#2085 = DIRECTION ( 'NONE',  ( -7.147005652999508048E-36, 5.642372883946980038E-36, 1.000000000000000000 ) ) ;
#2086 = CARTESIAN_POINT ( 'NONE',  ( 157.0312500000000568, -2.485281374238556218, -6.000000000000005329 ) ) ;
#2087 = DIRECTION ( 'NONE',  ( 1.000000000000000000, 0.000000000000000000, 0.000000000000000000 ) ) ;
#2088 = CARTESIAN_POINT ( 'NONE',  ( 3.464101615137852974, 5.999999999999884537, -55.33632486540524553 ) ) ;
#2089 = CARTESIAN_POINT ( 'NONE',  ( 119.6247167782376124, 1.849990392679523588, 0.000000000000000000 ) ) ;
#2090 = CARTESIAN_POINT ( 'NONE',  ( 6.000000000000000888, 1.743066579297358182E-13, -86.16367513459481131 ) ) ;
#2091 = ORIENTED_EDGE ( 'NONE', *, *, #27334, .F. ) ;
#2092 = CARTESIAN_POINT ( 'NONE',  ( 158.5312500000000284, -2.485281374238555774, -6.000000000000005329 ) ) ;
#2093 = FACE_OUTER_BOUND ( 'NONE', #12186, .T. ) ;
#2094 = CARTESIAN_POINT ( 'NONE',  ( 114.4377832217621318, 1.849990392679562001, 0.7662911109079489913 ) ) ;
#2095 = DIRECTION ( 'NONE',  ( 1.000000000000000000, -5.551115123125773458E-17, -1.260129944081490338E-35 ) ) ;
#2096 = VERTEX_POINT ( 'NONE', #1223 ) ;
#2097 = ORIENTED_EDGE ( 'NONE', *, *, #10762, .T. ) ;
#2098 = VERTEX_POINT ( 'NONE', #29334 ) ;
#2099 = CARTESIAN_POINT ( 'NONE',  ( -3.175426480542816510, 5.499999999999865885, -89.87500000000001421 ) ) ;
#2100 = CARTESIAN_POINT ( 'NONE',  ( 5.412658773652739619, 3.124999999999988898, -107.1830127018922383 ) ) ;
#2101 = CARTESIAN_POINT ( 'NONE',  ( -6.000000000000000888, 1.067854986875958443E-15, 7.560779664488942560E-35 ) ) ;
#2102 = CARTESIAN_POINT ( 'NONE',  ( -5.999999999999919176, 1.607695154586804565, -51.90331216351300725 ) ) ;
#2103 = ADVANCED_FACE ( 'NONE', ( #18019 ), #13264, .F. ) ;
#2104 = CARTESIAN_POINT ( 'NONE',  ( 3.175426480543072749, -5.500000000000105693, -165.6250000000000000 ) ) ;
#2105 = CARTESIAN_POINT ( 'NONE',  ( 5.380679364423385458, -9.595766763449143255, -27.68326114948592931 ) ) ;
#2106 = ORIENTED_EDGE ( 'NONE', *, *, #26530, .F. ) ;
#2107 = CARTESIAN_POINT ( 'NONE',  ( 136.0000000000000284, -9.165151389911669000, 8.000000000000007105 ) ) ;
#2108 = DIRECTION ( 'NONE',  ( -7.147005652999508048E-36, 5.642372883946980038E-36, 1.000000000000000000 ) ) ;
#2109 = VECTOR ( 'NONE', #6636, 1000.000000000000000 ) ;
#2110 = CARTESIAN_POINT ( 'NONE',  ( 3.175426480543072749, -5.500000000000105693, -174.6250000000000284 ) ) ;
#2111 = DIRECTION ( 'NONE',  ( 1.000000000000000000, 0.000000000000000000, 0.000000000000000000 ) ) ;
#2112 = CARTESIAN_POINT ( 'NONE',  ( 3.175426480543072749, -5.500000000000105693, -162.6250000000000284 ) ) ;
#2113 = CARTESIAN_POINT ( 'NONE',  ( 111.6874999999997584, -1.035533905932719101, -2.499999999999844569 ) ) ;
#2114 = CARTESIAN_POINT ( 'NONE',  ( 3.175426480543072749, 5.499999999999865885, -100.6250000000000000 ) ) ;
#2115 = DIRECTION ( 'NONE',  ( -7.147005652999508048E-36, 5.642372883946980038E-36, 1.000000000000000000 ) ) ;
#2116 = CARTESIAN_POINT ( 'NONE',  ( 145.8675748654052313, -5.500000000000012434, 2.278174593052012309 ) ) ;
#2117 = CARTESIAN_POINT ( 'NONE',  ( -3.175426480542816510, -5.500000000000057732, -99.87500000000000000 ) ) ;
#2118 = EDGE_CURVE ( 'NONE', #4691, #13609, #19686, .T. ) ;
#2119 = CARTESIAN_POINT ( 'NONE',  ( 162.3898502691896510, 3.535533905932725318, -3.535533905932725318 ) ) ;
#2120 = CARTESIAN_POINT ( 'NONE',  ( 135.0000000000000284, -7.310118669088633503, 8.297092313840531475 ) ) ;
#2121 = ORIENTED_EDGE ( 'NONE', *, *, #15780, .T. ) ;
#2122 = CARTESIAN_POINT ( 'NONE',  ( 10.87500000000010658, 5.551115123125782702E-14, 2.649519052838056332 ) ) ;
#2123 = CARTESIAN_POINT ( 'NONE',  ( 118.0624999999998010, 2.500000000000055067, 1.035533905932929599 ) ) ;
#2124 = DIRECTION ( 'NONE',  ( -7.147005652999508048E-36, 5.642372883946980038E-36, 1.000000000000000000 ) ) ;
#2125 = CARTESIAN_POINT ( 'NONE',  ( 106.5002832217622881, 1.308140751793696044, 1.308140751793640533 ) ) ;
#2126 = DIRECTION ( 'NONE',  ( 0.000000000000000000, 0.000000000000000000, 1.000000000000000000 ) ) ;
#2127 = EDGE_LOOP ( 'NONE', ( #2247, #600, #24235, #26920 ) ) ;
#2128 = CARTESIAN_POINT ( 'NONE',  ( -5.999999999999963585, 1.780251999655701777E-13, -111.8363248654052313 ) ) ;
#2129 = CARTESIAN_POINT ( 'NONE',  ( 106.9372167782374703, -0.7662911109076785410, 1.849990392679772278 ) ) ;
#2130 = EDGE_LOOP ( 'NONE', ( #2909, #12189, #895, #8535 ) ) ;
#2131 = DIRECTION ( 'NONE',  ( -0.000000000000000000, -0.000000000000000000, -1.000000000000000000 ) ) ;
#2132 =( BOUNDED_CURVE ( )  B_SPLINE_CURVE ( 2, ( #30291, #12051, #23698, #14064, #475, #24, #9252, #12205, #19097 ),
 .UNSPECIFIED., .F., .T. ) 
 B_SPLINE_CURVE_WITH_KNOTS ( ( 3, 2, 2, 2, 3 ),
 ( 0.5468750000000000000, 0.5546875000000000000, 0.5625000000000000000, 0.5703125000000000000, 0.5781250000000000000 ),
 .UNSPECIFIED. ) 
 CURVE ( )  GEOMETRIC_REPRESENTATION_ITEM ( )  RATIONAL_B_SPLINE_CURVE ( ( 1.000000000000000000, 0.9238795325112867385, 1.000000000000000000, 0.9238795325112867385, 1.000000000000000000, 0.9238795325112867385, 1.000000000000000000, 0.9238795325112867385, 1.000000000000000000 ) ) 
 REPRESENTATION_ITEM ( '' )  );
#2133 = VECTOR ( 'NONE', #5155, 1000.000000000000000 ) ;
#2134 = CIRCLE ( 'NONE', #6042, 0.5000000000000004441 ) ;
#2135 = CARTESIAN_POINT ( 'NONE',  ( 152.9062500000000000, 6.000000000000005329, -2.485281374238555774 ) ) ;
#2136 = ORIENTED_EDGE ( 'NONE', *, *, #29691, .T. ) ;
#2137 = CARTESIAN_POINT ( 'NONE',  ( 3.175426480543072749, 5.499999999999865885, -115.6250000000000142 ) ) ;
#2138 = CARTESIAN_POINT ( 'NONE',  ( 23.00000000000007461, -1.873492889144900975, -1.873492889144956486 ) ) ;
#2139 = AXIS2_PLACEMENT_3D ( 'NONE', #11477, #13471, #15473 ) ;
#2140 = CARTESIAN_POINT ( 'NONE',  ( 3.608439182435180470, 6.249999999999982236, -134.0580127018922667 ) ) ;
#2141 = ORIENTED_EDGE ( 'NONE', *, *, #8869, .T. ) ;
#2142 = DIRECTION ( 'NONE',  ( -7.147005652999508048E-36, 5.642372883946980038E-36, 1.000000000000000000 ) ) ;
#2143 = CARTESIAN_POINT ( 'NONE',  ( -3.608439182435115633, 6.249999999999965361, -165.9419872981078186 ) ) ;
#2144 = CARTESIAN_POINT ( 'NONE',  ( -5.412658773652684552, -3.125000000000099920, -180.5669872981078186 ) ) ;
#2145 = CARTESIAN_POINT ( 'NONE',  ( 160.0000000000000284, -12.58795266400503365, 3.128932333554976797 ) ) ;
#2146 = EDGE_CURVE ( 'NONE', #21560, #26328, #3356, .T. ) ;
#2147 = VERTEX_POINT ( 'NONE', #18317 ) ;
#2148 = CARTESIAN_POINT ( 'NONE',  ( 10.93750000000009948, 2.000000000000091926, -0.8284271247462354770 ) ) ;
#2149 = FACE_OUTER_BOUND ( 'NONE', #11451, .T. ) ;
#2150 = CARTESIAN_POINT ( 'NONE',  ( 5.511802646651305260, 2.338480655312030976, -180.0000000000001705 ) ) ;
#2151 = CARTESIAN_POINT ( 'NONE',  ( 112.3363248654049187, -1.414213562373173305, -1.414213562373034527 ) ) ;
#2152 = CARTESIAN_POINT ( 'NONE',  ( 111.3127832217622171, 1.849990392679501827, -0.7662911109077087390 ) ) ;
#2153 = CARTESIAN_POINT ( 'NONE',  ( -3.608439182435052128, -6.250000000000110134, -73.94198729810781856 ) ) ;
#2154 = CARTESIAN_POINT ( 'NONE',  ( 3.608439182435180470, -6.249999999999997335, -60.19198729810783277 ) ) ;
#2155 = CARTESIAN_POINT ( 'NONE',  ( -3.175426480542816510, 5.499999999999865885, -47.87500000000000000 ) ) ;
#2156 = CARTESIAN_POINT ( 'NONE',  ( -0.7481905315629638897, -9.503618936874122625, -4.126213593628788701 ) ) ;
#2157 = CARTESIAN_POINT ( 'NONE',  ( -3.464101615137757051, -5.999999999999979572, -123.5863248654051745 ) ) ;
#2158 = CARTESIAN_POINT ( 'NONE',  ( 0.000000000000000000, -5.999999999999991118, -53.53867513459481842 ) ) ;
#2159 = EDGE_CURVE ( 'NONE', #29595, #25966, #14183, .T. ) ;
#2160 = CARTESIAN_POINT ( 'NONE',  ( 4.763139720814407951, -2.749999999999988454, -119.0000000000000000 ) ) ;
#2161 = EDGE_CURVE ( 'NONE', #1738, #24742, #13565, .T. ) ;
#2162 = DIRECTION ( 'NONE',  ( -0.000000000000000000, -0.000000000000000000, -1.000000000000000000 ) ) ;
#2163 = FACE_OUTER_BOUND ( 'NONE', #5498, .T. ) ;
#2164 = VECTOR ( 'NONE', #17817, 1000.000000000000000 ) ;
#2165 = ORIENTED_EDGE ( 'NONE', *, *, #23927, .T. ) ;
#2166 = CARTESIAN_POINT ( 'NONE',  ( -5.999999999999963585, 1.780251999655701777E-13, -95.33632486540520290 ) ) ;
#2167 = ORIENTED_EDGE ( 'NONE', *, *, #21263, .T. ) ;
#2168 = CARTESIAN_POINT ( 'NONE',  ( 108.8747167782374987, 0.000000000000000000, 1.849990392679523588 ) ) ;
#2169 = CARTESIAN_POINT ( 'NONE',  ( -6.000000000000000888, 1.067854986875958443E-15, 7.560779664488942560E-35 ) ) ;
#2170 = CARTESIAN_POINT ( 'NONE',  ( 112.7497167782374845, 1.308140751793779311, 1.308140751793973600 ) ) ;
#2171 = CARTESIAN_POINT ( 'NONE',  ( 7.216878364870455975, -6.409875621278545621E-14, -109.4419872981078043 ) ) ;
#2172 = EDGE_LOOP ( 'NONE', ( #12798, #3021, #17719, #29733 ) ) ;
#2173 = ORIENTED_EDGE ( 'NONE', *, *, #8544, .T. ) ;
#2174 = CARTESIAN_POINT ( 'NONE',  ( -5.999999999999982236, -1.607695154586700426, -142.3466878364870354 ) ) ;
#2175 = CARTESIAN_POINT ( 'NONE',  ( 137.5312500000000284, -2.485281374238555774, -6.000000000000005329 ) ) ;
#2176 = CARTESIAN_POINT ( 'NONE',  ( 3.608439182435180470, 6.249999999999982236, -136.1919872981078470 ) ) ;
#2177 = DIRECTION ( 'NONE',  ( 1.000000000000000000, 0.000000000000000000, 0.000000000000000000 ) ) ;
#2178 = CARTESIAN_POINT ( 'NONE',  ( 24.50000000000010658, 5.551115123125782702E-14, -5.551115123125782702E-14 ) ) ;
#2179 = ADVANCED_FACE ( 'NONE', ( #14033 ), #25806, .T. ) ;
#2180 = AXIS2_PLACEMENT_3D ( 'NONE', #19791, #28990, #22824 ) ;
#2181 = CARTESIAN_POINT ( 'NONE',  ( 22.81250000000002132, 0.8284271247461753029, -2.000000000000091926 ) ) ;
#2182 = DIRECTION ( 'NONE',  ( -0.000000000000000000, -0.000000000000000000, -1.000000000000000000 ) ) ;
#2183 = CARTESIAN_POINT ( 'NONE',  ( -5.412658773652739619, 3.124999999999975131, -70.68301270189225249 ) ) ;
#2184 = CARTESIAN_POINT ( 'NONE',  ( 144.8288997308104058, 4.999999999999989342, -2.071067811865468400 ) ) ;
#2185 = CARTESIAN_POINT ( 'NONE',  ( 5.196152422706629359, -2.999999999999988898, -124.7113248654052597 ) ) ;
#2186 = CARTESIAN_POINT ( 'NONE',  ( 5.196152422706629359, -2.999999999999988898, -69.78867513459485394 ) ) ;
#2187 = FACE_OUTER_BOUND ( 'NONE', #8745, .T. ) ;
#2188 = CARTESIAN_POINT ( 'NONE',  ( 156.3824251345947971, 5.500000000000012434, 2.278174593052012309 ) ) ;
#2189 = CARTESIAN_POINT ( 'NONE',  ( 109.3124999999999147, -1.035533905932598975, 2.500000000000265121 ) ) ;
#2190 = CARTESIAN_POINT ( 'NONE',  ( 106.4136751345946692, 1.414213562373201061, 1.414213562373256572 ) ) ;
#2191 = EDGE_CURVE ( 'NONE', #28056, #407, #21075, .T. ) ;
#2192 = CARTESIAN_POINT ( 'NONE',  ( 6.350852961086080661, -9.614813431917819062E-14, -123.3750000000000000 ) ) ;
#2193 = CARTESIAN_POINT ( 'NONE',  ( 114.9136751345945981, -1.414213562373201061, -1.414213562373034527 ) ) ;
#2194 = CARTESIAN_POINT ( 'NONE',  ( 5.412658773652712085, -3.125000000000086153, -144.9330127018922383 ) ) ;
#2195 = CARTESIAN_POINT ( 'NONE',  ( 140.5000000000000284, 0.000000000000000000, 0.000000000000000000 ) ) ;
#2196 = CYLINDRICAL_SURFACE ( 'NONE', #4313, 6.000000000000000888 ) ;
#2197 = ORIENTED_EDGE ( 'NONE', *, *, #29081, .T. ) ;
#2198 = CARTESIAN_POINT ( 'NONE',  ( 4.763139720814407951, -2.749999999999988454, -56.00000000000004974 ) ) ;
#2199 = CARTESIAN_POINT ( 'NONE',  ( 3.464101615137852974, 5.999999999999884537, -124.3363248654051603 ) ) ;
#2200 = CARTESIAN_POINT ( 'NONE',  ( 6.000000000000000888, 1.607695154586715303, -63.01933756729744829 ) ) ;
#2201 = CARTESIAN_POINT ( 'NONE',  ( -15.49999999999999289, -25.00000000000007816, 8.000000000000007105 ) ) ;
#2202 = ORIENTED_EDGE ( 'NONE', *, *, #12275, .F. ) ;
#2203 = CARTESIAN_POINT ( 'NONE',  ( 119.8122167782374277, 0.7662911109078588412, 1.849990392679712103 ) ) ;
#2204 = CARTESIAN_POINT ( 'NONE',  ( 143.0625000000000284, -4.242640687119298093, 4.242640687119298093 ) ) ;
#2205 = AXIS2_PLACEMENT_3D ( 'NONE', #28868, #27023, #14927 ) ;
#2206 = CARTESIAN_POINT ( 'NONE',  ( 5.412658773652739619, 3.124999999999988898, -103.3169872981078470 ) ) ;
#2207 = CARTESIAN_POINT ( 'NONE',  ( 143.1636751345948255, 0.000000000000000000, 5.500000000000005329 ) ) ;
#2208 = CARTESIAN_POINT ( 'NONE',  ( 132.4687500000000284, -2.485281374238585972, 6.000000000000005329 ) ) ;
#2209 = CARTESIAN_POINT ( 'NONE',  ( 13.96132486540527218, 1.110223024625156540E-13, 2.499999999999946709 ) ) ;
#2210 = ORIENTED_EDGE ( 'NONE', *, *, #26698, .F. ) ;
#2211 = CARTESIAN_POINT ( 'NONE',  ( -6.350852961085760029, -1.281975124255709124E-13, -134.6250000000000284 ) ) ;
#2212 = CARTESIAN_POINT ( 'NONE',  ( 14.81250000000010481, 0.8284271247463557142, -2.000000000000031530 ) ) ;
#2213 = EDGE_LOOP ( 'NONE', ( #24247, #3446, #20523, #13445 ) ) ;
#2214 = VECTOR ( 'NONE', #405, 1000.000000000000000 ) ;
#2215 = CARTESIAN_POINT ( 'NONE',  ( -4.763139720814407951, -2.750000000000016431, -62.50000000000000000 ) ) ;
#2216 = EDGE_CURVE ( 'NONE', #20260, #9814, #23063, .T. ) ;
#2217 = CARTESIAN_POINT ( 'NONE',  ( 18.89882486540528106, 1.035533905932809473, 2.499999999999844569 ) ) ;
#2218 = CARTESIAN_POINT ( 'NONE',  ( -19.49999999999998224, -54.99999999999990763, -7.500000000000007105 ) ) ;
#2219 =( BOUNDED_CURVE ( )  B_SPLINE_CURVE ( 2, ( #12161, #21797, #23798, #5187, #28234, #7208, #7360, #21652, #16765 ),
 .UNSPECIFIED., .F., .T. ) 
 B_SPLINE_CURVE_WITH_KNOTS ( ( 3, 2, 2, 2, 3 ),
 ( 0.8529411764705882026, 0.8602941176470588758, 0.8676470588235294379, 0.8750000000000000000, 0.8823529411764705621 ),
 .UNSPECIFIED. ) 
 CURVE ( )  GEOMETRIC_REPRESENTATION_ITEM ( )  RATIONAL_B_SPLINE_CURVE ( ( 1.000000000000000000, 0.9238795325112867385, 1.000000000000000000, 0.9238795325112867385, 1.000000000000000000, 0.9238795325112867385, 1.000000000000000000, 0.9238795325112867385, 1.000000000000000000 ) ) 
 REPRESENTATION_ITEM ( '' )  );
#2220 = ADVANCED_FACE ( 'NONE', ( #30106 ), #27475, .F. ) ;
#2221 = CARTESIAN_POINT ( 'NONE',  ( 106.6872167782374277, 1.849990392679562001, 0.7662911109079489913 ) ) ;
#2222 = CARTESIAN_POINT ( 'NONE',  ( 112.9136751345946976, -1.414213562373090038, -1.414213562373145550 ) ) ;
#2223 = FACE_OUTER_BOUND ( 'NONE', #28038, .T. ) ;
#2224 = CARTESIAN_POINT ( 'NONE',  ( 121.0627832217620750, -0.7662911109076785410, -1.849990392679291551 ) ) ;
#2225 = TOROIDAL_SURFACE ( 'NONE', #19378, 6.000000000000000888, 5.000000000000000888 ) ;
#2226 =( BOUNDED_CURVE ( )  B_SPLINE_CURVE ( 2, ( #19868, #5871, #8175, #28611, #3261, #17140, #17593, #7579, #15292 ),
 .UNSPECIFIED., .F., .T. ) 
 B_SPLINE_CURVE_WITH_KNOTS ( ( 3, 2, 2, 2, 3 ),
 ( 0.3138888888888888840, 0.3148148148148147696, 0.3166666666666666519, 0.3185185185185185341, 0.3194444444444445308 ),
 .UNSPECIFIED. ) 
 CURVE ( )  GEOMETRIC_REPRESENTATION_ITEM ( )  RATIONAL_B_SPLINE_CURVE ( ( 0.9330127018922194093, 0.9330127018922194093, 1.000000000000000000, 0.8660254037844388186, 1.000000000000000000, 0.8660254037844388186, 1.000000000000000000, 0.9330127018922154125, 0.9330127018922194093 ) ) 
 REPRESENTATION_ITEM ( '' )  );
#2227 = CARTESIAN_POINT ( 'NONE',  ( 3.175426480543072749, -5.500000000000105693, -152.1250000000000284 ) ) ;
#2228 = CARTESIAN_POINT ( 'NONE',  ( 139.7119292434102249, -8.976731581292797912, -7.966772205599107259 ) ) ;
#2229 = CIRCLE ( 'NONE', #11578, 4.000000000000003553 ) ;
#2230 = CARTESIAN_POINT ( 'NONE',  ( -3.175426480542816510, 5.499999999999865885, -134.8750000000000000 ) ) ;
#2231 = CARTESIAN_POINT ( 'NONE',  ( -5.412658773652684552, -3.125000000000099920, -164.9330127018922667 ) ) ;
#2232 = FACE_OUTER_BOUND ( 'NONE', #13224, .T. ) ;
#2233 = CARTESIAN_POINT ( 'NONE',  ( 3.175426480543072749, -5.500000000000105693, -80.12500000000002842 ) ) ;
#2234 = CARTESIAN_POINT ( 'NONE',  ( -3.999999999999997335, 7.119033245839719993E-16, -180.0000000000000568 ) ) ;
#2235 = CARTESIAN_POINT ( 'NONE',  ( 6.350852961086080661, -9.614813431917819062E-14, -76.87500000000000000 ) ) ;
#2236 = CARTESIAN_POINT ( 'NONE',  ( -3.464101615137757051, -5.999999999999979572, -156.5863248654052313 ) ) ;
#2237 = CARTESIAN_POINT ( 'NONE',  ( 148.1398502691896510, -3.535533905932752852, 3.535533905932725318 ) ) ;
#2238 = CARTESIAN_POINT ( 'NONE',  ( -3.464101615137757051, -5.999999999999979572, -88.16367513459482552 ) ) ;
#2239 = DIRECTION ( 'NONE',  ( 0.000000000000000000, 0.000000000000000000, -1.000000000000000000 ) ) ;
#2240 = CARTESIAN_POINT ( 'NONE',  ( 160.0312500000000284, -2.485281374238556218, -6.000000000000005329 ) ) ;
#2241 = SURFACE_STYLE_FILL_AREA ( #9299 ) ;
#2242 = CARTESIAN_POINT ( 'NONE',  ( 19.93750000000015277, 2.000000000000091926, -0.8284271247462354770 ) ) ;
#2243 = VECTOR ( 'NONE', #6829, 1000.000000000000000 ) ;
#2244 = CYLINDRICAL_SURFACE ( 'NONE', #23221, 2.000000000000012879 ) ;
#2245 = CARTESIAN_POINT ( 'NONE',  ( 117.7497167782374987, 1.308140751793723799, 1.308140751793640533 ) ) ;
#2246 = FACE_OUTER_BOUND ( 'NONE', #26085, .T. ) ;
#2247 = ORIENTED_EDGE ( 'NONE', *, *, #8554, .T. ) ;
#2248 = CARTESIAN_POINT ( 'NONE',  ( 155.0625000000000284, -4.242640687119298093, 4.242640687119298093 ) ) ;
#2249 = CARTESIAN_POINT ( 'NONE',  ( 113.3752832217622881, 1.849990392679523588, 0.000000000000000000 ) ) ;
#2250 = CARTESIAN_POINT ( 'NONE',  ( 11.83632486540522954, 1.767766952966431937, 1.767766952966098870 ) ) ;
#2251 = VERTEX_POINT ( 'NONE', #8774 ) ;
#2252 = VERTEX_POINT ( 'NONE', #18770 ) ;
#2253 = VECTOR ( 'NONE', #9934, 1000.000000000000000 ) ;
#2254 = ORIENTED_EDGE ( 'NONE', *, *, #20352, .F. ) ;
#2255 = CARTESIAN_POINT ( 'NONE',  ( 4.763139720814407951, -2.749999999999988454, -87.50000000000002842 ) ) ;
#2256 = ADVANCED_FACE ( 'NONE', ( #30410 ), #27296, .T. ) ;
#2257 = CARTESIAN_POINT ( 'NONE',  ( 3.608439182435180470, -6.249999999999997335, -109.0580127018921957 ) ) ;
#2258 = ORIENTED_EDGE ( 'NONE', *, *, #21716, .F. ) ;
#2259 = DIRECTION ( 'NONE',  ( 0.000000000000000000, 0.000000000000000000, -1.000000000000000000 ) ) ;
#2260 = CARTESIAN_POINT ( 'NONE',  ( 1.000000000000000888, -14.14213562373095634, -8.500000000000007105 ) ) ;
#2261 = CARTESIAN_POINT ( 'NONE',  ( -6.000000000000007105, -1.607695154586655129, -63.76933756729744118 ) ) ;
#2262 = ORIENTED_EDGE ( 'NONE', *, *, #18472, .F. ) ;
#2263 = CARTESIAN_POINT ( 'NONE',  ( 5.196152422706629359, 3.000000000000002665, -93.53867513459479710 ) ) ;
#2264 = CARTESIAN_POINT ( 'NONE',  ( -4.763139720814407951, -2.750000000000016431, -169.0000000000000284 ) ) ;
#2265 = CARTESIAN_POINT ( 'NONE',  ( 3.175426480543072749, -5.500000000000105693, -156.6250000000000000 ) ) ;
#2266 =( BOUNDED_CURVE ( )  B_SPLINE_CURVE ( 2, ( #9093, #18490, #27657, #18637, #20628, #9403, #14055, #27808, #11274 ),
 .UNSPECIFIED., .F., .F. ) 
 B_SPLINE_CURVE_WITH_KNOTS ( ( 3, 2, 2, 2, 3 ),
 ( 0.4117647058823529216, 0.4191176470588234837, 0.4264705882352941568, 0.4338235294117647189, 0.4411764705882352811 ),
 .UNSPECIFIED. ) 
 CURVE ( )  GEOMETRIC_REPRESENTATION_ITEM ( )  RATIONAL_B_SPLINE_CURVE ( ( 1.000000000000000000, 0.9238795325112867385, 1.000000000000000000, 0.9238795325112867385, 1.000000000000000000, 0.9238795325112867385, 1.000000000000000000, 0.9238795325112867385, 1.000000000000000000 ) ) 
 REPRESENTATION_ITEM ( '' )  );
#2267 = CARTESIAN_POINT ( 'NONE',  ( 110.8749999999998721, 1.767766952966431937, -1.767766952966209892 ) ) ;
#2268 =( BOUNDED_CURVE ( )  B_SPLINE_CURVE ( 2, ( #1523, #27321, #13396, #8445, #6284, #24872, #22281, #1208, #10461 ),
 .UNSPECIFIED., .F., .F. ) 
 B_SPLINE_CURVE_WITH_KNOTS ( ( 3, 2, 2, 2, 3 ),
 ( 0.7125000000000011324, 0.7187500000000008882, 0.7250000000000006439, 0.7312500000000003997, 0.7375000000000002665 ),
 .UNSPECIFIED. ) 
 CURVE ( )  GEOMETRIC_REPRESENTATION_ITEM ( )  RATIONAL_B_SPLINE_CURVE ( ( 0.9999999999999864553, 0.9238795325113002832, 1.000000000000000000, 0.9238795325112867385, 1.000000000000000000, 0.9238795325112867385, 1.000000000000000000, 0.9238795325112840739, 1.000000000000002665 ) ) 
 REPRESENTATION_ITEM ( '' )  );
#2269 = CARTESIAN_POINT ( 'NONE',  ( -3.175426480542816066, -5.500000000000057732, -104.3750000000000142 ) ) ;
#2270 = CARTESIAN_POINT ( 'NONE',  ( -5.196152422706601826, 2.999999999999975131, -87.03867513459483973 ) ) ;
#2271 = CARTESIAN_POINT ( 'NONE',  ( -2.775557561562891351E-14, -5.500000000000115463, -101.2500000000000000 ) ) ;
#2272 =( NAMED_UNIT ( * ) SI_UNIT ( $, .STERADIAN. ) SOLID_ANGLE_UNIT ( ) );
#2273 = CARTESIAN_POINT ( 'NONE',  ( 151.4136751345948539, 0.000000000000000000, -5.500000000000005329 ) ) ;
#2274 = ORIENTED_EDGE ( 'NONE', *, *, #28192, .T. ) ;
#2275 = CIRCLE ( 'NONE', #11624, 30.00000000000000000 ) ;
#2276 = CARTESIAN_POINT ( 'NONE',  ( 111.9999999999999716, 2.500000000000002220, 0.000000000000000000 ) ) ;
#2277 = CARTESIAN_POINT ( 'NONE',  ( -3.464101615137757051, -5.999999999999979572, -161.6636751345947687 ) ) ;
#2278 =( BOUNDED_CURVE ( )  B_SPLINE_CURVE ( 2, ( #18950, #12200, #9711, #16942, #21541, #21832, #16805, #28710, #626 ),
 .UNSPECIFIED., .F., .F. ) 
 B_SPLINE_CURVE_WITH_KNOTS ( ( 3, 2, 2, 2, 3 ),
 ( 0.3281250000000000000, 0.3359375000000000000, 0.3437500000000000000, 0.3515625000000000000, 0.3593750000000000000 ),
 .UNSPECIFIED. ) 
 CURVE ( )  GEOMETRIC_REPRESENTATION_ITEM ( )  RATIONAL_B_SPLINE_CURVE ( ( 1.000000000000000000, 0.9238795325112867385, 1.000000000000000000, 0.9238795325112867385, 1.000000000000000000, 0.9238795325112867385, 1.000000000000000000, 0.9238795325112867385, 1.000000000000000000 ) ) 
 REPRESENTATION_ITEM ( '' )  );
#2279 = CARTESIAN_POINT ( 'NONE',  ( 107.1877832217621886, 0.7662911109078588412, -1.849990392679231599 ) ) ;
#2280 = CARTESIAN_POINT ( 'NONE',  ( 0.000000000000000000, 0.000000000000000000, 0.000000000000000000 ) ) ;
#2281 = ORIENTED_EDGE ( 'NONE', *, *, #27299, .T. ) ;
#2282 = CARTESIAN_POINT ( 'NONE',  ( 0.000000000000000000, 0.000000000000000000, 0.000000000000000000 ) ) ;
#2283 = CARTESIAN_POINT ( 'NONE',  ( -5.999999999999919176, 1.607695154586804565, -111.9033121635129930 ) ) ;
#2284 = CARTESIAN_POINT ( 'NONE',  ( 105.4372167782375413, 0.7662911109078888172, -1.849990392679291551 ) ) ;
#2285 = EDGE_CURVE ( 'NONE', #27416, #2984, #9679, .T. ) ;
#2286 = CARTESIAN_POINT ( 'NONE',  ( 6.000000000000000888, -3.330669073875464691E-16, -7.560779664488942560E-35 ) ) ;
#2287 = ORIENTED_EDGE ( 'NONE', *, *, #21549, .T. ) ;
#2288 = CARTESIAN_POINT ( 'NONE',  ( 153.0937500000000284, 6.000000000000005329, 2.485281374238585972 ) ) ;
#2289 = ORIENTED_EDGE ( 'NONE', *, *, #28821, .T. ) ;
#2290 = CARTESIAN_POINT ( 'NONE',  ( 0.000000000000000000, 5.499999999999991118, -115.5000000000000426 ) ) ;
#2291 = CARTESIAN_POINT ( 'NONE',  ( 20.62500000000008882, 5.551115123125782702E-14, 2.649519052838056332 ) ) ;
#2292 = EDGE_CURVE ( 'NONE', #4004, #11247, #822, .T. ) ;
#2293 = CARTESIAN_POINT ( 'NONE',  ( -3.608439182435115633, 6.249999999999965361, -130.8080127018922383 ) ) ;
#2294 = ORIENTED_EDGE ( 'NONE', *, *, #5521, .T. ) ;
#2295 = DIRECTION ( 'NONE',  ( 1.000000000000000000, -0.000000000000000000, -0.000000000000000000 ) ) ;
#2296 = CARTESIAN_POINT ( 'NONE',  ( 3.608439182435180470, -6.249999999999997335, -172.6919872981078470 ) ) ;
#2297 = CARTESIAN_POINT ( 'NONE',  ( 110.3749999999999289, -1.767766952966209892, 1.767766952966542959 ) ) ;
#2298 = VECTOR ( 'NONE', #2025, 1000.000000000000000 ) ;
#2299 =( GEOMETRIC_REPRESENTATION_CONTEXT ( 3 ) GLOBAL_UNCERTAINTY_ASSIGNED_CONTEXT ( ( #14584 ) ) GLOBAL_UNIT_ASSIGNED_CONTEXT ( ( #913, #468, #12790 ) ) REPRESENTATION_CONTEXT ( 'NONE', 'WORKASPACE' ) );
#2300 = CARTESIAN_POINT ( 'NONE',  ( 10.50000000000003730, -1.999999999999835243, 0.000000000000000000 ) ) ;
#2301 = CARTESIAN_POINT ( 'NONE',  ( -0.08259260911911876779, -15.14630466264630648, -7.836667287028713957 ) ) ;
#2302 = CARTESIAN_POINT ( 'NONE',  ( 2.846577545700131662, 4.964493094578525501, -180.0000000000000000 ) ) ;
#2303 = DIRECTION ( 'NONE',  ( 1.000000000000000000, -5.551115123125774690E-17, 0.000000000000000000 ) ) ;
#2304 = CARTESIAN_POINT ( 'NONE',  ( 112.4613248654051461, 0.000000000000000000, -2.000000000000001776 ) ) ;
#2305 = CARTESIAN_POINT ( 'NONE',  ( 108.5002832217622313, 1.308140751793696044, 1.308140751793640533 ) ) ;
#2306 = CARTESIAN_POINT ( 'NONE',  ( 5.412658773652739619, 3.124999999999988898, -176.1830127018922383 ) ) ;
#2307 = CARTESIAN_POINT ( 'NONE',  ( -0.8690767379103921941, -9.065461631044712476, -4.000000000000005329 ) ) ;
#2308 = CARTESIAN_POINT ( 'NONE',  ( -6.000000000000007105, -1.607695154586655129, -48.76933756729741987 ) ) ;
#2309 = LINE ( 'NONE', #21350, #4504 ) ;
#2310 = CARTESIAN_POINT ( 'NONE',  ( 4.763139720814407951, 2.750000000000002665, -124.7500000000000284 ) ) ;
#2311 = CARTESIAN_POINT ( 'NONE',  ( 6.000000000000000888, -1.859271017917181981E-14, -146.1636751345948255 ) ) ;
#2312 = ORIENTED_EDGE ( 'NONE', *, *, #7278, .F. ) ;
#2313 = CIRCLE ( 'NONE', #11665, 12.00000000000000178 ) ;
#2314 = CARTESIAN_POINT ( 'NONE',  ( 21.68750000000007105, 2.649519052838419153, 1.097466725451559322 ) ) ;
#2315 = LINE ( 'NONE', #28389, #563 ) ;
#2316 = CARTESIAN_POINT ( 'NONE',  ( 5.196152422706629359, 3.000000000000002665, -105.5386751345948113 ) ) ;
#2317 =( BOUNDED_CURVE ( )  B_SPLINE_CURVE ( 2, ( #20901, #19496, #28826, #7787, #585, #12753, #3178, #9820, #742 ),
 .UNSPECIFIED., .F., .T. ) 
 B_SPLINE_CURVE_WITH_KNOTS ( ( 3, 2, 2, 2, 3 ),
 ( 0.4916666666666665853, 0.4925925925925925819, 0.4944444444444444642, 0.4962962962962963465, 0.4972222222222222321 ),
 .UNSPECIFIED. ) 
 CURVE ( )  GEOMETRIC_REPRESENTATION_ITEM ( )  RATIONAL_B_SPLINE_CURVE ( ( 0.9330127018922194093, 0.9330127018922154125, 1.000000000000000000, 0.8660254037844388186, 1.000000000000000000, 0.8660254037844388186, 1.000000000000000000, 0.9330127018922194093, 0.9330127018922194093 ) ) 
 REPRESENTATION_ITEM ( '' )  );
#2318 = VERTEX_POINT ( 'NONE', #2166 ) ;
#2319 = CONICAL_SURFACE ( 'NONE', #19486, 5.500000000000000000, 0.7853981633974369547 ) ;
#2320 = CARTESIAN_POINT ( 'NONE',  ( 110.2497167782375698, -1.308140751793585022, -1.308140751793529510 ) ) ;
#2321 = CARTESIAN_POINT ( 'NONE',  ( 5.196152422706629359, 3.000000000000002665, -122.0386751345948824 ) ) ;
#2322 = EDGE_CURVE ( 'NONE', #91, #5714, #22225, .T. ) ;
#2323 = CARTESIAN_POINT ( 'NONE',  ( 2.775557561562891351E-14, -6.250000000000061284, -108.3169872981077901 ) ) ;
#2324 = SURFACE_STYLE_FILL_AREA ( #23378 ) ;
#2325 = ORIENTED_EDGE ( 'NONE', *, *, #17767, .F. ) ;
#2326 = CYLINDRICAL_SURFACE ( 'NONE', #16772, 6.000000000000000888 ) ;
#2327 = ORIENTED_EDGE ( 'NONE', *, *, #19995, .F. ) ;
#2328 = VERTEX_POINT ( 'NONE', #11249 ) ;
#2329 = CARTESIAN_POINT ( 'NONE',  ( 20.91367513459485394, -1.767766952966154381, -1.767766952966487448 ) ) ;
#2330 = CARTESIAN_POINT ( 'NONE',  ( 136.5937500000000853, 6.000000000000005329, 2.485281374238585972 ) ) ;
#2331 = EDGE_CURVE ( 'NONE', #3077, #26117, #7501, .T. ) ;
#2332 = AXIS2_PLACEMENT_3D ( 'NONE', #9625, #28338, #7457 ) ;
#2333 = CARTESIAN_POINT ( 'NONE',  ( 7.216878364870455975, -6.409875621278545621E-14, -136.4419872981077901 ) ) ;
#2334 = CARTESIAN_POINT ( 'NONE',  ( -5.999999999999963585, 8.134310703387671600E-14, -146.9136751345948255 ) ) ;
#2335 = FACE_OUTER_BOUND ( 'NONE', #11656, .T. ) ;
#2336 = CARTESIAN_POINT ( 'NONE',  ( 18.87500000000008527, 1.414213562373256572, -1.414213562373090038 ) ) ;
#2337 = CARTESIAN_POINT ( 'NONE',  ( 5.196152422706629359, -2.999999999999988898, -171.2113248654052313 ) ) ;
#2338 = CARTESIAN_POINT ( 'NONE',  ( 5.412658773652739619, 3.124999999999988898, -57.68301270189224539 ) ) ;
#2339 = DIRECTION ( 'NONE',  ( 1.000000000000000000, 0.000000000000000000, 0.000000000000000000 ) ) ;
#2340 = CARTESIAN_POINT ( 'NONE',  ( 145.9538997308103774, -2.071067811865468400, -4.999999999999989342 ) ) ;
#2341 = CARTESIAN_POINT ( 'NONE',  ( 3.464101615137757051, -5.999999999999979572, -124.8363248654051745 ) ) ;
#2342 = CARTESIAN_POINT ( 'NONE',  ( 12.85117513459490191, -2.499999999999844569, -1.035533905932809473 ) ) ;
#2343 = CARTESIAN_POINT ( 'NONE',  ( 146.9136751345948539, 0.000000000000000000, -5.500000000000005329 ) ) ;
#2344 = CARTESIAN_POINT ( 'NONE',  ( 24.65159914405371921, -2.238694682432001759, 0.7252922178121359309 ) ) ;
#2345 = CARTESIAN_POINT ( 'NONE',  ( 0.000000000000000000, 5.999999999999977796, -115.2113248654052029 ) ) ;
#2346 = CARTESIAN_POINT ( 'NONE',  ( 110.8124999999999574, 1.035533905932719101, -2.499999999999904521 ) ) ;
#2347 = CARTESIAN_POINT ( 'NONE',  ( -14.99999999999999289, -54.99999999999990763, -7.500000000000007105 ) ) ;
#2348 = CARTESIAN_POINT ( 'NONE',  ( 6.000000000000000888, 1.743066579297358182E-13, -75.08632486540521711 ) ) ;
#2349 = DIRECTION ( 'NONE',  ( 0.000000000000000000, 0.000000000000000000, -1.000000000000000000 ) ) ;
#2350 = ORIENTED_EDGE ( 'NONE', *, *, #29699, .F. ) ;
#2351 = CARTESIAN_POINT ( 'NONE',  ( 4.763139720814407951, 2.750000000000002665, -55.75000000000002132 ) ) ;
#2352 = FACE_OUTER_BOUND ( 'NONE', #19071, .T. ) ;
#2353 = CARTESIAN_POINT ( 'NONE',  ( 5.196152422706629359, 3.000000000000002665, -121.4613248654052313 ) ) ;
#2354 = EDGE_LOOP ( 'NONE', ( #6191, #27822, #18065, #3558 ) ) ;
#2355 = CARTESIAN_POINT ( 'NONE',  ( 106.3749999999999574, -1.767766952966320915, 1.767766952966431937 ) ) ;
#2356 = CARTESIAN_POINT ( 'NONE',  ( 137.3437500000000284, -6.000000000000005329, -2.485281374238556218 ) ) ;
#2357 = EDGE_CURVE ( 'NONE', #28820, #11352, #22041, .T. ) ;
#2358 = CARTESIAN_POINT ( 'NONE',  ( -5.412658773652684552, -3.125000000000099920, -104.0669872981078186 ) ) ;
#2359 = VECTOR ( 'NONE', #6119, 1000.000000000000000 ) ;
#2360 = CARTESIAN_POINT ( 'NONE',  ( 160.8601497308104058, -3.535533905932725318, -3.535533905932725318 ) ) ;
#2361 = CARTESIAN_POINT ( 'NONE',  ( 119.1249999999999432, 1.767766952966348670, 1.767766952966431937 ) ) ;
#2362 = EDGE_LOOP ( 'NONE', ( #28718, #15523, #16232, #7841 ) ) ;
#2363 =( BOUNDED_CURVE ( )  B_SPLINE_CURVE ( 2, ( #10930, #20279, #29469, #24718, #15225, #15066, #3351, #19809, #15549 ),
 .UNSPECIFIED., .F., .F. ) 
 B_SPLINE_CURVE_WITH_KNOTS ( ( 3, 2, 2, 2, 3 ),
 ( 0.008333333333333414750, 0.009259259259259300379, 0.01111111111111107164, 0.01296296296296295392, 0.01388888888888883955 ),
 .UNSPECIFIED. ) 
 CURVE ( )  GEOMETRIC_REPRESENTATION_ITEM ( )  RATIONAL_B_SPLINE_CURVE ( ( 0.9330127018922194093, 0.9330127018922234061, 1.000000000000000000, 0.8660254037844388186, 1.000000000000000000, 0.8660254037844388186, 1.000000000000000000, 0.9330127018922234061, 0.9330127018922194093 ) ) 
 REPRESENTATION_ITEM ( '' )  );
#2364 = ADVANCED_FACE ( 'NONE', ( #24098 ), #598, .F. ) ;
#2365 = CARTESIAN_POINT ( 'NONE',  ( -4.763139720814407951, -2.750000000000016431, -139.0000000000000000 ) ) ;
#2366 = EDGE_CURVE ( 'NONE', #8039, #28361, #299, .T. ) ;
#2367 = VERTEX_POINT ( 'NONE', #21807 ) ;
#2368 = CARTESIAN_POINT ( 'NONE',  ( 115.2738248654048760, -1.999999999999911626, -0.8284271247460553989 ) ) ;
#2369 = CARTESIAN_POINT ( 'NONE',  ( 4.763139720814407951, 2.750000000000002665, -67.75000000000002842 ) ) ;
#2370 = CARTESIAN_POINT ( 'NONE',  ( 109.1636751345948113, 1.414213562373145550, -1.414213562372812483 ) ) ;
#2371 = CARTESIAN_POINT ( 'NONE',  ( -3.608439182435052128, -6.250000000000110134, -80.80801270189226670 ) ) ;
#2372 = CARTESIAN_POINT ( 'NONE',  ( 152.4449251345948824, -5.500000000000012434, 2.278174593052012309 ) ) ;
#2373 = CARTESIAN_POINT ( 'NONE',  ( 106.2497167782374845, -1.308140751793585022, -1.308140751793640533 ) ) ;
#2374 = DIRECTION ( 'NONE',  ( 1.000000000000000000, -5.551115123125773458E-17, -1.260129944081490338E-35 ) ) ;
#2375 = CARTESIAN_POINT ( 'NONE',  ( 119.8127832217621460, -1.849990392679381701, 0.7662911109078287542 ) ) ;
#2376 = CARTESIAN_POINT ( 'NONE',  ( -3.175426480542816066, -5.500000000000057732, -146.3750000000000284 ) ) ;
#2377 = CARTESIAN_POINT ( 'NONE',  ( 139.6502262449442924, -9.198487685513971002, -7.982156388384278323 ) ) ;
#2378 = CARTESIAN_POINT ( 'NONE',  ( 0.000000000000000000, 5.499999999999991118, -133.5000000000000000 ) ) ;
#2379 = CARTESIAN_POINT ( 'NONE',  ( -3.608439182435115633, 6.249999999999965361, -162.3080127018922667 ) ) ;
#2380 = CARTESIAN_POINT ( 'NONE',  ( 3.464101615137757051, -5.999999999999979572, -148.8363248654051176 ) ) ;
#2381 = CARTESIAN_POINT ( 'NONE',  ( 3.175426480543072749, 5.499999999999865885, -75.12500000000000000 ) ) ;
#2382 = CARTESIAN_POINT ( 'NONE',  ( -6.350852961085760029, -1.281975124255709124E-13, -62.62500000000001421 ) ) ;
#2383 = FILL_AREA_STYLE ('',( #9602 ) ) ;
#2384 = CARTESIAN_POINT ( 'NONE',  ( 158.7187500000000284, 2.485281374238556218, -6.000000000000005329 ) ) ;
#2385 = EDGE_CURVE ( 'NONE', #22196, #4423, #17948, .T. ) ;
#2386 = CARTESIAN_POINT ( 'NONE',  ( 119.9553615878004393, -1.023503819640848800, -1.804923305105176290 ) ) ;
#2387 = CARTESIAN_POINT ( 'NONE',  ( 118.3747167782375129, 0.000000000000000000, -1.849990392679301543 ) ) ;
#2388 = CARTESIAN_POINT ( 'NONE',  ( -3.464101615137757051, -5.999999999999979572, -98.08632486540524553 ) ) ;
#2389 = EDGE_CURVE ( 'NONE', #15666, #14341, #19074, .T. ) ;
#2390 = VERTEX_POINT ( 'NONE', #9534 ) ;
#2391 = CARTESIAN_POINT ( 'NONE',  ( 147.8437500000000284, -6.000000000000005329, -2.485281374238555774 ) ) ;
#2392 = CARTESIAN_POINT ( 'NONE',  ( 115.9377832217620323, -1.849990392679441875, -0.7662911109075283278 ) ) ;
#2393 = DIRECTION ( 'NONE',  ( -7.147005652999508048E-36, 5.642372883946980038E-36, 1.000000000000000000 ) ) ;
#2394 = EDGE_LOOP ( 'NONE', ( #2136, #24211, #9224, #3417 ) ) ;
#2395 = ORIENTED_EDGE ( 'NONE', *, *, #10585, .T. ) ;
#2396 =( BOUNDED_CURVE ( )  B_SPLINE_CURVE ( 2, ( #17510, #29751, #3936, #6257, #20394, #8728, #27433, #13223, #6402 ),
 .UNSPECIFIED., .F., .T. ) 
 B_SPLINE_CURVE_WITH_KNOTS ( ( 3, 2, 2, 2, 3 ),
 ( 0.7361111111111110494, 0.7370370370370370461, 0.7388888888888889284, 0.7407407407407406996, 0.7416666666666666963 ),
 .UNSPECIFIED. ) 
 CURVE ( )  GEOMETRIC_REPRESENTATION_ITEM ( )  RATIONAL_B_SPLINE_CURVE ( ( 0.9330127018922194093, 0.9330127018922154125, 1.000000000000000000, 0.8660254037844388186, 1.000000000000000000, 0.8660254037844388186, 1.000000000000000000, 0.9330127018922154125, 0.9330127018922194093 ) ) 
 REPRESENTATION_ITEM ( '' )  );
#2397 = PRESENTATION_LAYER_ASSIGNMENT (  '', '', ( #2465 ) ) ;
#2398 = CARTESIAN_POINT ( 'NONE',  ( 22.37500000000011724, -1.414213562372979016, 1.414213562372979016 ) ) ;
#2399 = VERTEX_POINT ( 'NONE', #14897 ) ;
#2400 = CARTESIAN_POINT ( 'NONE',  ( -3.175426480542816510, 5.499999999999865885, -88.37500000000000000 ) ) ;
#2401 = CARTESIAN_POINT ( 'NONE',  ( 7.216878364870455975, -6.409875621278545621E-14, -107.3080127018922525 ) ) ;
#2402 =( BOUNDED_CURVE ( )  B_SPLINE_CURVE ( 2, ( #16114, #4073, #22834, #1775, #11179, #29879, #8858, #13806, #18241 ),
 .UNSPECIFIED., .F., .T. ) 
 B_SPLINE_CURVE_WITH_KNOTS ( ( 3, 2, 2, 2, 3 ),
 ( 0.8194444444444444198, 0.8203703703703704164, 0.8222222222222221877, 0.8240740740740740700, 0.8249999999999999556 ),
 .UNSPECIFIED. ) 
 CURVE ( )  GEOMETRIC_REPRESENTATION_ITEM ( )  RATIONAL_B_SPLINE_CURVE ( ( 0.9330127018922194093, 0.9330127018922154125, 1.000000000000000000, 0.8660254037844388186, 1.000000000000000000, 0.8660254037844388186, 1.000000000000000000, 0.9330127018922234061, 0.9330127018922194093 ) ) 
 REPRESENTATION_ITEM ( '' )  );
#2403 = ORIENTED_EDGE ( 'NONE', *, *, #30161, .F. ) ;
#2404 = FILL_AREA_STYLE ('',( #7155 ) ) ;
#2405 = CARTESIAN_POINT ( 'NONE',  ( 158.3288997308104058, 4.999999999999989342, -2.071067811865468400 ) ) ;
#2406 = CARTESIAN_POINT ( 'NONE',  ( -6.350852961085760029, -1.281975124255709124E-13, -163.1249999999999716 ) ) ;
#2407 = CARTESIAN_POINT ( 'NONE',  ( -5.412658773652739619, 3.124999999999975131, -48.18301270189223828 ) ) ;
#2408 = CARTESIAN_POINT ( 'NONE',  ( 135.8344003793675085, -8.798545317550690470, 8.160000018076395634 ) ) ;
#2409 = SURFACE_SIDE_STYLE ('',( #14424 ) ) ;
#2410 = CARTESIAN_POINT ( 'NONE',  ( -3.175426480542816066, -5.500000000000057732, -170.3750000000000853 ) ) ;
#2411 = CARTESIAN_POINT ( 'NONE',  ( 24.99999999999999289, 1.110223024625156540E-13, -2.220446049250313081E-13 ) ) ;
#2412 = CARTESIAN_POINT ( 'NONE',  ( 4.763139720814407951, 2.750000000000002665, -151.7500000000000568 ) ) ;
#2413 = CARTESIAN_POINT ( 'NONE',  ( 112.8124999999998579, 1.035533905932779275, -2.499999999999904521 ) ) ;
#2414 = CARTESIAN_POINT ( 'NONE',  ( 0.000000000000000000, 5.499999999999991118, -103.5000000000000426 ) ) ;
#2415 = CARTESIAN_POINT ( 'NONE',  ( 21.39882486540530238, -1.035533905932749299, -2.499999999999964473 ) ) ;
#2416 = CARTESIAN_POINT ( 'NONE',  ( 115.4761751345947118, 0.8284271247462654530, 2.000000000000151879 ) ) ;
#2417 = CARTESIAN_POINT ( 'NONE',  ( 4.763139720814407951, 2.750000000000002665, -87.25000000000005684 ) ) ;
#2418 = CARTESIAN_POINT ( 'NONE',  ( 13.58632486540531303, 1.767766952966487448, -1.767766952966320915 ) ) ;
#2419 = SURFACE_STYLE_FILL_AREA ( #9335 ) ;
#2420 = CARTESIAN_POINT ( 'NONE',  ( 134.9999999999997158, -6.982120021892662898, 8.500000000000007105 ) ) ;
#2421 = ORIENTED_EDGE ( 'NONE', *, *, #20777, .F. ) ;
#2422 = CARTESIAN_POINT ( 'NONE',  ( 10.06250000000008349, -2.649519052838178457, 1.097466725451499370 ) ) ;
#2423 = CARTESIAN_POINT ( 'NONE',  ( 113.6874999999998437, -1.035533905932749299, -2.499999999999904521 ) ) ;
#2424 = DIRECTION ( 'NONE',  ( -7.147005652999508048E-36, 5.642372883946980038E-36, 1.000000000000000000 ) ) ;
#2425 = ADVANCED_FACE ( 'NONE', ( #18922 ), #28244, .F. ) ;
#2426 = CARTESIAN_POINT ( 'NONE',  ( 10.00000000000009059, 2.022462396512465510, -0.1718975768220544764 ) ) ;
#2427 = CARTESIAN_POINT ( 'NONE',  ( 157.9761751345948255, 3.889087296526011706, 3.889087296526011706 ) ) ;
#2428 = EDGE_CURVE ( 'NONE', #1801, #26144, #4898, .T. ) ;
#2429 = VERTEX_POINT ( 'NONE', #2603 ) ;
#2430 = CARTESIAN_POINT ( 'NONE',  ( 9.937500000000083489, 2.000000000000151879, -0.8284271247463557142 ) ) ;
#2431 = CARTESIAN_POINT ( 'NONE',  ( 0.000000000000000000, 0.000000000000000000, 0.000000000000000000 ) ) ;
#2432 = CARTESIAN_POINT ( 'NONE',  ( 106.1247167782374987, -1.849990392679412565, 2.220446049250313081E-13 ) ) ;
#2433 = ORIENTED_EDGE ( 'NONE', *, *, #19492, .T. ) ;
#2434 = LINE ( 'NONE', #2286, #3664 ) ;
#2435 = ORIENTED_EDGE ( 'NONE', *, *, #25003, .T. ) ;
#2436 = CARTESIAN_POINT ( 'NONE',  ( 152.2500000000000284, -6.000000000000005329, 0.000000000000000000 ) ) ;
#2437 = ORIENTED_EDGE ( 'NONE', *, *, #24781, .F. ) ;
#2438 = CARTESIAN_POINT ( 'NONE',  ( 3.175426480543072749, -5.500000000000105693, -110.1249999999999858 ) ) ;
#2439 = AXIS2_PLACEMENT_3D ( 'NONE', #3544, #5700, #21859 ) ;
#2440 = CARTESIAN_POINT ( 'NONE',  ( 23.68750000000013500, -1.097466725451379244, 2.649519052838358757 ) ) ;
#2441 = CARTESIAN_POINT ( 'NONE',  ( -7.216878364870328078, 0.000000000000000000, -129.0580127018922383 ) ) ;
#2442 = ORIENTED_EDGE ( 'NONE', *, *, #8844, .T. ) ;
#2443 = CARTESIAN_POINT ( 'NONE',  ( 158.9925748654052313, 2.278174593051907504, 5.500000000000116351 ) ) ;
#2444 = CIRCLE ( 'NONE', #1436, 14.49999999999999822 ) ;
#2445 = CARTESIAN_POINT ( 'NONE',  ( 7.216878364870455975, -6.409875621278545621E-14, -167.9419872981078186 ) ) ;
#2446 = CARTESIAN_POINT ( 'NONE',  ( 109.4374999999998721, -2.499999999999934719, 1.035533905932929599 ) ) ;
#2447 = CARTESIAN_POINT ( 'NONE',  ( 133.2976497308104058, 0.000000000000000000, 5.000000000000004441 ) ) ;
#2448 = ORIENTED_EDGE ( 'NONE', *, *, #9048, .F. ) ;
#2449 = CARTESIAN_POINT ( 'NONE',  ( 3.106370373199874635, 4.832402510089593761, -180.0000000000001421 ) ) ;
#2450 = DIRECTION ( 'NONE',  ( 0.000000000000000000, 0.000000000000000000, 1.000000000000000000 ) ) ;
#2451 = CARTESIAN_POINT ( 'NONE',  ( 6.350852961086080661, -9.614813431917819062E-14, -178.8750000000000284 ) ) ;
#2452 = CARTESIAN_POINT ( 'NONE',  ( 106.3752832217622171, 1.849990392679523588, 0.000000000000000000 ) ) ;
#2453 = CARTESIAN_POINT ( 'NONE',  ( -3.608439182435115633, 6.249999999999965361, -177.3080127018922383 ) ) ;
#2454 = DIRECTION ( 'NONE',  ( 5.551115123125785167E-17, -1.000000000000000000, -8.881784197001256268E-16 ) ) ;
#2455 = CARTESIAN_POINT ( 'NONE',  ( -4.763139720814407951, -2.750000000000016431, -111.9999999999999858 ) ) ;
#2456 = CARTESIAN_POINT ( 'NONE',  ( 134.9999999999992895, -6.982120021884474781, -8.500000000000007105 ) ) ;
#2457 = CARTESIAN_POINT ( 'NONE',  ( 6.000000000000052403, 1.607695154586625819, -154.5193375672974128 ) ) ;
#2458 = VERTEX_POINT ( 'NONE', #21359 ) ;
#2459 = CARTESIAN_POINT ( 'NONE',  ( 21.93750000000006395, -1.097466725451379244, 2.649519052838178457 ) ) ;
#2460 = CARTESIAN_POINT ( 'NONE',  ( 0.000000000000000000, -15.50000000000001421, -5.656854249492387687 ) ) ;
#2461 = DIRECTION ( 'NONE',  ( 0.000000000000000000, 0.000000000000000000, 1.000000000000000000 ) ) ;
#2462 = CARTESIAN_POINT ( 'NONE',  ( 135.0000000000000000, 1.949781249179272091, -5.142796231657337458 ) ) ;
#2463 = EDGE_CURVE ( 'NONE', #15491, #21222, #25343, .T. ) ;
#2464 = ORIENTED_EDGE ( 'NONE', *, *, #16603, .F. ) ;
#2465 = STYLED_ITEM ( 'NONE', ( #15153 ), #14219 ) ;
#2466 = CARTESIAN_POINT ( 'NONE',  ( 118.3363248654051176, -1.414213562373201061, -1.414213562373034527 ) ) ;
#2467 = CARTESIAN_POINT ( 'NONE',  ( -5.196152422706573404, -3.000000000000002665, -176.7886751345948539 ) ) ;
#2468 = CARTESIAN_POINT ( 'NONE',  ( -5.196152422706573404, -3.000000000000002665, -95.78867513459482552 ) ) ;
#2469 = LINE ( 'NONE', #25959, #11347 ) ;
#2470 = ORIENTED_EDGE ( 'NONE', *, *, #27046, .F. ) ;
#2471 = ORIENTED_EDGE ( 'NONE', *, *, #25251, .T. ) ;
#2472 = LINE ( 'NONE', #4467, #26239 ) ;
#2473 = CARTESIAN_POINT ( 'NONE',  ( 134.9062500000000284, 6.000000000000005329, -2.485281374238555774 ) ) ;
#2474 = CARTESIAN_POINT ( 'NONE',  ( 2.775557561562891351E-14, 6.250000000000033751, -137.5669872981077901 ) ) ;
#2475 = CARTESIAN_POINT ( 'NONE',  ( 10.06250000000005151, -1.097466725451499370, -2.649519052838419153 ) ) ;
#2476 = CARTESIAN_POINT ( 'NONE',  ( 19.93750000000015277, 2.000000000000091926, -0.8284271247462354770 ) ) ;
#2477 = CARTESIAN_POINT ( 'NONE',  ( -5.196152422706573404, -3.000000000000002665, -171.7113248654052029 ) ) ;
#2478 = CARTESIAN_POINT ( 'NONE',  ( 117.2738248654048476, -1.999999999999911626, -0.8284271247460553989 ) ) ;
#2479 = CARTESIAN_POINT ( 'NONE',  ( 143.3288997308104911, 4.999999999999989342, -2.071067811865468400 ) ) ;
#2480 = CARTESIAN_POINT ( 'NONE',  ( -5.999999999999963585, 8.134310703387671600E-14, -125.3363248654052171 ) ) ;
#2481 = LINE ( 'NONE', #16056, #19708 ) ;
#2482 = CARTESIAN_POINT ( 'NONE',  ( 0.000000000000000000, -5.999999999999991118, -139.9613248654052313 ) ) ;
#2483 = ADVANCED_FACE ( 'NONE', ( #14608 ), #23961, .T. ) ;
#2484 = CARTESIAN_POINT ( 'NONE',  ( 24.58754953339359162, -1.405346041411892788, 1.966652551842076990 ) ) ;
#2485 = SURFACE_SIDE_STYLE ('',( #2629 ) ) ;
#2486 = CARTESIAN_POINT ( 'NONE',  ( 109.8749999999998437, 1.767766952966320915, -1.767766952966209892 ) ) ;
#2487 =( BOUNDED_CURVE ( )  B_SPLINE_CURVE ( 2, ( #15246, #5831, #13114, #3837, #29493, #13265, #24578, #7839, #12957 ),
 .UNSPECIFIED., .F., .T. ) 
 B_SPLINE_CURVE_WITH_KNOTS ( ( 3, 2, 2, 2, 3 ),
 ( 0.3750000000000000000, 0.3759259259259258856, 0.3777777777777777679, 0.3796296296296296502, 0.3805555555555555358 ),
 .UNSPECIFIED. ) 
 CURVE ( )  GEOMETRIC_REPRESENTATION_ITEM ( )  RATIONAL_B_SPLINE_CURVE ( ( 0.9330127018922194093, 0.9330127018922194093, 1.000000000000000000, 0.8660254037844388186, 1.000000000000000000, 0.8660254037844388186, 1.000000000000000000, 0.9330127018922234061, 0.9330127018922194093 ) ) 
 REPRESENTATION_ITEM ( '' )  );
#2488 = CARTESIAN_POINT ( 'NONE',  ( 3.464101615137852974, 5.999999999999884537, -112.9136751345948255 ) ) ;
#2489 = ORIENTED_EDGE ( 'NONE', *, *, #4182, .T. ) ;
#2490 = CARTESIAN_POINT ( 'NONE',  ( 0.000000000000000000, 5.499999999999991118, -52.49999999999999289 ) ) ;
#2491 = CARTESIAN_POINT ( 'NONE',  ( -5.999999999999971578, 1.607695154586715303, -87.90331216351300725 ) ) ;
#2492 = ORIENTED_EDGE ( 'NONE', *, *, #12853, .T. ) ;
#2493 = CARTESIAN_POINT ( 'NONE',  ( 120.0622167782374419, -1.849990392679472073, 0.7662911109078888172 ) ) ;
#2494 = CARTESIAN_POINT ( 'NONE',  ( 140.1562500000000568, -6.000000000000005329, 2.485281374238556218 ) ) ;
#2495 = CARTESIAN_POINT ( 'NONE',  ( 2.775557561562891351E-14, 6.250000000000033751, -100.0669872981078186 ) ) ;
#2496 = AXIS2_PLACEMENT_3D ( 'NONE', #19663, #3507, #12624 ) ;
#2497 = CARTESIAN_POINT ( 'NONE',  ( 6.000000000000000888, 1.743066579297358182E-13, -77.16367513459483973 ) ) ;
#2498 = CARTESIAN_POINT ( 'NONE',  ( 159.8288997308104058, 4.999999999999989342, -2.071067811865468400 ) ) ;
#2499 = CARTESIAN_POINT ( 'NONE',  ( -3.175426480542816510, 5.499999999999865885, -139.3750000000000568 ) ) ;
#2500 = ORIENTED_EDGE ( 'NONE', *, *, #21909, .T. ) ;
#2501 = EDGE_LOOP ( 'NONE', ( #3910, #381, #12584, #28216 ) ) ;
#2502 = CARTESIAN_POINT ( 'NONE',  ( 5.196152422706629359, 3.000000000000002665, -163.4613248654052029 ) ) ;
#2503 = CARTESIAN_POINT ( 'NONE',  ( 4.763139720814407951, -2.749999999999988454, -69.50000000000000000 ) ) ;
#2504 = CARTESIAN_POINT ( 'NONE',  ( 140.3511751345948255, -3.889087296526011706, 3.889087296526011706 ) ) ;
#2505 = CARTESIAN_POINT ( 'NONE',  ( -5.999999999999919176, 1.607695154586804565, -65.98066243270258724 ) ) ;
#2506 = CARTESIAN_POINT ( 'NONE',  ( -7.216878364870328078, 0.000000000000000000, -84.05801270189220986 ) ) ;
#2507 = DIRECTION ( 'NONE',  ( 1.000000000000000000, 0.000000000000000000, 0.000000000000000000 ) ) ;
#2508 = ADVANCED_FACE ( 'NONE', ( #15948 ), #8848, .F. ) ;
#2509 = CARTESIAN_POINT ( 'NONE',  ( 107.3122167782375413, -0.7662911109077087390, -1.849990392679291551 ) ) ;
#2510 = CARTESIAN_POINT ( 'NONE',  ( 5.999999999999949374, -1.607695154586841868, -175.6533121635130215 ) ) ;
#2511 = VECTOR ( 'NONE', #12672, 1000.000000000000114 ) ;
#2512 = CARTESIAN_POINT ( 'NONE',  ( 118.3127832217620750, 1.849990392679532247, -0.7662911109075883909 ) ) ;
#2513 = CARTESIAN_POINT ( 'NONE',  ( -3.175426480542816066, 5.499999999999865885, -149.8750000000000000 ) ) ;
#2514 = CARTESIAN_POINT ( 'NONE',  ( 139.6067523651853151, -8.946933530859819683, 7.999999965039304328 ) ) ;
#2515 = VECTOR ( 'NONE', #21031, 1000.000000000000000 ) ;
#2516 = CARTESIAN_POINT ( 'NONE',  ( -5.412658773652739619, 3.124999999999975131, -162.1830127018922951 ) ) ;
#2517 = CARTESIAN_POINT ( 'NONE',  ( -5.999999999999962697, 3.323446944526963260E-14, -149.3363248654052313 ) ) ;
#2518 = VECTOR ( 'NONE', #14237, 1000.000000000000000 ) ;
#2519 = CARTESIAN_POINT ( 'NONE',  ( -3.175426480542816066, 5.499999999999865885, -82.37500000000002842 ) ) ;
#2520 = CARTESIAN_POINT ( 'NONE',  ( 3.464101615137852974, 5.999999999999884537, -85.91367513459482552 ) ) ;
#2521 = EDGE_CURVE ( 'NONE', #14299, #26206, #15206, .T. ) ;
#2522 = CARTESIAN_POINT ( 'NONE',  ( -2.775557561562891351E-14, -5.500000000000115463, -63.75000000000002842 ) ) ;
#2523 = EDGE_CURVE ( 'NONE', #15395, #9180, #5366, .T. ) ;
#2524 = CARTESIAN_POINT ( 'NONE',  ( 143.0773502691896510, 5.000000000000004441, 0.000000000000000000 ) ) ;
#2525 = CARTESIAN_POINT ( 'NONE',  ( 108.7886751345946834, -1.999999999999946265, 1.110223024625156540E-13 ) ) ;
#2526 = CARTESIAN_POINT ( 'NONE',  ( 155.2500000000000284, -6.000000000000005329, 0.000000000000000000 ) ) ;
#2527 = FACE_OUTER_BOUND ( 'NONE', #25917, .T. ) ;
#2528 = CARTESIAN_POINT ( 'NONE',  ( 16.62500000000013856, -1.414213562372867994, -1.414213562373145550 ) ) ;
#2529 = SURFACE_SIDE_STYLE ('',( #23741 ) ) ;
#2530 =( BOUNDED_CURVE ( )  B_SPLINE_CURVE ( 2, ( #10038, #19415, #14235, #28146, #14088, #25860, #4806, #2505, #15109 ),
 .UNSPECIFIED., .F., .F. ) 
 B_SPLINE_CURVE_WITH_KNOTS ( ( 3, 2, 2, 2, 3 ),
 ( 0.8527777777777778567, 0.8537037037037037424, 0.8555555555555555136, 0.8574074074074073959, 0.8583333333333332815 ),
 .UNSPECIFIED. ) 
 CURVE ( )  GEOMETRIC_REPRESENTATION_ITEM ( )  RATIONAL_B_SPLINE_CURVE ( ( 0.9330127018922194093, 0.9330127018922234061, 1.000000000000000000, 0.8660254037844388186, 1.000000000000000000, 0.8660254037844388186, 1.000000000000000000, 0.9330127018922234061, 0.9330127018922194093 ) ) 
 REPRESENTATION_ITEM ( '' )  );
#2531 = CYLINDRICAL_SURFACE ( 'NONE', #14609, 2.000000000000012879 ) ;
#2532 = CARTESIAN_POINT ( 'NONE',  ( 118.4372167782374135, 0.7662911109079189043, -1.849990392679291551 ) ) ;
#2533 = CARTESIAN_POINT ( 'NONE',  ( 6.000000000000000888, -3.330669073875464691E-16, -7.560779664488942560E-35 ) ) ;
#2534 = VERTEX_POINT ( 'NONE', #18231 ) ;
#2535 = CARTESIAN_POINT ( 'NONE',  ( 147.3750000000000284, 0.000000000000000000, 6.000000000000005329 ) ) ;
#2536 = CARTESIAN_POINT ( 'NONE',  ( 6.000000000000000888, -1.859271017917181981E-14, -141.0863248654052029 ) ) ;
#2537 = B_SPLINE_CURVE_WITH_KNOTS ( 'NONE', 3,
 ( #11703, #25638, #284, #14312, #27770, #2302, #2449, #6590, #6747, #16463, #21200, #18302, #7052, #16318, #2150, #16013 ),
 .UNSPECIFIED., .F., .F.,
 ( 4, 2, 2, 2, 2, 2, 2, 4 ),
 ( 0.000000000000000000, 0.001747794382755240477, 0.002621691574132859522, 0.003495588765510479218, 0.004369485956888098481, 0.005243383148265719045, 0.006117280339643340475, 0.006991177531020960172 ),
 .UNSPECIFIED. ) ;
#2538 = CARTESIAN_POINT ( 'NONE',  ( 114.0627832217621602, -0.7662911109077388261, -1.849990392679231599 ) ) ;
#2539 = CARTESIAN_POINT ( 'NONE',  ( 6.350852961086080661, -9.614813431917819062E-14, -153.3750000000000000 ) ) ;
#2540 = DIRECTION ( 'NONE',  ( -7.147005652999508048E-36, 5.642372883946980038E-36, 1.000000000000000000 ) ) ;
#2541 = ORIENTED_EDGE ( 'NONE', *, *, #18260, .T. ) ;
#2542 = CARTESIAN_POINT ( 'NONE',  ( 20.75000000000012790, 1.665334536937734811E-13, -2.000000000000001776 ) ) ;
#2543 = ORIENTED_EDGE ( 'NONE', *, *, #603, .T. ) ;
#2544 = CARTESIAN_POINT ( 'NONE',  ( 4.763139720814407951, -2.749999999999988454, -89.00000000000002842 ) ) ;
#2545 = CARTESIAN_POINT ( 'NONE',  ( 7.216878364870455975, -6.409875621278545621E-14, -101.3080127018922525 ) ) ;
#2546 = CARTESIAN_POINT ( 'NONE',  ( 155.0476497308104342, 0.000000000000000000, -5.000000000000004441 ) ) ;
#2547 = EDGE_CURVE ( 'NONE', #226, #17900, #28486, .T. ) ;
#2548 = CARTESIAN_POINT ( 'NONE',  ( 0.000000000000000000, 0.000000000000000000, 0.000000000000000000 ) ) ;
#2549 = CARTESIAN_POINT ( 'NONE',  ( -3.464101615137757051, -5.999999999999979572, -68.08632486540523132 ) ) ;
#2550 = CARTESIAN_POINT ( 'NONE',  ( 4.763139720814407951, 2.750000000000002665, -171.2500000000000000 ) ) ;
#2551 = CARTESIAN_POINT ( 'NONE',  ( 5.196152422706629359, -2.999999999999988898, -80.28867513459481131 ) ) ;
#2552 = CARTESIAN_POINT ( 'NONE',  ( -6.350852961085760029, -1.281975124255709124E-13, -154.1250000000000568 ) ) ;
#2553 = CARTESIAN_POINT ( 'NONE',  ( 113.3749999999999289, -1.767766952966293159, 1.767766952966431937 ) ) ;
#2554 = CARTESIAN_POINT ( 'NONE',  ( 4.763139720814407951, -2.749999999999988454, -99.50000000000002842 ) ) ;
#2555 = CARTESIAN_POINT ( 'NONE',  ( 21.02382486540522066, -1.035533905932749299, 2.499999999999964473 ) ) ;
#2556 = CARTESIAN_POINT ( 'NONE',  ( 0.000000000000000000, 5.999999999999977796, -59.71132486540520290 ) ) ;
#2557 = EDGE_CURVE ( 'NONE', #84, #21073, #12765, .T. ) ;
#2559 = CARTESIAN_POINT ( 'NONE',  ( -3.175426480542816510, 5.499999999999865885, -91.37500000000001421 ) ) ;
#2558 = CARTESIAN_POINT ( 'NONE',  ( -4.763139720814407951, -2.750000000000016431, -155.5000000000000284 ) ) ;
#2560 = CARTESIAN_POINT ( 'NONE',  ( 156.1086002691896510, -2.071067811865468400, -4.999999999999989342 ) ) ;
#2561 = CARTESIAN_POINT ( 'NONE',  ( 107.1011751345945981, 0.8284271247463257382, -1.999999999999791278 ) ) ;
#2562 = EDGE_LOOP ( 'NONE', ( #24072, #13087, #479, #12346 ) ) ;
#2563 = CARTESIAN_POINT ( 'NONE',  ( 23.87500000000009237, 1.414213562373256572, -1.414213562373145550 ) ) ;
#2564 = UNCERTAINTY_MEASURE_WITH_UNIT (LENGTH_MEASURE( 1.000000000000000082E-05 ), #28419, 'distance_accuracy_value', 'NONE');
#2565 = CARTESIAN_POINT ( 'NONE',  ( 111.4374999999997300, -2.499999999999904521, 1.035533905932869425 ) ) ;
#2566 = CARTESIAN_POINT ( 'NONE',  ( 5.196152422706629359, -2.999999999999988898, -66.21132486540520290 ) ) ;
#2567 = CARTESIAN_POINT ( 'NONE',  ( 105.0002832217622029, -1.308140751793612777, -1.308140751793640533 ) ) ;
#2568 = CARTESIAN_POINT ( 'NONE',  ( 161.0872520967092782, 0.6323632113212951378, 5.560287570051549721 ) ) ;
#2569 =( BOUNDED_CURVE ( )  B_SPLINE_CURVE ( 2, ( #3185, #5194, #12609, #2894, #5640, #12461, #21803, #10283, #19358 ),
 .UNSPECIFIED., .F., .T. ) 
 B_SPLINE_CURVE_WITH_KNOTS ( ( 3, 2, 2, 2, 3 ),
 ( 0.5374999999999999778, 0.5437499999999997335, 0.5499999999999996003, 0.5562499999999993561, 0.5624999999999991118 ),
 .UNSPECIFIED. ) 
 CURVE ( )  GEOMETRIC_REPRESENTATION_ITEM ( )  RATIONAL_B_SPLINE_CURVE ( ( 1.000000000000000000, 0.9238795325112867385, 1.000000000000000000, 0.9238795325112867385, 1.000000000000000000, 0.9238795325112867385, 1.000000000000000000, 0.9238795325112975076, 0.9999999999999892308 ) ) 
 REPRESENTATION_ITEM ( '' )  );
#2570 = ORIENTED_EDGE ( 'NONE', *, *, #8367, .T. ) ;
#2571 = DIRECTION ( 'NONE',  ( 1.000000000000000000, 0.000000000000000000, 0.000000000000000000 ) ) ;
#2572 = LINE ( 'NONE', #21325, #18737 ) ;
#2573 = ORIENTED_EDGE ( 'NONE', *, *, #23425, .F. ) ;
#2574 = CARTESIAN_POINT ( 'NONE',  ( -3.464101615137757051, -5.999999999999979572, -141.5863248654052029 ) ) ;
#2575 = CARTESIAN_POINT ( 'NONE',  ( 149.2500000000000284, -6.000000000000005329, 0.000000000000000000 ) ) ;
#2576 = ORIENTED_EDGE ( 'NONE', *, *, #30089, .T. ) ;
#2577 = CARTESIAN_POINT ( 'NONE',  ( 4.763139720814407951, -2.749999999999988454, -117.5000000000000426 ) ) ;
#2578 = CARTESIAN_POINT ( 'NONE',  ( 21.43750000000003908, 2.649519052838419153, 1.097466725451499370 ) ) ;
#2579 = CARTESIAN_POINT ( 'NONE',  ( 7.216878364870455975, -6.409875621278545621E-14, -120.8080127018921957 ) ) ;
#2580 = EDGE_LOOP ( 'NONE', ( #15203, #2944 ) ) ;
#2581 = CARTESIAN_POINT ( 'NONE',  ( 0.000000000000000000, 0.000000000000000000, 0.000000000000000000 ) ) ;
#2582 = CARTESIAN_POINT ( 'NONE',  ( 3.608439182435180470, 6.249999999999982236, -169.1919872981078186 ) ) ;
#2583 = CARTESIAN_POINT ( 'NONE',  ( 106.8124999999997016, 1.035533905932749299, -2.499999999999784173 ) ) ;
#2584 =( NAMED_UNIT ( * ) PLANE_ANGLE_UNIT ( ) SI_UNIT ( $, .RADIAN. ) );
#2585 = EDGE_CURVE ( 'NONE', #5920, #379, #5587, .T. ) ;
#2586 = ORIENTED_EDGE ( 'NONE', *, *, #28158, .F. ) ;
#2587 = CARTESIAN_POINT ( 'NONE',  ( -0.08237010255012430782, -15.17881940287713149, -7.764910707444049542 ) ) ;
#2588 = EDGE_CURVE ( 'NONE', #14973, #8441, #16177, .T. ) ;
#2589 = DIRECTION ( 'NONE',  ( -7.147005652999508048E-36, 5.642372883946980038E-36, 1.000000000000000000 ) ) ;
#2590 = LINE ( 'NONE', #28666, #30003 ) ;
#2591 = CARTESIAN_POINT ( 'NONE',  ( -4.763139720814407951, 2.749999999999946709, -176.7500000000000284 ) ) ;
#2592 = CARTESIAN_POINT ( 'NONE',  ( 109.0002832217621034, -1.308140751793640533, -1.308140751793640533 ) ) ;
#2593 = CARTESIAN_POINT ( 'NONE',  ( -7.216878364870328078, 0.000000000000000000, -174.0580127018922667 ) ) ;
#2594 = CYLINDRICAL_SURFACE ( 'NONE', #849, 6.000000000000005329 ) ;
#2595 = CARTESIAN_POINT ( 'NONE',  ( 160.7876825596520405, -11.44597140916194711, -3.606058123595494713 ) ) ;
#2596 = UNCERTAINTY_MEASURE_WITH_UNIT (LENGTH_MEASURE( 1.000000000000000082E-05 ), #27730, 'distance_accuracy_value', 'NONE');
#2597 = CARTESIAN_POINT ( 'NONE',  ( -2.775557561562891351E-14, -5.500000000000115463, -113.2500000000000142 ) ) ;
#2598 = CARTESIAN_POINT ( 'NONE',  ( 5.630955349231442142, 2.071796769705314123, -180.0000000000000568 ) ) ;
#2599 = CARTESIAN_POINT ( 'NONE',  ( 6.000000000000000888, 1.607695154586715303, -101.0966878364870638 ) ) ;
#2600 = VERTEX_POINT ( 'NONE', #889 ) ;
#2601 = CARTESIAN_POINT ( 'NONE',  ( 19.31250000000007105, -1.097466725451379244, -2.649519052838538613 ) ) ;
#2602 = CARTESIAN_POINT ( 'NONE',  ( -0.02761656219841567006, -15.32973869486954754, 6.905504754228253717 ) ) ;
#2603 = CARTESIAN_POINT ( 'NONE',  ( -39.99999999999998579, -59.99999999999980105, -3.000000000000002665 ) ) ;
#2604 = CARTESIAN_POINT ( 'NONE',  ( -6.000000000000023093, 1.607695154586625819, -131.4033121635129930 ) ) ;
#2605 = AXIS2_PLACEMENT_3D ( 'NONE', #117, #9498, #28203 ) ;
#2606 = ORIENTED_EDGE ( 'NONE', *, *, #11414, .F. ) ;
#2607 =( NAMED_UNIT ( * ) PLANE_ANGLE_UNIT ( ) SI_UNIT ( $, .RADIAN. ) );
#2608 = CARTESIAN_POINT ( 'NONE',  ( 6.000000000000000888, -3.330669073875464691E-16, -7.560779664488942560E-35 ) ) ;
#2609 = CARTESIAN_POINT ( 'NONE',  ( 5.196152422706629359, 3.000000000000002665, -108.5386751345948113 ) ) ;
#2610 = CARTESIAN_POINT ( 'NONE',  ( 159.0000000000000284, -12.00000000000001066, -4.000000000000003553 ) ) ;
#2611 =( GEOMETRIC_REPRESENTATION_CONTEXT ( 3 ) GLOBAL_UNCERTAINTY_ASSIGNED_CONTEXT ( ( #26005 ) ) GLOBAL_UNIT_ASSIGNED_CONTEXT ( ( #6212, #8836, #11315 ) ) REPRESENTATION_CONTEXT ( 'NONE', 'WORKASPACE' ) );
#2612 = CARTESIAN_POINT ( 'NONE',  ( -5.999999999999963585, -1.487416814333745711E-14, -80.33632486540523132 ) ) ;
#2613 = ORIENTED_EDGE ( 'NONE', *, *, #2686, .T. ) ;
#2614 = ORIENTED_EDGE ( 'NONE', *, *, #3229, .F. ) ;
#2615 = CARTESIAN_POINT ( 'NONE',  ( 136.7812500000000284, 2.485281374238585972, 6.000000000000005329 ) ) ;
#2616 =( BOUNDED_SURFACE ( )  B_SPLINE_SURFACE ( 2, 3, ( 
 ( #15747, #13432, #6483, #25204 ),
 ( #4167, #13591, #8159, #26892 ),
 ( #15273, #24601, #3551, #10658 ) ),
 .UNSPECIFIED., .F., .F., .F. ) 
 B_SPLINE_SURFACE_WITH_KNOTS ( ( 3, 3 ),
 ( 4, 4 ),
 ( 0.000000000000000000, 1.000000000000000000 ),
 ( 0.000000000000000000, 1.000000000000000000 ),
 .UNSPECIFIED. ) 
 GEOMETRIC_REPRESENTATION_ITEM ( )  RATIONAL_B_SPLINE_SURFACE ( (
 ( 1.000000000000000000, 0.3333333333333334259, 0.3333333333333334259, 1.000000000000000000),
 ( 1.000000000000000000, 0.3333333333333334259, 0.3333333333333334259, 1.000000000000000000),
 ( 1.000000000000000000, 0.3333333333333334259, 0.3333333333333334259, 1.000000000000000000) ) ) 
 REPRESENTATION_ITEM ( '' )  SURFACE ( )  );
#2617 = ORIENTED_EDGE ( 'NONE', *, *, #1141, .F. ) ;
#2618 = CARTESIAN_POINT ( 'NONE',  ( -3.608439182435052128, -6.250000000000110134, -141.4419872981078186 ) ) ;
#2619 = CARTESIAN_POINT ( 'NONE',  ( 6.000000000000001776, 5.345404176511898156E-15, -174.6636751345948539 ) ) ;
#2620 = CARTESIAN_POINT ( 'NONE',  ( 10.56250000000013678, 1.097466725451679892, 2.649519052838419153 ) ) ;
#2621 = CARTESIAN_POINT ( 'NONE',  ( 0.000000000000000000, 5.999999999999977796, -129.2886751345947971 ) ) ;
#2622 = CARTESIAN_POINT ( 'NONE',  ( 18.43749999999999289, -1.999999999999971800, 0.8284271247462354770 ) ) ;
#2623 = PLANE ( 'NONE',  #11819 ) ;
#2624 = CARTESIAN_POINT ( 'NONE',  ( 117.2113248654051034, -1.999999999999890754, 3.330669073875469621E-13 ) ) ;
#2625 = ADVANCED_FACE ( 'NONE', ( #10439 ), #13499, .T. ) ;
#2626 = CARTESIAN_POINT ( 'NONE',  ( 136.2976497308104058, 0.000000000000000000, 5.000000000000004441 ) ) ;
#2627 = CARTESIAN_POINT ( 'NONE',  ( 137.8988248654052313, 3.889087296526011706, 3.889087296526011706 ) ) ;
#2628 = CARTESIAN_POINT ( 'NONE',  ( 5.999999999999949374, 1.607695154586804565, -60.59668783648704249 ) ) ;
#2629 = SURFACE_STYLE_FILL_AREA ( #23545 ) ;
#2630 = CARTESIAN_POINT ( 'NONE',  ( 107.2499999999999147, 0.000000000000000000, 2.499999999999946709 ) ) ;
#2631 = CYLINDRICAL_SURFACE ( 'NONE', #9262, 2.499999999999999112 ) ;
#2632 = CARTESIAN_POINT ( 'NONE',  ( 5.999999999999988454, 1.607695154586737729, -149.0966878364870922 ) ) ;
#2633 = EDGE_LOOP ( 'NONE', ( #12030, #17756, #23523, #12329 ) ) ;
#2634 = CARTESIAN_POINT ( 'NONE',  ( -5.196152422706573404, -3.000000000000002665, -107.2113248654052455 ) ) ;
#2635 = CARTESIAN_POINT ( 'NONE',  ( 6.000000000000000888, 7.762456499804234384E-14, -132.6636751345948539 ) ) ;
#2636 = CARTESIAN_POINT ( 'NONE',  ( -5.999999999999919176, 1.607695154586804565, -120.9033121635129930 ) ) ;
#2637 = CARTESIAN_POINT ( 'NONE',  ( 135.5000000000000284, -54.99999999999993605, -8.000000000000007105 ) ) ;
#2638 = EDGE_LOOP ( 'NONE', ( #17869, #15243, #6960, #18367 ) ) ;
#2639 = CARTESIAN_POINT ( 'NONE',  ( 116.5622167782374135, 1.849990392679562001, -0.7662911109077087390 ) ) ;
#2640 = CARTESIAN_POINT ( 'NONE',  ( 139.6875000000000284, 4.242640687119269671, 4.242640687119298093 ) ) ;
#2641 = CARTESIAN_POINT ( 'NONE',  ( 12.25000000000006573, 5.551115123125782702E-14, 1.999999999999946265 ) ) ;
#2642 = CARTESIAN_POINT ( 'NONE',  ( -5.412658773652739619, 3.124999999999975131, -101.3169872981078470 ) ) ;
#2643 = CARTESIAN_POINT ( 'NONE',  ( 0.000000000000000000, 5.999999999999977796, -176.7113248654052029 ) ) ;
#2644 = CARTESIAN_POINT ( 'NONE',  ( 159.2663997308104058, -4.999999999999989342, -2.071067811865468400 ) ) ;
#2645 = CARTESIAN_POINT ( 'NONE',  ( 118.4999999999998437, -2.499999999999919176, 0.000000000000000000 ) ) ;
#2646 = EDGE_CURVE ( 'NONE', #16115, #1732, #29138, .T. ) ;
#2647 = CARTESIAN_POINT ( 'NONE',  ( -6.350852961085760029, -1.281975124255709124E-13, -131.6250000000000284 ) ) ;
#2648 = VERTEX_POINT ( 'NONE', #22256 ) ;
#2649 = CARTESIAN_POINT ( 'NONE',  ( 6.350852961086080661, -9.614813431917819062E-14, -57.37500000000004974 ) ) ;
#2650 = CARTESIAN_POINT ( 'NONE',  ( 6.000000000000000888, -1.859271017917181981E-14, -116.1636751345948255 ) ) ;
#2651 = DIRECTION ( 'NONE',  ( -7.147005652999508048E-36, 5.642372883946980038E-36, 1.000000000000000000 ) ) ;
#2652 = CARTESIAN_POINT ( 'NONE',  ( 5.412658773652739619, 3.124999999999988898, -86.18301270189220986 ) ) ;
#2653 =( BOUNDED_CURVE ( )  B_SPLINE_CURVE ( 2, ( #2904, #7662, #2468, #11884, #9384, #28547, #28252, #4905, #4762 ),
 .UNSPECIFIED., .F., .T. ) 
 B_SPLINE_CURVE_WITH_KNOTS ( ( 3, 2, 2, 2, 3 ),
 ( 0.6361111111111110716, 0.6370370370370370683, 0.6388888888888888395, 0.6407407407407407218, 0.6416666666666667185 ),
 .UNSPECIFIED. ) 
 CURVE ( )  GEOMETRIC_REPRESENTATION_ITEM ( )  RATIONAL_B_SPLINE_CURVE ( ( 0.9330127018922194093, 0.9330127018922154125, 1.000000000000000000, 0.8660254037844388186, 1.000000000000000000, 0.8660254037844388186, 1.000000000000000000, 0.9330127018922154125, 0.9330127018922194093 ) ) 
 REPRESENTATION_ITEM ( '' )  );
#2654 = PRODUCT_DEFINITION_CONTEXT ( 'detailed design', #14794, 'design' ) ;
#2655 = EDGE_CURVE ( 'NONE', #16741, #19034, #20264, .T. ) ;
#2656 = CARTESIAN_POINT ( 'NONE',  ( -3.464101615137725076, 5.999999999999979572, -139.6636751345947971 ) ) ;
#2657 = CARTESIAN_POINT ( 'NONE',  ( 140.8531441848274710, -11.85314418482602150, -4.000138456839524181 ) ) ;
#2658 = CARTESIAN_POINT ( 'NONE',  ( 117.1252832217621460, -5.551115123125782702E-14, -1.849990392679523588 ) ) ;
#2659 = CARTESIAN_POINT ( 'NONE',  ( 3.175426480543072749, 5.499999999999865885, -144.1250000000000000 ) ) ;
#2660 = CARTESIAN_POINT ( 'NONE',  ( 140.1568281512133183, -9.009466367372738205, 7.926673930277594593 ) ) ;
#2661 = CARTESIAN_POINT ( 'NONE',  ( -5.412658773652684552, -3.125000000000099920, -154.4330127018922383 ) ) ;
#2662 = CARTESIAN_POINT ( 'NONE',  ( 0.000000000000000000, 5.999999999999977796, -116.7113248654052597 ) ) ;
#2663 = CARTESIAN_POINT ( 'NONE',  ( 105.6488248654050182, 2.000000000000061728, -0.8284271247459350507 ) ) ;
#2664 = CARTESIAN_POINT ( 'NONE',  ( 3.175426480543072749, 5.499999999999865885, -69.12500000000002842 ) ) ;
#2665 = DIRECTION ( 'NONE',  ( -1.000000000000000000, -1.665334536937736783E-16, -2.220446049250315546E-16 ) ) ;
#2666 = CARTESIAN_POINT ( 'NONE',  ( 3.175426480543072749, 5.499999999999865885, -61.62500000000000000 ) ) ;
#2667 = CARTESIAN_POINT ( 'NONE',  ( 0.000000000000000000, -5.999999999999991118, -148.0386751345948539 ) ) ;
#2668 = CARTESIAN_POINT ( 'NONE',  ( 158.8125000000000284, 4.242640687119298093, -4.242640687119298093 ) ) ;
#2669 = DIRECTION ( 'NONE',  ( 1.000000000000000000, 1.387778780781444413E-14, 0.000000000000000000 ) ) ;
#2670 =( LENGTH_UNIT ( ) NAMED_UNIT ( * ) SI_UNIT ( .MILLI., .METRE. ) );
#2671 = DIRECTION ( 'NONE',  ( 5.551115123125785167E-17, -1.000000000000000000, -8.881784197001256268E-16 ) ) ;
#2672 = CARTESIAN_POINT ( 'NONE',  ( 115.1247167782376692, -1.849990392679523588, 0.000000000000000000 ) ) ;
#2673 = DIRECTION ( 'NONE',  ( 1.000000000000000000, -0.000000000000000000, -0.000000000000000000 ) ) ;
#2674 = EDGE_LOOP ( 'NONE', ( #27119, #10105, #17595, #4465 ) ) ;
#2675 = CARTESIAN_POINT ( 'NONE',  ( 149.3437500000000284, -6.000000000000005329, -2.485281374238555774 ) ) ;
#2676 = CARTESIAN_POINT ( 'NONE',  ( 113.9377832217623450, -1.849990392679441875, -0.7662911109076485650 ) ) ;
#2677 = EDGE_CURVE ( 'NONE', #17448, #20178, #12832, .T. ) ;
#2678 = FACE_OUTER_BOUND ( 'NONE', #30205, .T. ) ;
#2679 = CARTESIAN_POINT ( 'NONE',  ( 5.999999999999949374, 1.607695154586804565, -64.51933756729744118 ) ) ;
#2680 = CARTESIAN_POINT ( 'NONE',  ( 3.175426480543072749, -5.500000000000105693, -179.1250000000000568 ) ) ;
#2681 = CARTESIAN_POINT ( 'NONE',  ( 21.43750000000007105, -1.999999999999911626, 0.8284271247461753029 ) ) ;
#2682 = VERTEX_POINT ( 'NONE', #19250 ) ;
#2683 = ORIENTED_EDGE ( 'NONE', *, *, #3065, .T. ) ;
#2684 = CARTESIAN_POINT ( 'NONE',  ( -6.350852961085760029, -1.281975124255709124E-13, -86.62499999999998579 ) ) ;
#2685 = TOROIDAL_SURFACE ( 'NONE', #10053, 9.999999999999998224, 1.000000000000000000 ) ;
#2686 = EDGE_CURVE ( 'NONE', #29417, #10444, #19362, .T. ) ;
#2687 = ORIENTED_EDGE ( 'NONE', *, *, #11577, .T. ) ;
#2688 = AXIS2_PLACEMENT_3D ( 'NONE', #28731, #7703, #26438 ) ;
#2689 = DIRECTION ( 'NONE',  ( -1.000000000000000000, -1.665334536937736783E-16, -2.220446049250315546E-16 ) ) ;
#2690 = CARTESIAN_POINT ( 'NONE',  ( 154.5788997308104058, -4.999999999999989342, 2.071067811865468400 ) ) ;
#2691 = CARTESIAN_POINT ( 'NONE',  ( -5.999999999999963585, 1.780251999655701777E-13, -94.41367513459482552 ) ) ;
#2692 = CARTESIAN_POINT ( 'NONE',  ( 4.509628467067703816, -10.03401783428612326, -21.03762154299058906 ) ) ;
#2693 = CARTESIAN_POINT ( 'NONE',  ( 5.196152422706629359, -2.999999999999988898, -67.71132486540520290 ) ) ;
#2694 = CARTESIAN_POINT ( 'NONE',  ( -4.763139720814407951, -2.750000000000016431, -166.0000000000000284 ) ) ;
#2695 = CARTESIAN_POINT ( 'NONE',  ( 6.000000000000000888, -1.607695154586752384, -80.23066243270258724 ) ) ;
#2696 = CARTESIAN_POINT ( 'NONE',  ( -6.350852961085760029, -1.281975124255709124E-13, -152.6250000000000568 ) ) ;
#2697 = CARTESIAN_POINT ( 'NONE',  ( 112.0624999999997868, 2.500000000000055067, 1.035533905932989551 ) ) ;
#2698 = CARTESIAN_POINT ( 'NONE',  ( -3.464101615137757051, -5.999999999999979572, -52.16367513459485394 ) ) ;
#2699 =( BOUNDED_CURVE ( )  B_SPLINE_CURVE ( 2, ( #8153, #26887, #20000, #5400, #29352, #22310, #24759, #24594, #24440 ),
 .UNSPECIFIED., .F., .F. ) 
 B_SPLINE_CURVE_WITH_KNOTS ( ( 3, 2, 2, 2, 3 ),
 ( 0.9027777777777777901, 0.9037037037037036757, 0.9055555555555555580, 0.9074074074074074403, 0.9083333333333333259 ),
 .UNSPECIFIED. ) 
 CURVE ( )  GEOMETRIC_REPRESENTATION_ITEM ( )  RATIONAL_B_SPLINE_CURVE ( ( 0.9330127018922194093, 0.9330127018922194093, 1.000000000000000000, 0.8660254037844388186, 1.000000000000000000, 0.8660254037844388186, 1.000000000000000000, 0.9330127018922194093, 0.9330127018922194093 ) ) 
 REPRESENTATION_ITEM ( '' )  );
#2700 = DIRECTION ( 'NONE',  ( 1.000000000000000000, -3.469446951953694061E-16, 0.000000000000000000 ) ) ;
#2701 = CARTESIAN_POINT ( 'NONE',  ( -2.775557561562891351E-14, -5.500000000000115463, -89.25000000000005684 ) ) ;
#2702 = CARTESIAN_POINT ( 'NONE',  ( 155.4523502691896510, 0.000000000000000000, 5.000000000000004441 ) ) ;
#2703 = CARTESIAN_POINT ( 'NONE',  ( 0.000000000000000000, 0.000000000000000000, 0.000000000000000000 ) ) ;
#2704 = CARTESIAN_POINT ( 'NONE',  ( 112.4374999999998010, -2.499999999999934719, 1.035533905932989551 ) ) ;
#2705 = DIRECTION ( 'NONE',  ( 0.000000000000000000, -2.081668171172248016E-17, 1.000000000000000000 ) ) ;
#2706 = DIRECTION ( 'NONE',  ( 0.000000000000000000, 0.000000000000000000, -1.000000000000000000 ) ) ;
#2707 = CARTESIAN_POINT ( 'NONE',  ( 6.000000000000000888, 7.762456499804235646E-14, -129.6636751345948255 ) ) ;
#2708 = VERTEX_POINT ( 'NONE', #12651 ) ;
#2709 = AXIS2_PLACEMENT_3D ( 'NONE', #5352, #16637, #5203 ) ;
#2710 = CARTESIAN_POINT ( 'NONE',  ( 6.000000000000000888, 7.762456499804235646E-14, -117.6636751345948255 ) ) ;
#2711 = CARTESIAN_POINT ( 'NONE',  ( 106.2497167782374845, -1.308140751793585022, -1.308140751793640533 ) ) ;
#2712 = EDGE_CURVE ( 'NONE', #11265, #20245, #26137, .T. ) ;
#2713 = ORIENTED_EDGE ( 'NONE', *, *, #3850, .T. ) ;
#2714 = CARTESIAN_POINT ( 'NONE',  ( 145.7812500000000284, 2.485281374238585972, 6.000000000000005329 ) ) ;
#2715 = EDGE_LOOP ( 'NONE', ( #27835, #18399, #6894, #21530 ) ) ;
#2716 = COLOUR_RGB ( '', 0.31764706, 0.68627451, 0.89019608) ;
#2717 = CARTESIAN_POINT ( 'NONE',  ( -3.175426480542816510, -5.500000000000057732, -110.3750000000000426 ) ) ;
#2718 = CARTESIAN_POINT ( 'NONE',  ( 17.06250000000004263, -1.097466725451439196, -2.649519052838358757 ) ) ;
#2719 = EDGE_CURVE ( 'NONE', #1935, #7475, #10031, .T. ) ;
#2720 = CARTESIAN_POINT ( 'NONE',  ( -3.608439182435052128, -6.250000000000110134, -125.8080127018922383 ) ) ;
#2721 = VERTEX_POINT ( 'NONE', #12353 ) ;
#2722 = DIRECTION ( 'NONE',  ( -1.000000000000000000, 0.000000000000000000, 0.000000000000000000 ) ) ;
#2723 = CARTESIAN_POINT ( 'NONE',  ( 2.775557561562891351E-14, 6.250000000000033751, -158.5669872981078186 ) ) ;
#2724 = CARTESIAN_POINT ( 'NONE',  ( 109.9374999999996874, 2.500000000000114575, -1.035533905932448873 ) ) ;
#2725 = CARTESIAN_POINT ( 'NONE',  ( 133.9538997308104342, -2.071067811865468400, -4.999999999999989342 ) ) ;
#2726 = ORIENTED_EDGE ( 'NONE', *, *, #46, .T. ) ;
#2727 = CARTESIAN_POINT ( 'NONE',  ( 2.799076333356274106E-14, 11.00000000000000000, -19.00000000000002132 ) ) ;
#2728 = CARTESIAN_POINT ( 'NONE',  ( -4.763139720814407951, 2.749999999999946709, -181.2500000000000284 ) ) ;
#2729 = CARTESIAN_POINT ( 'NONE',  ( 108.7502832217622881, -1.308140751793640533, 1.308140751793862577 ) ) ;
#2730 = DIRECTION ( 'NONE',  ( 0.000000000000000000, 0.000000000000000000, -1.000000000000000000 ) ) ;
#2731 = CARTESIAN_POINT ( 'NONE',  ( 3.608439182435180470, 6.249999999999982236, -176.0580127018922667 ) ) ;
#2732 = DIRECTION ( 'NONE',  ( 1.000000000000000000, -5.551115123125773458E-17, -1.260129944081490338E-35 ) ) ;
#2733 = CARTESIAN_POINT ( 'NONE',  ( -5.999999999999962697, 3.323446944526963891E-14, -161.9136751345948539 ) ) ;
#2734 = CARTESIAN_POINT ( 'NONE',  ( -2.775557561562891351E-14, -5.500000000000115463, -123.7500000000000284 ) ) ;
#2735 = CARTESIAN_POINT ( 'NONE',  ( 0.000000000000000000, 0.000000000000000000, 0.000000000000000000 ) ) ;
#2736 =( BOUNDED_CURVE ( )  B_SPLINE_CURVE ( 2, ( #9079, #27345, #27485, #1552, #11573, #1855, #30266, #27793, #8937 ),
 .UNSPECIFIED., .F., .T. ) 
 B_SPLINE_CURVE_WITH_KNOTS ( ( 3, 2, 2, 2, 3 ),
 ( 0.5882352941176470784, 0.5955882352941176405, 0.6029411764705882026, 0.6102941176470588758, 0.6176470588235294379 ),
 .UNSPECIFIED. ) 
 CURVE ( )  GEOMETRIC_REPRESENTATION_ITEM ( )  RATIONAL_B_SPLINE_CURVE ( ( 1.000000000000000000, 0.9238795325112867385, 1.000000000000000000, 0.9238795325112867385, 1.000000000000000000, 0.9238795325112867385, 1.000000000000000000, 0.9238795325112867385, 1.000000000000000000 ) ) 
 REPRESENTATION_ITEM ( '' )  );
#2737 = CARTESIAN_POINT ( 'NONE',  ( -3.175426480542816510, 5.499999999999865885, -113.8750000000000000 ) ) ;
#2738 = FACE_OUTER_BOUND ( 'NONE', #22689, .T. ) ;
#2739 = CARTESIAN_POINT ( 'NONE',  ( 5.196152422706629359, 3.000000000000002665, -101.0386751345948539 ) ) ;
#2740 = EDGE_LOOP ( 'NONE', ( #7967, #11336, #27256, #978 ) ) ;
#2741 = CARTESIAN_POINT ( 'NONE',  ( 18.43749999999990408, 1.097466725451619718, -2.649519052838358757 ) ) ;
#2742 = VECTOR ( 'NONE', #12531, 1000.000000000000000 ) ;
#2743 = DIRECTION ( 'NONE',  ( 1.000000000000000000, 0.000000000000000000, 0.000000000000000000 ) ) ;
#2744 = CARTESIAN_POINT ( 'NONE',  ( -3.464101615137725076, 5.999999999999979572, -168.1636751345948255 ) ) ;
#2745 = CARTESIAN_POINT ( 'NONE',  ( 18.39882486540522422, -1.035533905932689347, -2.500000000000084821 ) ) ;
#2746 = PLANE ( 'NONE',  #8076 ) ;
#2747 =( BOUNDED_CURVE ( )  B_SPLINE_CURVE ( 2, ( #12411, #24190, #2843, #12264, #539, #28779, #21606, #21755, #696 ),
 .UNSPECIFIED., .F., .T. ) 
 B_SPLINE_CURVE_WITH_KNOTS ( ( 3, 2, 2, 2, 3 ),
 ( 0.5294117647058823595, 0.5367647058823529216, 0.5441176470588234837, 0.5514705882352941568, 0.5588235294117647189 ),
 .UNSPECIFIED. ) 
 CURVE ( )  GEOMETRIC_REPRESENTATION_ITEM ( )  RATIONAL_B_SPLINE_CURVE ( ( 1.000000000000000000, 0.9238795325112867385, 1.000000000000000000, 0.9238795325112867385, 1.000000000000000000, 0.9238795325112867385, 1.000000000000000000, 0.9238795325112867385, 1.000000000000000000 ) ) 
 REPRESENTATION_ITEM ( '' )  );
#2748 = CARTESIAN_POINT ( 'NONE',  ( 6.000000000000000888, 1.743066579297358182E-13, -87.08632486540520290 ) ) ;
#2749 = VERTEX_POINT ( 'NONE', #21554 ) ;
#2750 = CARTESIAN_POINT ( 'NONE',  ( 111.2886751345946834, 2.000000000000001776, 3.330669073875469621E-13 ) ) ;
#2751 = CARTESIAN_POINT ( 'NONE',  ( -4.763139720814407951, 2.749999999999946709, -179.7500000000000284 ) ) ;
#2752 = ADVANCED_FACE ( 'NONE', ( #10177 ), #2225, .T. ) ;
#2753 = CARTESIAN_POINT ( 'NONE',  ( 22.83632486540521001, 1.767766952966376426, 1.767766952966376426 ) ) ;
#2754 = ORIENTED_EDGE ( 'NONE', *, *, #10445, .T. ) ;
#2755 = CARTESIAN_POINT ( 'NONE',  ( 22.53867513459501026, 1.110223024625156540E-13, 2.499999999999835687 ) ) ;
#2756 = EDGE_CURVE ( 'NONE', #566, #20580, #1035, .T. ) ;
#2757 = ORIENTED_EDGE ( 'NONE', *, *, #23319, .T. ) ;
#2758 = EDGE_LOOP ( 'NONE', ( #26210, #2327, #29337, #1440 ) ) ;
#2759 = FACE_OUTER_BOUND ( 'NONE', #18505, .T. ) ;
#2760 = CARTESIAN_POINT ( 'NONE',  ( 160.1250000000000568, 0.000000000000000000, -6.000000000000005329 ) ) ;
#2761 = ORIENTED_EDGE ( 'NONE', *, *, #5141, .T. ) ;
#2762 = CARTESIAN_POINT ( 'NONE',  ( 5.412658773652712085, -3.125000000000086153, -129.0669872981078470 ) ) ;
#2763 = CARTESIAN_POINT ( 'NONE',  ( 12.18750000000008349, 1.097466725451679892, -2.649519052838238409 ) ) ;
#2764 = CARTESIAN_POINT ( 'NONE',  ( 19.14882486540521356, -2.499999999999964473, 1.035533905932749299 ) ) ;
#2765 = VERTEX_POINT ( 'NONE', #24889 ) ;
#2766 = CARTESIAN_POINT ( 'NONE',  ( 19.06250000000013500, 2.000000000000091926, 0.8284271247461753029 ) ) ;
#2767 = CARTESIAN_POINT ( 'NONE',  ( -4.999999999999886313, -70.00000000000001421, 5.000000000000004441 ) ) ;
#2768 = DIRECTION ( 'NONE',  ( 0.000000000000000000, 0.000000000000000000, -1.000000000000000000 ) ) ;
#2769 = FACE_OUTER_BOUND ( 'NONE', #17397, .T. ) ;
#2770 = CARTESIAN_POINT ( 'NONE',  ( 135.3601497308104342, -3.535533905932725318, -3.535533905932725318 ) ) ;
#2771 = CARTESIAN_POINT ( 'NONE',  ( 22.60117513459491434, -1.035533905932629173, 2.499999999999784173 ) ) ;
#2772 = CARTESIAN_POINT ( 'NONE',  ( 6.000000000000052403, -1.607695154586662678, -99.15331216351297883 ) ) ;
#2773 = CARTESIAN_POINT ( 'NONE',  ( 5.196152422706629359, 3.000000000000002665, -146.9613248654052597 ) ) ;
#2774 = DIRECTION ( 'NONE',  ( -1.000000000000000000, 1.387778780781444413E-14, 0.000000000000000000 ) ) ;
#2775 =( NAMED_UNIT ( * ) PLANE_ANGLE_UNIT ( ) SI_UNIT ( $, .RADIAN. ) );
#2776 = CARTESIAN_POINT ( 'NONE',  ( 107.1874999999997584, 1.035533905932779275, 2.500000000000205169 ) ) ;
#2777 = PRESENTATION_LAYER_ASSIGNMENT (  '', '', ( #29240 ) ) ;
#2778 = CARTESIAN_POINT ( 'NONE',  ( 104.7401757384976975, 1.138422607625655392, -1.478012502211212054 ) ) ;
#2779 = ORIENTED_EDGE ( 'NONE', *, *, #3365, .F. ) ;
#2780 = CARTESIAN_POINT ( 'NONE',  ( 3.175426480543072749, 5.499999999999865885, -48.12500000000000000 ) ) ;
#2781 = DIRECTION ( 'NONE',  ( 0.000000000000000000, 0.000000000000000000, 1.000000000000000000 ) ) ;
#2782 =( NAMED_UNIT ( * ) SI_UNIT ( $, .STERADIAN. ) SOLID_ANGLE_UNIT ( ) );
#2783 = EDGE_LOOP ( 'NONE', ( #3660, #529, #9080, #20842 ) ) ;
#2784 = AXIS2_PLACEMENT_3D ( 'NONE', #19725, #29071, #26756 ) ;
#2785 = CARTESIAN_POINT ( 'NONE',  ( 117.5622167782373992, 1.849990392679562001, -0.7662911109076485650 ) ) ;
#2786 =( NAMED_UNIT ( * ) SI_UNIT ( $, .STERADIAN. ) SOLID_ANGLE_UNIT ( ) );
#2787 = CARTESIAN_POINT ( 'NONE',  ( 12.12500000000005329, 1.414213562373201061, 1.414213562373034527 ) ) ;
#2788 = CARTESIAN_POINT ( 'NONE',  ( -3.608439182435052128, -6.250000000000110134, -100.9419872981078186 ) ) ;
#2789 = CARTESIAN_POINT ( 'NONE',  ( -5.999999999999971578, 1.607695154586715303, -172.4806624327026157 ) ) ;
#2790 = ADVANCED_FACE ( 'NONE', ( #26875 ), #1230, .T. ) ;
#2791 = CARTESIAN_POINT ( 'NONE',  ( 135.0000000000000284, 6.000000000000005329, 0.000000000000000000 ) ) ;
#2792 = CARTESIAN_POINT ( 'NONE',  ( 118.4374999999998721, -2.499999999999964473, 1.035533905932929599 ) ) ;
#2793 = VECTOR ( 'NONE', #191, 1000.000000000000000 ) ;
#2794 = AXIS2_PLACEMENT_3D ( 'NONE', #3371, #24884, #24425 ) ;
#2795 = CARTESIAN_POINT ( 'NONE',  ( 0.000000000000000000, 5.499999999999991118, -127.5000000000000568 ) ) ;
#2796 = ORIENTED_EDGE ( 'NONE', *, *, #1289, .T. ) ;
#2797 = CARTESIAN_POINT ( 'NONE',  ( 115.5238248654051176, 0.8284271247462955401, -1.999999999999851674 ) ) ;
#2798 = CARTESIAN_POINT ( 'NONE',  ( 0.000000000000000000, 5.499999999999991118, -60.00000000000005684 ) ) ;
#2799 = CARTESIAN_POINT ( 'NONE',  ( 3.464101615137757051, -5.999999999999979572, -81.33632486540523132 ) ) ;
#2800 = CARTESIAN_POINT ( 'NONE',  ( 109.1011751345947687, 0.8284271247462955401, -1.999999999999911626 ) ) ;
#2801 = CARTESIAN_POINT ( 'NONE',  ( 2.775557561562891351E-14, 6.250000000000033751, -82.93301270189223828 ) ) ;
#2802 = CARTESIAN_POINT ( 'NONE',  ( 2.775557561562891351E-14, 10.99999999999998224, -31.00000000000002842 ) ) ;
#2803 = VECTOR ( 'NONE', #6598, 1000.000000000000000 ) ;
#2804 = CARTESIAN_POINT ( 'NONE',  ( 5.999999999999999112, 2.951592740943527306E-14, -150.0863248654052313 ) ) ;
#2805 = CARTESIAN_POINT ( 'NONE',  ( 107.6247167782376124, 1.849990392679523588, 0.000000000000000000 ) ) ;
#2806 = LINE ( 'NONE', #9896, #23463 ) ;
#2807 = CARTESIAN_POINT ( 'NONE',  ( 5.999999999999949374, 1.607695154586804565, -61.51933756729744118 ) ) ;
#2808 = CARTESIAN_POINT ( 'NONE',  ( 115.1877832217620892, 0.7662911109078588412, -1.849990392679231599 ) ) ;
#2809 = CARTESIAN_POINT ( 'NONE',  ( -4.763139720814407951, 2.749999999999946709, -140.7500000000000284 ) ) ;
#2810 = DIRECTION ( 'NONE',  ( 0.000000000000000000, 0.000000000000000000, -1.000000000000000000 ) ) ;
#2811 = CARTESIAN_POINT ( 'NONE',  ( -5.412658773652739619, 3.124999999999975131, -150.1830127018922667 ) ) ;
#2812 = CARTESIAN_POINT ( 'NONE',  ( -5.999999999999963585, -1.487416814333745711E-14, -101.3363248654052171 ) ) ;
#2813 = VECTOR ( 'NONE', #2540, 1000.000000000000000 ) ;
#2814 = CYLINDRICAL_SURFACE ( 'NONE', #17181, 5.500000000000000000 ) ;
#2815 = EDGE_CURVE ( 'NONE', #2765, #25369, #27340, .T. ) ;
#2816 = CARTESIAN_POINT ( 'NONE',  ( -4.763139720814407951, -2.750000000000016431, -68.50000000000000000 ) ) ;
#2817 = CARTESIAN_POINT ( 'NONE',  ( -5.999999999999963585, 1.780251999655701777E-13, -85.41367513459483973 ) ) ;
#2818 = CARTESIAN_POINT ( 'NONE',  ( -2.775557561562891351E-14, -5.500000000000115463, -68.25000000000002842 ) ) ;
#2819 = CARTESIAN_POINT ( 'NONE',  ( 6.000000000000000888, -1.859271017917181981E-14, -54.08632486540521001 ) ) ;
#2820 = CARTESIAN_POINT ( 'NONE',  ( 142.7961002691896510, 2.071067811865468400, -4.999999999999989342 ) ) ;
#2821 = CARTESIAN_POINT ( 'NONE',  ( 145.5863248654052313, 0.000000000000000000, 5.500000000000005329 ) ) ;
#2822 = CARTESIAN_POINT ( 'NONE',  ( 152.6250000000000284, 0.000000000000000000, -6.000000000000005329 ) ) ;
#2823 = CARTESIAN_POINT ( 'NONE',  ( -5.999999999999971578, 1.607695154586715303, -133.4806624327025872 ) ) ;
#2824 = CARTESIAN_POINT ( 'NONE',  ( 6.000000000000000888, -1.607695154586752384, -147.1533121635130215 ) ) ;
#2825 = FACE_OUTER_BOUND ( 'NONE', #21627, .T. ) ;
#2826 = ADVANCED_FACE ( 'NONE', ( #6159 ), #2685, .T. ) ;
#2827 = ORIENTED_EDGE ( 'NONE', *, *, #24879, .T. ) ;
#2828 = CARTESIAN_POINT ( 'NONE',  ( 152.8125000000000568, 4.242640687119298093, -4.242640687119298093 ) ) ;
#2829 = VECTOR ( 'NONE', #21429, 1000.000000000000000 ) ;
#2830 = CARTESIAN_POINT ( 'NONE',  ( 112.6877832217621034, -0.7662911109076184779, 1.849990392679652151 ) ) ;
#2831 = CARTESIAN_POINT ( 'NONE',  ( 11.53867513459497296, 5.551115123125782702E-14, 2.500000000000002220 ) ) ;
#2832 =( BOUNDED_CURVE ( )  B_SPLINE_CURVE ( 2, ( #29045, #10190, #15431, #24758, #14950, #3698, #27199, #24292, #3238 ),
 .UNSPECIFIED., .F., .F. ) 
 B_SPLINE_CURVE_WITH_KNOTS ( ( 3, 2, 2, 2, 3 ),
 ( 0.8875000000000003997, 0.8937500000000002665, 0.9000000000000000222, 0.9062499999999997780, 0.9124999999999995337 ),
 .UNSPECIFIED. ) 
 CURVE ( )  GEOMETRIC_REPRESENTATION_ITEM ( )  RATIONAL_B_SPLINE_CURVE ( ( 0.9999999999999945599, 0.9238795325112921786, 1.000000000000000000, 0.9238795325112867385, 1.000000000000000000, 0.9238795325112867385, 1.000000000000000000, 0.9238795325112921786, 0.9999999999999945599 ) ) 
 REPRESENTATION_ITEM ( '' )  );
#2833 = CARTESIAN_POINT ( 'NONE',  ( -2.775557561562891351E-14, -5.500000000000115463, -177.7500000000000284 ) ) ;
#2834 = CARTESIAN_POINT ( 'NONE',  ( 22.43750000000002842, -1.999999999999851674, 0.8284271247462354770 ) ) ;
#2835 = ORIENTED_EDGE ( 'NONE', *, *, #12855, .F. ) ;
#2836 = CARTESIAN_POINT ( 'NONE',  ( -4.763139720814407951, 2.749999999999946709, -83.74999999999998579 ) ) ;
#2837 = CARTESIAN_POINT ( 'NONE',  ( -5.412658773652684552, -3.125000000000099920, -98.93301270189225249 ) ) ;
#2838 = ORIENTED_EDGE ( 'NONE', *, *, #5555, .T. ) ;
#2839 = MECHANICAL_DESIGN_GEOMETRIC_PRESENTATION_REPRESENTATION (  '', ( #24414 ), #25396 ) ;
#2840 = CARTESIAN_POINT ( 'NONE',  ( -5.999999999999963585, -1.487416814333745711E-14, -128.3363248654052029 ) ) ;
#2841 = CARTESIAN_POINT ( 'NONE',  ( 111.1636751345946976, 1.414213562373145550, -1.414213562373145550 ) ) ;
#2842 = CARTESIAN_POINT ( 'NONE',  ( 124.9999999999999432, -70.00000000000000000, 8.000000000000007105 ) ) ;
#2843 = CARTESIAN_POINT ( 'NONE',  ( 111.5863248654051887, 1.414213562373090038, -1.414213562373145550 ) ) ;
#2844 = CARTESIAN_POINT ( 'NONE',  ( 135.0000273856245201, -6.966962943922541562, 8.502862253531825232 ) ) ;
#2845 = CARTESIAN_POINT ( 'NONE',  ( -3.175426480542816066, 5.499999999999865885, -166.3750000000000568 ) ) ;
#2846 = CARTESIAN_POINT ( 'NONE',  ( 6.000000000000000888, 1.607695154586715303, -58.51933756729743408 ) ) ;
#2847 = COLOUR_RGB ( '', 0.40784314, 0.44705882, 0.49803922) ;
#2848 = CARTESIAN_POINT ( 'NONE',  ( 3.175426480543072749, 5.499999999999865885, -154.6250000000000853 ) ) ;
#2849 = EDGE_CURVE ( 'NONE', #9948, #12840, #10858, .T. ) ;
#2850 = CARTESIAN_POINT ( 'NONE',  ( -3.464101615137725076, 5.999999999999979572, -76.66367513459483973 ) ) ;
#2851 = CARTESIAN_POINT ( 'NONE',  ( 148.5863248654052313, 0.000000000000000000, 5.500000000000005329 ) ) ;
#2852 = ADVANCED_FACE ( 'NONE', ( #27188 ), #29181, .F. ) ;
#2853 = CARTESIAN_POINT ( 'NONE',  ( 0.000000000000000000, 5.499999999999991118, -96.00000000000002842 ) ) ;
#2854 = CARTESIAN_POINT ( 'NONE',  ( 144.9449251345948255, -5.500000000000012434, 2.278174593052012309 ) ) ;
#2855 = CARTESIAN_POINT ( 'NONE',  ( -4.763139720814407951, 2.749999999999946709, -88.25000000000005684 ) ) ;
#2856 = CARTESIAN_POINT ( 'NONE',  ( 107.0386751345946550, 5.551115123125782702E-14, -2.000000000000001776 ) ) ;
#2857 = CARTESIAN_POINT ( 'NONE',  ( 24.37500000000014566, -1.414213562373034527, 1.414213562373034527 ) ) ;
#2858 = CARTESIAN_POINT ( 'NONE',  ( 114.9374999999997868, 2.500000000000055067, -1.035533905932629173 ) ) ;
#2859 = CARTESIAN_POINT ( 'NONE',  ( 6.000000000000000888, -1.859271017917181981E-14, -126.6636751345948397 ) ) ;
#2860 = EDGE_CURVE ( 'NONE', #23232, #25957, #1088, .T. ) ;
#2861 = DIRECTION ( 'NONE',  ( -7.147005652999508048E-36, 5.642372883946980038E-36, 1.000000000000000000 ) ) ;
#2862 = ORIENTED_EDGE ( 'NONE', *, *, #14815, .T. ) ;
#2863 = SURFACE_STYLE_USAGE ( .BOTH. , #14573 ) ;
#2864 = CARTESIAN_POINT ( 'NONE',  ( -0.08385222888512024186, -15.14261269756462269, -7.883965026287834910 ) ) ;
#2865 = CARTESIAN_POINT ( 'NONE',  ( 121.3752832217622881, 1.849990392679579099, 0.000000000000000000 ) ) ;
#2866 = ORIENTED_EDGE ( 'NONE', *, *, #14291, .T. ) ;
#2867 = CARTESIAN_POINT ( 'NONE',  ( 145.9687500000000568, -2.485281374238585972, 6.000000000000005329 ) ) ;
#2868 = ORIENTED_EDGE ( 'NONE', *, *, #14613, .T. ) ;
#2869 = CARTESIAN_POINT ( 'NONE',  ( 3.175426480543072749, 5.499999999999865885, -106.6250000000000284 ) ) ;
#2870 = CARTESIAN_POINT ( 'NONE',  ( 20.37500000000017053, 2.649519052838555933, 0.000000000000000000 ) ) ;
#2871 = CARTESIAN_POINT ( 'NONE',  ( 6.350852961086080661, -9.614813431917819062E-14, -150.3749999999999716 ) ) ;
#2872 = CARTESIAN_POINT ( 'NONE',  ( 5.412658773652739619, 3.124999999999988898, -122.1830127018922525 ) ) ;
#2873 = UNCERTAINTY_MEASURE_WITH_UNIT (LENGTH_MEASURE( 1.000000000000000082E-05 ), #8792, 'distance_accuracy_value', 'NONE');
#2874 = ORIENTED_EDGE ( 'NONE', *, *, #20069, .F. ) ;
#2875 = CARTESIAN_POINT ( 'NONE',  ( -5.196152422706601826, 2.999999999999975131, -111.0386751345948113 ) ) ;
#2876 = CARTESIAN_POINT ( 'NONE',  ( -3.608439182435115633, 6.249999999999965361, -159.9419872981077901 ) ) ;
#2877 = CARTESIAN_POINT ( 'NONE',  ( 107.5624999999998153, -2.499999999999874767, -1.035533905932629173 ) ) ;
#2878 = CARTESIAN_POINT ( 'NONE',  ( 133.0163997308104058, 4.999999999999989342, 2.071067811865468400 ) ) ;
#2879 = CARTESIAN_POINT ( 'NONE',  ( 5.412658773652739619, 3.124999999999988898, -60.68301270189224539 ) ) ;
#2880 = ORIENTED_EDGE ( 'NONE', *, *, #17113, .T. ) ;
#2881 = CARTESIAN_POINT ( 'NONE',  ( 6.000000000000000888, -1.859271017917181981E-14, -168.0863248654052029 ) ) ;
#2882 = CARTESIAN_POINT ( 'NONE',  ( -0.4007817556719547869, 11.00000000000000711, -19.00000000000001066 ) ) ;
#2883 = DIRECTION ( 'NONE',  ( 0.000000000000000000, 0.000000000000000000, -1.000000000000000000 ) ) ;
#2884 = CARTESIAN_POINT ( 'NONE',  ( -4.763139720814407951, 2.749999999999946709, -175.2500000000000284 ) ) ;
#2885 = CARTESIAN_POINT ( 'NONE',  ( 109.2502832217621602, 1.308140751793751555, -1.308140751793640533 ) ) ;
#2886 = CARTESIAN_POINT ( 'NONE',  ( 5.196152422706629359, 3.000000000000002665, -100.4613248654052171 ) ) ;
#2887 = CARTESIAN_POINT ( 'NONE',  ( -5.412658773652684552, -3.125000000000099920, -179.9330127018922099 ) ) ;
#2888 = PLANE ( 'NONE',  #25881 ) ;
#2889 = EDGE_CURVE ( 'NONE', #9651, #8975, #3687, .T. ) ;
#2890 = CARTESIAN_POINT ( 'NONE',  ( -5.999999999999963585, 1.780251999655701777E-13, -48.83632486540521711 ) ) ;
#2891 = CARTESIAN_POINT ( 'NONE',  ( 4.763139720814407951, 2.750000000000002665, -118.7500000000000284 ) ) ;
#2892 = CARTESIAN_POINT ( 'NONE',  ( 0.000000000000000000, 5.999999999999977796, -84.28867513459481131 ) ) ;
#2893 = CARTESIAN_POINT ( 'NONE',  ( -3.175426480542816510, 5.499999999999865885, -116.8750000000000142 ) ) ;
#2894 = CARTESIAN_POINT ( 'NONE',  ( 148.6949251345948539, 5.500000000000012434, -2.278174593052012309 ) ) ;
#2895 = VERTEX_POINT ( 'NONE', #9506 ) ;
#2896 = CARTESIAN_POINT ( 'NONE',  ( 16.62500000000008527, 2.649519052838444910, -1.110223024625156540E-13 ) ) ;
#2897 = LINE ( 'NONE', #19205, #8416 ) ;
#2898 = CARTESIAN_POINT ( 'NONE',  ( 3.464101615137757051, -5.999999999999979572, -55.83632486540525264 ) ) ;
#2899 = EDGE_CURVE ( 'NONE', #15450, #9582, #1401, .T. ) ;
#2900 = EDGE_CURVE ( 'NONE', #12068, #17448, #1468, .T. ) ;
#2901 = CARTESIAN_POINT ( 'NONE',  ( -5.196152422706573404, -3.000000000000002665, -126.7113248654052597 ) ) ;
#2902 = CARTESIAN_POINT ( 'NONE',  ( 17.35117513459481131, 2.500000000000084821, 1.035533905932689347 ) ) ;
#2903 = EDGE_LOOP ( 'NONE', ( #27728, #28703, #9986, #25114 ) ) ;
#2904 = CARTESIAN_POINT ( 'NONE',  ( -5.999999999999963585, 1.780251999655701777E-13, -95.91367513459483973 ) ) ;
#2905 = VERTEX_POINT ( 'NONE', #27261 ) ;
#2906 = ORIENTED_EDGE ( 'NONE', *, *, #6480, .T. ) ;
#2907 = CARTESIAN_POINT ( 'NONE',  ( 1.110223024625164183E-16, -2.000000000000012879, -1.776356839400262692E-15 ) ) ;
#2908 = CARTESIAN_POINT ( 'NONE',  ( 135.2961002691896226, 2.071067811865468400, -4.999999999999989342 ) ) ;
#2909 = ORIENTED_EDGE ( 'NONE', *, *, #2900, .F. ) ;
#2910 = CARTESIAN_POINT ( 'NONE',  ( -7.216878364870328078, 0.000000000000000000, -128.1919872981078186 ) ) ;
#2911 = CARTESIAN_POINT ( 'NONE',  ( 24.14882486540529527, -2.499999999999964473, 1.035533905932749299 ) ) ;
#2912 = CARTESIAN_POINT ( 'NONE',  ( 10.87500000000005151, -2.649519052838111843, -5.551115123125782702E-14 ) ) ;
#2913 = CARTESIAN_POINT ( 'NONE',  ( -3.464101615137757051, -5.999999999999979572, -116.6636751345947545 ) ) ;
#2914 = ORIENTED_EDGE ( 'NONE', *, *, #22757, .F. ) ;
#2915 = CARTESIAN_POINT ( 'NONE',  ( 19.68750000000015632, -0.8284271247461152399, -1.999999999999971800 ) ) ;
#2916 = DIRECTION ( 'NONE',  ( 1.000000000000000000, 0.000000000000000000, -0.000000000000000000 ) ) ;
#2917 = DIRECTION ( 'NONE',  ( -0.000000000000000000, -0.000000000000000000, -1.000000000000000000 ) ) ;
#2918 =( BOUNDED_CURVE ( )  B_SPLINE_CURVE ( 2, ( #18115, #17820, #13222, #24692, #15369, #1799, #6401, #8245, #8565 ),
 .UNSPECIFIED., .F., .T. ) 
 B_SPLINE_CURVE_WITH_KNOTS ( ( 3, 2, 2, 2, 3 ),
 ( 0.1416666666666666907, 0.1425925925925926041, 0.1444444444444444309, 0.1462962962962962854, 0.1472222222222221988 ),
 .UNSPECIFIED. ) 
 CURVE ( )  GEOMETRIC_REPRESENTATION_ITEM ( )  RATIONAL_B_SPLINE_CURVE ( ( 0.9330127018922194093, 0.9330127018922204085, 1.000000000000000000, 0.8660254037844388186, 1.000000000000000000, 0.8660254037844388186, 1.000000000000000000, 0.9330127018922205195, 0.9330127018922196314 ) ) 
 REPRESENTATION_ITEM ( '' )  );
#2919 = CARTESIAN_POINT ( 'NONE',  ( 138.8288997308104058, 4.999999999999989342, -2.071067811865468400 ) ) ;
#2920 = CARTESIAN_POINT ( 'NONE',  ( 137.9925748654052029, 2.278174593052074925, 5.499999999999950262 ) ) ;
#2921 = CARTESIAN_POINT ( 'NONE',  ( 6.000000000000052403, -1.607695154586662678, -139.6533121635129930 ) ) ;
#2922 = CARTESIAN_POINT ( 'NONE',  ( 5.196152422706629359, -2.999999999999988898, -69.21132486540521711 ) ) ;
#2923 = CARTESIAN_POINT ( 'NONE',  ( 105.0624999999998437, 2.500000000000054623, 1.035533905932869425 ) ) ;
#2924 = ADVANCED_FACE ( 'NONE', ( #29583 ), #21847, .F. ) ;
#2925 = CARTESIAN_POINT ( 'NONE',  ( -5.196152422706573404, -3.000000000000002665, -143.2113248654052313 ) ) ;
#2926 = TOROIDAL_SURFACE ( 'NONE', #6853, 10.49999999999998934, 0.5000000000000000000 ) ;
#2927 = CARTESIAN_POINT ( 'NONE',  ( -6.350852961085760029, -1.281975124255709124E-13, -136.1250000000000568 ) ) ;
#2928 = CARTESIAN_POINT ( 'NONE',  ( 1.000000000000000888, -14.99923475244191451, -9.015151515151503148 ) ) ;
#2929 = VERTEX_POINT ( 'NONE', #24959 ) ;
#2930 = CARTESIAN_POINT ( 'NONE',  ( 108.1011751345946692, 0.8284271247463257382, -1.999999999999731104 ) ) ;
#2931 = DIRECTION ( 'NONE',  ( 1.000000000000000000, 0.000000000000000000, 0.000000000000000000 ) ) ;
#2932 = ADVANCED_FACE ( 'NONE', ( #29724 ), #12887, .T. ) ;
#2933 = CARTESIAN_POINT ( 'NONE',  ( 112.2886751345947118, 2.000000000000112799, 3.330669073875469621E-13 ) ) ;
#2934 = VERTEX_POINT ( 'NONE', #3608 ) ;
#2935 = CARTESIAN_POINT ( 'NONE',  ( 117.8747167782375840, 2.775557561562891351E-14, 1.849990392679523588 ) ) ;
#2936 = DIRECTION ( 'NONE',  ( 1.000000000000000000, 1.665334536937731113E-16, -1.526556658859586792E-16 ) ) ;
#2937 = CARTESIAN_POINT ( 'NONE',  ( -3.608439182435115633, 6.249999999999965361, -95.44198729810779014 ) ) ;
#2938 = CARTESIAN_POINT ( 'NONE',  ( 0.000000000000000000, 0.000000000000000000, 0.000000000000000000 ) ) ;
#2939 = CARTESIAN_POINT ( 'NONE',  ( 20.89882486540530948, 1.035533905932809473, 2.499999999999844569 ) ) ;
#2940 = CARTESIAN_POINT ( 'NONE',  ( 118.8124999999998579, 1.035533905932749299, -2.499999999999784173 ) ) ;
#2941 = CYLINDRICAL_SURFACE ( 'NONE', #14986, 1.000000000000000000 ) ;
#2942 = AXIS2_PLACEMENT_3D ( 'NONE', #11189, #17802, #25263 ) ;
#2943 = CARTESIAN_POINT ( 'NONE',  ( 0.000000000000000000, 5.499999999999991118, -126.0000000000000000 ) ) ;
#2944 = ORIENTED_EDGE ( 'NONE', *, *, #3388, .T. ) ;
#2945 = EDGE_LOOP ( 'NONE', ( #7663, #23528, #21633, #126 ) ) ;
#2946 = CIRCLE ( 'NONE', #28920, 15.00000000000000000 ) ;
#2947 = CARTESIAN_POINT ( 'NONE',  ( -5.196152422706601826, 2.999999999999975131, -96.03867513459485394 ) ) ;
#2948 = CARTESIAN_POINT ( 'NONE',  ( -4.763139720814407951, 2.749999999999946709, -55.25000000000002132 ) ) ;
#2949 = DIRECTION ( 'NONE',  ( 1.000000000000000000, 0.000000000000000000, -0.000000000000000000 ) ) ;
#2950 = CARTESIAN_POINT ( 'NONE',  ( 159.5344527694593921, -12.11656139239292784, -3.856021467126169000 ) ) ;
#2951 = CARTESIAN_POINT ( 'NONE',  ( 3.035671606378345100, 10.57820549248699926, -19.81012201018821273 ) ) ;
#2952 = CARTESIAN_POINT ( 'NONE',  ( -5.412658773652739619, 3.124999999999975131, -81.18301270189220986 ) ) ;
#2953 = CARTESIAN_POINT ( 'NONE',  ( -5.999999999999971578, 1.607695154586715303, -168.9033121635130215 ) ) ;
#2954 = DIRECTION ( 'NONE',  ( -1.000000000000000000, -0.000000000000000000, -0.000000000000000000 ) ) ;
#2955 = FILL_AREA_STYLE_COLOUR ( '', #25889 ) ;
#2956 = EDGE_CURVE ( 'NONE', #28521, #23217, #28112, .T. ) ;
#2957 = CARTESIAN_POINT ( 'NONE',  ( 115.9377832217620323, -1.849990392679441875, -0.7662911109075283278 ) ) ;
#2958 = EDGE_CURVE ( 'NONE', #14503, #25740, #14966, .T. ) ;
#2959 = CARTESIAN_POINT ( 'NONE',  ( 3.175426480543072749, 5.499999999999865885, -136.6250000000000568 ) ) ;
#2960 = CARTESIAN_POINT ( 'NONE',  ( 140.4999999888488276, -9.513811511959360701, 7.314917984054192246 ) ) ;
#2961 = CARTESIAN_POINT ( 'NONE',  ( -3.608439182435115633, 6.249999999999965361, -151.8080127018922383 ) ) ;
#2962 = CARTESIAN_POINT ( 'NONE',  ( 10.03867513459497118, 1.110223024625156540E-13, -2.500000000000113243 ) ) ;
#2963 = CARTESIAN_POINT ( 'NONE',  ( 3.175426480543072749, 5.499999999999865885, -67.62500000000002842 ) ) ;
#2964 = CARTESIAN_POINT ( 'NONE',  ( -4.763139720814407951, -2.750000000000016431, -61.00000000000000000 ) ) ;
#2965 = CARTESIAN_POINT ( 'NONE',  ( 146.9211002691896510, -4.999999999999989342, -2.071067811865468400 ) ) ;
#2966 = CARTESIAN_POINT ( 'NONE',  ( 152.4375000000000284, -4.242640687119298093, -4.242640687119298093 ) ) ;
#2967 = CARTESIAN_POINT ( 'NONE',  ( 135.0000000000000284, -9.047800747817580813, -7.500000000000007105 ) ) ;
#2968 = CARTESIAN_POINT ( 'NONE',  ( 17.37500000000011369, -1.414213562372979016, 1.414213562373034527 ) ) ;
#2969 = CARTESIAN_POINT ( 'NONE',  ( 1.110223024625164183E-16, -2.000000000000012879, -1.776356839400262692E-15 ) ) ;
#2970 = CARTESIAN_POINT ( 'NONE',  ( 135.0000000000000284, -12.00000000000001066, -5.000000000000004441 ) ) ;
#2972 = EDGE_LOOP ( 'NONE', ( #19771, #1972, #9379, #9654 ) ) ;
#2971 = AXIS2_PLACEMENT_3D ( 'NONE', #1906, #11313, #30010 ) ;
#2973 = CARTESIAN_POINT ( 'NONE',  ( 153.0000000000000284, 6.000000000000005329, 0.000000000000000000 ) ) ;
#2974 = DIRECTION ( 'NONE',  ( -1.000000000000000000, -1.665334536937736783E-16, -2.220446049250315546E-16 ) ) ;
#2975 = UNCERTAINTY_MEASURE_WITH_UNIT (LENGTH_MEASURE( 1.000000000000000082E-05 ), #20026, 'distance_accuracy_value', 'NONE');
#2976 = LINE ( 'NONE', #24318, #19245 ) ;
#2977 = CARTESIAN_POINT ( 'NONE',  ( -3.175426480542816510, -5.500000000000057732, -179.3750000000000568 ) ) ;
#2978 = CARTESIAN_POINT ( 'NONE',  ( 21.68750000000000711, -0.8284271247461753029, -2.000000000000031530 ) ) ;
#2979 = CARTESIAN_POINT ( 'NONE',  ( -5.412658773652739619, 3.124999999999975131, -153.8169872981078186 ) ) ;
#2980 = ORIENTED_EDGE ( 'NONE', *, *, #18472, .T. ) ;
#2981 = CARTESIAN_POINT ( 'NONE',  ( -3.175426480542816510, 5.499999999999865885, -83.87500000000004263 ) ) ;
#2982 = AXIS2_PLACEMENT_3D ( 'NONE', #23278, #9278, #2507 ) ;
#2983 = CARTESIAN_POINT ( 'NONE',  ( 2.775557561562891351E-14, -6.250000000000061284, -100.1830127018922241 ) ) ;
#2984 = VERTEX_POINT ( 'NONE', #8221 ) ;
#2985 = CIRCLE ( 'NONE', #3972, 1.000000000000000000 ) ;
#2986 = CARTESIAN_POINT ( 'NONE',  ( 119.9999999999998153, 0.1805100831983324217, 2.088914846013814053 ) ) ;
#2987 = CARTESIAN_POINT ( 'NONE',  ( 3.175426480543072749, 5.499999999999865885, -168.1250000000000000 ) ) ;
#2988 = CARTESIAN_POINT ( 'NONE',  ( 125.0000000000000568, -55.00000000000000711, -5.000000000000004441 ) ) ;
#2989 = CARTESIAN_POINT ( 'NONE',  ( 4.754775042825850839, -9.920200456738756500, -21.33539821540183468 ) ) ;
#2990 = DIRECTION ( 'NONE',  ( 5.551115123125785167E-17, -1.000000000000000000, -8.881784197001256268E-16 ) ) ;
#2991 = ADVANCED_FACE ( 'NONE', ( #17635 ), #27716, .T. ) ;
#2992 = CARTESIAN_POINT ( 'NONE',  ( 3.175426480543072749, -5.500000000000105693, -162.6250000000000568 ) ) ;
#2993 = CARTESIAN_POINT ( 'NONE',  ( -3.464101615137725076, 5.999999999999979572, -161.5863248654051745 ) ) ;
#2994 = CARTESIAN_POINT ( 'NONE',  ( 3.175426480543072749, -5.500000000000105693, -146.1250000000000000 ) ) ;
#2995 = CARTESIAN_POINT ( 'NONE',  ( 135.0000000000000284, 5.526307313663695098, 1.967927276880694576 ) ) ;
#2996 = CARTESIAN_POINT ( 'NONE',  ( -3.175426480542816066, -5.500000000000057732, -96.87499999999997158 ) ) ;
#2997 = CARTESIAN_POINT ( 'NONE',  ( 6.000000000000000888, -1.859271017917181981E-14, -126.0863248654052171 ) ) ;
#2998 =( BOUNDED_CURVE ( )  B_SPLINE_CURVE ( 2, ( #16258, #9148, #11645, #11492, #25411, #13487, #27403, #9300, #13958 ),
 .UNSPECIFIED., .F., .F. ) 
 B_SPLINE_CURVE_WITH_KNOTS ( ( 3, 2, 2, 2, 3 ),
 ( 0.6416666666666667185, 0.6425925925925926041, 0.6444444444444444864, 0.6462962962962962576, 0.6472222222222221433 ),
 .UNSPECIFIED. ) 
 CURVE ( )  GEOMETRIC_REPRESENTATION_ITEM ( )  RATIONAL_B_SPLINE_CURVE ( ( 0.9330127018922194093, 0.9330127018922234061, 1.000000000000000000, 0.8660254037844388186, 1.000000000000000000, 0.8660254037844388186, 1.000000000000000000, 0.9330127018922234061, 0.9330127018922194093 ) ) 
 REPRESENTATION_ITEM ( '' )  );
#2999 = CARTESIAN_POINT ( 'NONE',  ( -2.775557561562891351E-14, -5.500000000000115463, -92.25000000000000000 ) ) ;
#3000 = CARTESIAN_POINT ( 'NONE',  ( 116.0000000000000142, 6.735557395310442023E-16, 5.500000000000000000 ) ) ;
#3001 = CARTESIAN_POINT ( 'NONE',  ( -5.999999999999971578, 1.607695154586715303, -143.4033121635129930 ) ) ;
#3002 = CARTESIAN_POINT ( 'NONE',  ( 9.375000000000078160, 1.110223024625156540E-13, -2.649519052838444910 ) ) ;
#3003 = CARTESIAN_POINT ( 'NONE',  ( 109.8749999999998437, 1.767766952966320915, -1.767766952966209892 ) ) ;
#3004 = FACE_OUTER_BOUND ( 'NONE', #20337, .T. ) ;
#3005 = AXIS2_PLACEMENT_3D ( 'NONE', #9363, #2450, #4128 ) ;
#3006 = CARTESIAN_POINT ( 'NONE',  ( -6.000000000000000888, 1.067854986875958443E-15, 7.560779664488942560E-35 ) ) ;
#3007 =( BOUNDED_SURFACE ( )  B_SPLINE_SURFACE ( 1, 2, ( 
 ( #19844, #3543, #13585, #6628, #30279, #20621, #22770, #29968, #6475, #1561, #8631, #8794, #27352, #22923, #22625, #20315, #18181, #11433, #25197, #6315, #4322, #29662, #18336, #1866, #6780, #6928, #23239, #11268, #23084, #25049, #20928, #15740, #18484, #16198, #29817, #2181, #27952, #11582, #27803, #20457, #13740, #3851, #8946, #1714, #15899, #4009, #10966, #2026, #20778, #13425, #9238, #27498, #18036, #25509, #9088, #11111, #4473, #18632, #4160, #27652, #16050, #30125, #25350, #13899, #16351, #13281, #26265, #23537, #620, #5216, #10005, #19380, #7526, #462, #14630, #18946, #16937, #11895, #4775, #23830, #28409, #2476, #25669, #23975, #173, #2915, #16649, #28704, #5064, #14493, #7675, #317, #4620, #9553, #14050, #2766, #23388, #21535, #2336, #28262, #11735, #19230, #25972, #9853, #21080, #2622, #4916, #14347, #28110, #12, #28558, #9397, #23685, #18789, #12043, #7084, #16498, #21381, #19089, #7390, #16798, #26118, #28861, #14772, #3511, #3204, #10304, #10154, #773, #27013, #5510, #22433, #5978, #1370, #10780, #8273, #22276, #15396, #19668, #24720, #21973, #26562, #15227, #19811, #24256, #17086, #3661, #29008, #20128, #7973, #29472, #26851, #5810, #26413, #22125, #5364, #17382, #24117, #24559, #3064, #12940, #12489, #26697, #1202, #5661, #24412, #19963, #21827, #14917, #10457, #15068, #17535, #3353, #19528, #7820, #12781, #17234, #10611, #29156, #8118, #30088, #8442, #8595, #18000, #11232, #20281, #27767, #4284, #1520, #11393, #6137, #9056, #6745, #6429, #20581, #4434, #25160, #27316, #4125, #11077, #15551, #13247, #13394, #29629, #13546, #27166, #24869, #22737, #16011, #8757, #15704, #18298, #25013, #22887, #1828, #20738, #11548, #16163, #29929, #27612, #3968, #25471, #20421, #13860, #23201, #2148, #20889, #17848, #4587, #27918, #18596, #14013, #2300, #10492, #1819, #4116, #15105, #3234, #7707, #1096, #17114, #29041, #29188, #26440, #3540, #12814, #10646, #12970, #6009 ),
 ( #12661, #22156, #935, #10184, #10337, #8007, #17414, #5693, #8149, #26884, #15263, #22307, #1239, #19997, #8310, #17720, #15427, #22877, #23496, #23645, #9513, #30233, #9354, #11385, #7194, #1977, #4731, #2440, #16153, #18900, #14305, #28221, #14159, #6734, #30386, #29921, #27909, #18439, #2138, #23034, #27601, #18746, #28067, #20728, #16605, #25461, #6580, #11850, #25783, #13696, #21188, #25926, #30079, #9047, #16003, #7043, #4425, #13853, #27756, #4274, #129, #23193, #4874, #2578, #8899, #25303, #11539, #20880, #9196, #18588, #6886, #25632, #4580, #16456, #23351, #14006, #2291, #11696, #21040, #3162, #2870, #24365, #21782, #725, #19621, #17036, #12001, #16894, #24213, #10110, #28964, #19479, #21333, #26213, #17189, #5169, #19336, #14870, #276, #28811, #7771, #7927, #26368, #9659, #14581, #861, #26512, #17337, #5463, #19049, #23933, #10261, #12291, #28655, #26653, #28365, #416, #5317, #9957, #12435, #7626, #5613, #7344, #7482, #16750, #26076, #5017, #14726, #14448, #23783, #12145, #21490, #24069, #2718, #9805, #28513, #569, #3019, #29110, #1628, #8707, #13047, #6085, #5765, #17797, #10560, #29586, #8546, #23608, #21296, #19148, #9619, #21599, #11970, #7310, #12404, #17152, #21896, #833, #10230, #24324, #22347, #15308, #29553, #11000, #27234, #17606, #27084, #29078, #24934, #8042, #1442, #6205, #12852, #15624, #1597, #13316, #22657, #24473, #17760, #17305, #24631, #5732, #19881, #26766, #5579, #6050, #3737, #22195, #20345, #10527, #14984, #26622, #13171, #29227, #3277, #3580, #13008, #20040, #8352, #7387, #7082, #14200, #14047, #4618, #21532, #9395, #16933, #458, #26262, #5213, #2763, #26115, #9849, #23535, #12191, #16496, #8, #19086, #23682, #28108, #20925, #19227, #25823, #28555, #11893, #23974, #12040, #21078, #23386, #14626, #7523, #2912, #30276, #9236, #18629, #27949, #2620, #4772, #9704, #6926, #5060, #315, #16349, #9551, #2475, #14345, #18944, #25668 ) ),
 .UNSPECIFIED., .F., .F., .F. ) 
 B_SPLINE_SURFACE_WITH_KNOTS ( ( 2, 2 ),
 ( 3, 2, 2, 2, 2, 2, 2, 2, 2, 2, 2, 2, 2, 2, 2, 2, 2, 2, 2, 2, 2, 2, 2, 2, 2, 2, 2, 2, 2, 2, 2, 2, 2, 2, 2, 2, 2, 2, 2, 2, 2, 2, 2, 2, 2, 2, 2, 2, 2, 2, 2, 2, 2, 2, 2, 2, 2, 2, 2, 2, 2, 2, 2, 2, 2, 2, 2, 2, 2, 2, 2, 2, 2, 2, 2, 2, 2, 2, 2, 2, 2, 2, 2, 2, 2, 2, 2, 2, 2, 2, 2, 2, 2, 2, 2, 2, 2, 2, 2, 2, 2, 2, 2, 2, 2, 2, 2, 2, 2, 2, 2, 2, 2, 2, 2, 2, 2, 2, 2, 2, 2, 2, 2, 2, 3 ),
 ( 0.000000000000000000, 1.000000000000000000 ),
 ( 0.000000000000000000, 0.007812500000000000000, 0.01562500000000000000, 0.02343750000000000000, 0.03125000000000000000, 0.03906250000000000000, 0.04687500000000000000, 0.05468750000000000000, 0.06250000000000000000, 0.07031250000000000000, 0.07812500000000000000, 0.08593750000000000000, 0.09375000000000000000, 0.1015625000000000000, 0.1093750000000000000, 0.1171875000000000000, 0.1250000000000000000, 0.1328125000000000000, 0.1406250000000000000, 0.1484375000000000000, 0.1562500000000000000, 0.1640625000000000000, 0.1718750000000000000, 0.1796875000000000000, 0.1875000000000000000, 0.1953125000000000000, 0.2031250000000000000, 0.2109375000000000000, 0.2187500000000000000, 0.2265625000000000000, 0.2343750000000000000, 0.2421875000000000000, 0.2500000000000000000, 0.2578125000000000000, 0.2656250000000000000, 0.2734375000000000000, 0.2812500000000000000, 0.2890625000000000000, 0.2968750000000000000, 0.3046875000000000000, 0.3125000000000000000, 0.3203125000000000000, 0.3281250000000000000, 0.3359375000000000000, 0.3437500000000000000, 0.3515625000000000000, 0.3593750000000000000, 0.3671875000000000000, 0.3750000000000000000, 0.3828125000000000000, 0.3906250000000000000, 0.3984375000000000000, 0.4062500000000000000, 0.4140625000000000000, 0.4218750000000000000, 0.4296875000000000000, 0.4375000000000000000, 0.4453125000000000000, 0.4531250000000000000, 0.4609375000000000000, 0.4687500000000000000, 0.4765625000000000000, 0.4843750000000000000, 0.4921875000000000000, 0.5000000000000000000, 0.5078125000000000000, 0.5156250000000000000, 0.5234375000000000000, 0.5312500000000000000, 0.5390625000000000000, 0.5468750000000000000, 0.5546875000000000000, 0.5625000000000000000, 0.5703125000000000000, 0.5781250000000000000, 0.5859375000000000000, 0.5937500000000000000, 0.6015625000000000000, 0.6093750000000000000, 0.6171875000000000000, 0.6250000000000000000, 0.6328125000000000000, 0.6406250000000000000, 0.6484375000000000000, 0.6562500000000000000, 0.6640625000000000000, 0.6718750000000000000, 0.6796875000000000000, 0.6875000000000000000, 0.6953125000000000000, 0.7031250000000000000, 0.7109375000000000000, 0.7187500000000000000, 0.7265625000000000000, 0.7343750000000000000, 0.7421875000000000000, 0.7500000000000000000, 0.7578125000000000000, 0.7656250000000000000, 0.7734375000000000000, 0.7812500000000000000, 0.7890625000000000000, 0.7968750000000000000, 0.8046875000000000000, 0.8125000000000000000, 0.8203125000000000000, 0.8281250000000000000, 0.8359375000000000000, 0.8437500000000000000, 0.8515625000000000000, 0.8593750000000000000, 0.8671875000000000000, 0.8750000000000000000, 0.8828125000000000000, 0.8906250000000000000, 0.8984375000000000000, 0.9062500000000000000, 0.9140625000000000000, 0.9218750000000000000, 0.9296875000000000000, 0.9375000000000000000, 0.9453125000000000000, 0.9531250000000000000, 0.9609375000000000000, 0.9687500000000000000 ),
 .UNSPECIFIED. ) 
 GEOMETRIC_REPRESENTATION_ITEM ( )  RATIONAL_B_SPLINE_SURFACE ( (
 ( 1.000000000000000000, 0.9238795325112867385, 1.000000000000000000, 0.9238795325112867385, 1.000000000000000000, 0.9238795325112867385, 1.000000000000000000, 0.9238795325112867385, 1.000000000000000000, 0.9238795325112867385, 1.000000000000000000, 0.9238795325112867385, 1.000000000000000000, 0.9238795325112867385, 1.000000000000000000, 0.9238795325112867385, 1.000000000000000000, 0.9238795325112867385, 1.000000000000000000, 0.9238795325112867385, 1.000000000000000000, 0.9238795325112867385, 1.000000000000000000, 0.9238795325112867385, 1.000000000000000000, 0.9238795325112867385, 1.000000000000000000, 0.9238795325112867385, 1.000000000000000000, 0.9238795325112867385, 1.000000000000000000, 0.9238795325112867385, 1.000000000000000000, 0.9238795325112867385, 1.000000000000000000, 0.9238795325112867385, 1.000000000000000000, 0.9238795325112867385, 1.000000000000000000, 0.9238795325112867385, 1.000000000000000000, 0.9238795325112867385, 1.000000000000000000, 0.9238795325112867385, 1.000000000000000000, 0.9238795325112867385, 1.000000000000000000, 0.9238795325112867385, 1.000000000000000000, 0.9238795325112867385, 1.000000000000000000, 0.9238795325112867385, 1.000000000000000000, 0.9238795325112867385, 1.000000000000000000, 0.9238795325112867385, 1.000000000000000000, 0.9238795325112867385, 1.000000000000000000, 0.9238795325112867385, 1.000000000000000000, 0.9238795325112867385, 1.000000000000000000, 0.9238795325112867385, 1.000000000000000000, 0.9238795325112867385, 1.000000000000000000, 0.9238795325112867385, 1.000000000000000000, 0.9238795325112867385, 1.000000000000000000, 0.9238795325112867385, 1.000000000000000000, 0.9238795325112867385, 1.000000000000000000, 0.9238795325112867385, 1.000000000000000000, 0.9238795325112867385, 1.000000000000000000, 0.9238795325112867385, 1.000000000000000000, 0.9238795325112867385, 1.000000000000000000, 0.9238795325112867385, 1.000000000000000000, 0.9238795325112867385, 1.000000000000000000, 0.9238795325112867385, 1.000000000000000000, 0.9238795325112867385, 1.000000000000000000, 0.9238795325112867385, 1.000000000000000000, 0.9238795325112867385, 1.000000000000000000, 0.9238795325112867385, 1.000000000000000000, 0.9238795325112867385, 1.000000000000000000, 0.9238795325112867385, 1.000000000000000000, 0.9238795325112867385, 1.000000000000000000, 0.9238795325112867385, 1.000000000000000000, 0.9238795325112867385, 1.000000000000000000, 0.9238795325112867385, 1.000000000000000000, 0.9238795325112867385, 1.000000000000000000, 0.9238795325112867385, 1.000000000000000000, 0.9238795325112867385, 1.000000000000000000, 0.9238795325112867385, 1.000000000000000000, 0.9238795325112867385, 1.000000000000000000, 0.9238795325112867385, 1.000000000000000000, 0.9238795325112867385, 1.000000000000000000, 0.9238795325112867385, 1.000000000000000000, 0.9238795325112867385, 1.000000000000000000, 0.9238795325112867385, 1.000000000000000000, 0.9238795325112867385, 1.000000000000000000, 0.9238795325112867385, 1.000000000000000000, 0.9238795325112867385, 1.000000000000000000, 0.9238795325112867385, 1.000000000000000000, 0.9238795325112867385, 1.000000000000000000, 0.9238795325112867385, 1.000000000000000000, 0.9238795325112867385, 1.000000000000000000, 0.9238795325112867385, 1.000000000000000000, 0.9238795325112867385, 1.000000000000000000, 0.9238795325112867385, 1.000000000000000000, 0.9238795325112867385, 1.000000000000000000, 0.9238795325112867385, 1.000000000000000000, 0.9238795325112867385, 1.000000000000000000, 0.9238795325112867385, 1.000000000000000000, 0.9238795325112867385, 1.000000000000000000, 0.9238795325112867385, 1.000000000000000000, 0.9238795325112867385, 1.000000000000000000, 0.9238795325112867385, 1.000000000000000000, 0.9238795325112867385, 1.000000000000000000, 0.9238795325112867385, 1.000000000000000000, 0.9238795325112867385, 1.000000000000000000, 0.9238795325112867385, 1.000000000000000000, 0.9238795325112867385, 1.000000000000000000, 0.9238795325112867385, 1.000000000000000000, 0.9238795325112867385, 1.000000000000000000, 0.9238795325112867385, 1.000000000000000000, 0.9238795325112867385, 1.000000000000000000, 0.9238795325112867385, 1.000000000000000000, 0.9238795325112867385, 1.000000000000000000, 0.9238795325112867385, 1.000000000000000000, 0.9238795325112867385, 1.000000000000000000, 0.9238795325112867385, 1.000000000000000000, 0.9238795325112867385, 1.000000000000000000, 0.9238795325112867385, 1.000000000000000000, 0.9238795325112867385, 1.000000000000000000, 0.9238795325112867385, 1.000000000000000000, 0.9238795325112867385, 1.000000000000000000, 0.9238795325112867385, 1.000000000000000000, 0.9238795325112867385, 1.000000000000000000, 0.9238795325112867385, 1.000000000000000000, 0.9238795325112867385, 1.000000000000000000, 0.9238795325112867385, 1.000000000000000000, 0.9238795325112867385, 1.000000000000000000, 0.9238795325112867385, 1.000000000000000000, 0.9238795325112867385, 1.000000000000000000, 0.9238795325112867385, 1.000000000000000000, 0.9238795325112867385, 1.000000000000000000, 0.9238795325112867385, 1.000000000000000000, 0.9238795325112867385, 1.000000000000000000, 0.9238795325112867385, 1.000000000000000000, 0.9238795325112867385, 1.000000000000000000, 0.9238795325112867385, 1.000000000000000000, 0.9238795325112867385, 1.000000000000000000, 0.9238795325112867385, 1.000000000000000000, 0.9238795325112867385, 1.000000000000000000, 0.9238795325112867385, 1.000000000000000000, 0.9238795325112867385, 1.000000000000000000, 0.9238795325112867385, 1.000000000000000000, 0.9238795325112867385, 1.000000000000000000, 0.9238795325112867385, 1.000000000000000000),
 ( 1.000000000000000000, 0.9238795325112867385, 1.000000000000000000, 0.9238795325112867385, 1.000000000000000000, 0.9238795325112867385, 1.000000000000000000, 0.9238795325112867385, 1.000000000000000000, 0.9238795325112867385, 1.000000000000000000, 0.9238795325112867385, 1.000000000000000000, 0.9238795325112867385, 1.000000000000000000, 0.9238795325112867385, 1.000000000000000000, 0.9238795325112867385, 1.000000000000000000, 0.9238795325112867385, 1.000000000000000000, 0.9238795325112867385, 1.000000000000000000, 0.9238795325112867385, 1.000000000000000000, 0.9238795325112867385, 1.000000000000000000, 0.9238795325112867385, 1.000000000000000000, 0.9238795325112867385, 1.000000000000000000, 0.9238795325112867385, 1.000000000000000000, 0.9238795325112867385, 1.000000000000000000, 0.9238795325112867385, 1.000000000000000000, 0.9238795325112867385, 1.000000000000000000, 0.9238795325112867385, 1.000000000000000000, 0.9238795325112867385, 1.000000000000000000, 0.9238795325112867385, 1.000000000000000000, 0.9238795325112867385, 1.000000000000000000, 0.9238795325112867385, 1.000000000000000000, 0.9238795325112867385, 1.000000000000000000, 0.9238795325112867385, 1.000000000000000000, 0.9238795325112867385, 1.000000000000000000, 0.9238795325112867385, 1.000000000000000000, 0.9238795325112867385, 1.000000000000000000, 0.9238795325112867385, 1.000000000000000000, 0.9238795325112867385, 1.000000000000000000, 0.9238795325112867385, 1.000000000000000000, 0.9238795325112867385, 1.000000000000000000, 0.9238795325112867385, 1.000000000000000000, 0.9238795325112867385, 1.000000000000000000, 0.9238795325112867385, 1.000000000000000000, 0.9238795325112867385, 1.000000000000000000, 0.9238795325112867385, 1.000000000000000000, 0.9238795325112867385, 1.000000000000000000, 0.9238795325112867385, 1.000000000000000000, 0.9238795325112867385, 1.000000000000000000, 0.9238795325112867385, 1.000000000000000000, 0.9238795325112867385, 1.000000000000000000, 0.9238795325112867385, 1.000000000000000000, 0.9238795325112867385, 1.000000000000000000, 0.9238795325112867385, 1.000000000000000000, 0.9238795325112867385, 1.000000000000000000, 0.9238795325112867385, 1.000000000000000000, 0.9238795325112867385, 1.000000000000000000, 0.9238795325112867385, 1.000000000000000000, 0.9238795325112867385, 1.000000000000000000, 0.9238795325112867385, 1.000000000000000000, 0.9238795325112867385, 1.000000000000000000, 0.9238795325112867385, 1.000000000000000000, 0.9238795325112867385, 1.000000000000000000, 0.9238795325112867385, 1.000000000000000000, 0.9238795325112867385, 1.000000000000000000, 0.9238795325112867385, 1.000000000000000000, 0.9238795325112867385, 1.000000000000000000, 0.9238795325112867385, 1.000000000000000000, 0.9238795325112867385, 1.000000000000000000, 0.9238795325112867385, 1.000000000000000000, 0.9238795325112867385, 1.000000000000000000, 0.9238795325112867385, 1.000000000000000000, 0.9238795325112867385, 1.000000000000000000, 0.9238795325112867385, 1.000000000000000000, 0.9238795325112867385, 1.000000000000000000, 0.9238795325112867385, 1.000000000000000000, 0.9238795325112867385, 1.000000000000000000, 0.9238795325112867385, 1.000000000000000000, 0.9238795325112867385, 1.000000000000000000, 0.9238795325112867385, 1.000000000000000000, 0.9238795325112867385, 1.000000000000000000, 0.9238795325112867385, 1.000000000000000000, 0.9238795325112867385, 1.000000000000000000, 0.9238795325112867385, 1.000000000000000000, 0.9238795325112867385, 1.000000000000000000, 0.9238795325112867385, 1.000000000000000000, 0.9238795325112867385, 1.000000000000000000, 0.9238795325112867385, 1.000000000000000000, 0.9238795325112867385, 1.000000000000000000, 0.9238795325112867385, 1.000000000000000000, 0.9238795325112867385, 1.000000000000000000, 0.9238795325112867385, 1.000000000000000000, 0.9238795325112867385, 1.000000000000000000, 0.9238795325112867385, 1.000000000000000000, 0.9238795325112867385, 1.000000000000000000, 0.9238795325112867385, 1.000000000000000000, 0.9238795325112867385, 1.000000000000000000, 0.9238795325112867385, 1.000000000000000000, 0.9238795325112867385, 1.000000000000000000, 0.9238795325112867385, 1.000000000000000000, 0.9238795325112867385, 1.000000000000000000, 0.9238795325112867385, 1.000000000000000000, 0.9238795325112867385, 1.000000000000000000, 0.9238795325112867385, 1.000000000000000000, 0.9238795325112867385, 1.000000000000000000, 0.9238795325112867385, 1.000000000000000000, 0.9238795325112867385, 1.000000000000000000, 0.9238795325112867385, 1.000000000000000000, 0.9238795325112867385, 1.000000000000000000, 0.9238795325112867385, 1.000000000000000000, 0.9238795325112867385, 1.000000000000000000, 0.9238795325112867385, 1.000000000000000000, 0.9238795325112867385, 1.000000000000000000, 0.9238795325112867385, 1.000000000000000000, 0.9238795325112867385, 1.000000000000000000, 0.9238795325112867385, 1.000000000000000000, 0.9238795325112867385, 1.000000000000000000, 0.9238795325112867385, 1.000000000000000000, 0.9238795325112867385, 1.000000000000000000, 0.9238795325112867385, 1.000000000000000000, 0.9238795325112867385, 1.000000000000000000, 0.9238795325112867385, 1.000000000000000000, 0.9238795325112867385, 1.000000000000000000, 0.9238795325112867385, 1.000000000000000000, 0.9238795325112867385, 1.000000000000000000, 0.9238795325112867385, 1.000000000000000000, 0.9238795325112867385, 1.000000000000000000, 0.9238795325112867385, 1.000000000000000000, 0.9238795325112867385, 1.000000000000000000, 0.9238795325112867385, 1.000000000000000000, 0.9238795325112867385, 1.000000000000000000, 0.9238795325112867385, 1.000000000000000000) ) ) 
 REPRESENTATION_ITEM ( '' )  SURFACE ( )  );
#3008 = ORIENTED_EDGE ( 'NONE', *, *, #7985, .T. ) ;
#3009 = CARTESIAN_POINT ( 'NONE',  ( 5.196152422706629359, 3.000000000000002665, -179.0386751345948255 ) ) ;
#3010 = CARTESIAN_POINT ( 'NONE',  ( -0.07568246969667169477, -14.85893693147072447, -8.149031565298297863 ) ) ;
#3011 = CIRCLE ( 'NONE', #10378, 5.999999999999999112 ) ;
#3012 = CARTESIAN_POINT ( 'NONE',  ( 119.8752832217623450, -1.849990392679523588, 0.000000000000000000 ) ) ;
#3013 = VERTEX_POINT ( 'NONE', #26956 ) ;
#3014 = ORIENTED_EDGE ( 'NONE', *, *, #8120, .T. ) ;
#3015 = VECTOR ( 'NONE', #25712, 1000.000000000000000 ) ;
#3016 = EDGE_CURVE ( 'NONE', #7376, #4225, #13199, .T. ) ;
#3017 = ADVANCED_BREP_SHAPE_REPRESENTATION ( '', ( #24254, #18805 ), #12447 ) ;
#3018 = CARTESIAN_POINT ( 'NONE',  ( -2.775557561562891351E-14, -5.500000000000115463, -104.2500000000000142 ) ) ;
#3019 = CARTESIAN_POINT ( 'NONE',  ( 16.81250000000011013, -2.649519052838178457, 1.097466725451499370 ) ) ;
#3020 = CARTESIAN_POINT ( 'NONE',  ( -3.608439182435052128, -6.250000000000110134, -121.3080127018921957 ) ) ;
#3021 = ORIENTED_EDGE ( 'NONE', *, *, #28436, .F. ) ;
#3022 = CARTESIAN_POINT ( 'NONE',  ( -5.999999999999963585, -1.487416814333745711E-14, -118.4136751345948255 ) ) ;
#3023 = CARTESIAN_POINT ( 'NONE',  ( 2.775557561562891351E-14, -6.250000000000061284, -157.8169872981078470 ) ) ;
#3024 = CARTESIAN_POINT ( 'NONE',  ( 135.0000000000000284, -7.065583442230452427, 8.449385501354864658 ) ) ;
#3025 = CARTESIAN_POINT ( 'NONE',  ( 134.4226497308104058, 5.000000000000004441, 0.000000000000000000 ) ) ;
#3026 = CIRCLE ( 'NONE', #21218, 0.4999999999999993894 ) ;
#3027 = CARTESIAN_POINT ( 'NONE',  ( -3.608439182435115633, 6.249999999999965361, -57.30801270189221697 ) ) ;
#3028 = ORIENTED_EDGE ( 'NONE', *, *, #8081, .F. ) ;
#3029 = DIRECTION ( 'NONE',  ( 1.000000000000000000, -5.551115123125773458E-17, -1.260129944081490338E-35 ) ) ;
#3030 = EDGE_CURVE ( 'NONE', #26278, #3569, #25738, .T. ) ;
#3031 = CARTESIAN_POINT ( 'NONE',  ( -1.384933631640781648, 10.91424797897492560, -19.15860252534411146 ) ) ;
#3032 = CARTESIAN_POINT ( 'NONE',  ( 6.000000000000000888, 7.762456499804234384E-14, -138.0863248654051745 ) ) ;
#3033 = CARTESIAN_POINT ( 'NONE',  ( -3.175426480542816510, 5.499999999999865885, -178.3750000000000568 ) ) ;
#3034 = CARTESIAN_POINT ( 'NONE',  ( 119.0624999999998295, 2.500000000000024425, 1.035533905932809473 ) ) ;
#3035 = CYLINDRICAL_SURFACE ( 'NONE', #15215, 2.499999999999999112 ) ;
#3036 = CARTESIAN_POINT ( 'NONE',  ( 5.412658773652712085, -3.125000000000086153, -167.4330127018922667 ) ) ;
#3037 = CARTESIAN_POINT ( 'NONE',  ( 155.1636751345948255, 0.000000000000000000, 5.500000000000005329 ) ) ;
#3038 = CARTESIAN_POINT ( 'NONE',  ( 23.43750000000010303, -1.999999999999851674, 0.8284271247462955401 ) ) ;
#3039 = CARTESIAN_POINT ( 'NONE',  ( -4.763139720814407951, 2.749999999999946709, -119.7500000000000284 ) ) ;
#3040 = CARTESIAN_POINT ( 'NONE',  ( -3.464101615137725076, 5.999999999999979572, -84.16367513459481131 ) ) ;
#3041 = CARTESIAN_POINT ( 'NONE',  ( 4.763139720814407951, 2.750000000000002665, -112.7500000000000142 ) ) ;
#3042 = CARTESIAN_POINT ( 'NONE',  ( -9.999999999999793943, 9.000000000000007105, 3.000000000000002665 ) ) ;
#3043 = CARTESIAN_POINT ( 'NONE',  ( -5.999999999999971578, 1.607695154586715303, -88.48066243270262987 ) ) ;
#3044 = ORIENTED_EDGE ( 'NONE', *, *, #4067, .T. ) ;
#3045 = CARTESIAN_POINT ( 'NONE',  ( 17.75000000000018119, 1.873492889145067508, 1.873492889144734441 ) ) ;
#3046 = CARTESIAN_POINT ( 'NONE',  ( 120.5624999999997442, -2.499999999999964473, -1.035533905932508825 ) ) ;
#3047 = CARTESIAN_POINT ( 'NONE',  ( -4.999999999999990230, -24.99999999999999289, -8.000000000000007105 ) ) ;
#3048 = ORIENTED_EDGE ( 'NONE', *, *, #16099, .T. ) ;
#3049 = CARTESIAN_POINT ( 'NONE',  ( -20.99999999999998224, -54.99999999999990763, 5.000000000000004441 ) ) ;
#3050 = CARTESIAN_POINT ( 'NONE',  ( -3.175426480542816066, -5.500000000000057732, -179.3750000000000568 ) ) ;
#3051 = EDGE_LOOP ( 'NONE', ( #14605, #23100, #26807, #9998 ) ) ;
#3052 = CARTESIAN_POINT ( 'NONE',  ( 115.7113248654050466, 2.000000000000112799, 0.000000000000000000 ) ) ;
#3053 = VERTEX_POINT ( 'NONE', #28024 ) ;
#3054 = ORIENTED_EDGE ( 'NONE', *, *, #9514, .T. ) ;
#3055 = CARTESIAN_POINT ( 'NONE',  ( 0.000000000000000000, 5.999999999999977796, -85.21132486540523132 ) ) ;
#3056 = CARTESIAN_POINT ( 'NONE',  ( 133.7023502691896510, 0.000000000000000000, -5.000000000000004441 ) ) ;
#3057 = EDGE_CURVE ( 'NONE', #15338, #12734, #21000, .T. ) ;
#3058 = ORIENTED_EDGE ( 'NONE', *, *, #22847, .F. ) ;
#3059 = CARTESIAN_POINT ( 'NONE',  ( -3.608439182435052128, -6.250000000000110134, -130.9419872981078470 ) ) ;
#3060 = LINE ( 'NONE', #26114, #29914 ) ;
#3061 = CARTESIAN_POINT ( 'NONE',  ( 5.999999999999949374, 1.607695154586804565, -50.09668783648704249 ) ) ;
#3062 = CYLINDRICAL_SURFACE ( 'NONE', #17718, 6.000000000000000888 ) ;
#3063 = VERTEX_POINT ( 'NONE', #13495 ) ;
#3064 = CARTESIAN_POINT ( 'NONE',  ( 15.06250000000016165, 2.000000000000151879, 0.8284271247461152399 ) ) ;
#3065 = EDGE_CURVE ( 'NONE', #23806, #13194, #27318, .T. ) ;
#3066 = CARTESIAN_POINT ( 'NONE',  ( -5.196152422706573404, -3.000000000000002665, -92.21132486540523132 ) ) ;
#3067 = CARTESIAN_POINT ( 'NONE',  ( 0.000000000000000000, 0.000000000000000000, 0.000000000000000000 ) ) ;
#3068 = EDGE_CURVE ( 'NONE', #14517, #16677, #19282, .T. ) ;
#3069 = CARTESIAN_POINT ( 'NONE',  ( 136.6726497308104058, -5.000000000000004441, 0.000000000000000000 ) ) ;
#3070 = CARTESIAN_POINT ( 'NONE',  ( -5.999999999999971578, 1.607695154586715303, -92.40331216351296462 ) ) ;
#3071 = DIRECTION ( 'NONE',  ( -7.147005652999508048E-36, 5.642372883946980038E-36, 1.000000000000000000 ) ) ;
#3072 = DIRECTION ( 'NONE',  ( -7.147005652999508048E-36, 5.642372883946980038E-36, 1.000000000000000000 ) ) ;
#3073 = CARTESIAN_POINT ( 'NONE',  ( 6.000000000000000888, 1.743066579297358182E-13, -56.16367513459481842 ) ) ;
#3074 = CARTESIAN_POINT ( 'NONE',  ( -5.999999999999956479, -1.607695154586745057, -143.2693375672974696 ) ) ;
#3075 = CARTESIAN_POINT ( 'NONE',  ( 3.175426480543072749, 5.499999999999865885, -133.6250000000000284 ) ) ;
#3076 = AXIS2_PLACEMENT_3D ( 'NONE', #3148, #19322, #7615 ) ;
#3077 = VERTEX_POINT ( 'NONE', #27410 ) ;
#3078 = CARTESIAN_POINT ( 'NONE',  ( 0.000000000000000000, 5.499999999999991118, -49.49999999999998579 ) ) ;
#3079 = CARTESIAN_POINT ( 'NONE',  ( 161.0000000000000284, 1.469576158976823947E-15, 12.00000000000000178 ) ) ;
#3080 = MECHANICAL_DESIGN_GEOMETRIC_PRESENTATION_REPRESENTATION (  '', ( #11964 ), #7020 ) ;
#3081 = ORIENTED_EDGE ( 'NONE', *, *, #15845, .F. ) ;
#3082 = CARTESIAN_POINT ( 'NONE',  ( 119.5622167782373708, 1.849990392679621953, -0.7662911109075283278 ) ) ;
#3083 = CARTESIAN_POINT ( 'NONE',  ( -3.608439182435052128, -6.250000000000110134, -91.94198729810786119 ) ) ;
#3084 = CARTESIAN_POINT ( 'NONE',  ( -3.464101615137757051, -5.999999999999979572, -78.58632486540523132 ) ) ;
#3085 = CARTESIAN_POINT ( 'NONE',  ( 112.4999999999999147, -2.499999999999835687, 0.000000000000000000 ) ) ;
#3086 = ADVANCED_FACE ( 'NONE', ( #6376 ), #9310, .T. ) ;
#3087 = CARTESIAN_POINT ( 'NONE',  ( -6.350852961085760029, -1.281975124255709124E-13, -133.1250000000000284 ) ) ;
#3088 =( BOUNDED_CURVE ( )  B_SPLINE_CURVE ( 2, ( #25106, #6224, #13485, #15643, #18087, #15485, #5905, #20515, #3760 ),
 .UNSPECIFIED., .F., .T. ) 
 B_SPLINE_CURVE_WITH_KNOTS ( ( 3, 2, 2, 2, 3 ),
 ( 0.5750000000000000666, 0.5759259259259259522, 0.5777777777777777235, 0.5796296296296296058, 0.5805555555555554914 ),
 .UNSPECIFIED. ) 
 CURVE ( )  GEOMETRIC_REPRESENTATION_ITEM ( )  RATIONAL_B_SPLINE_CURVE ( ( 0.9330127018922194093, 0.9330127018922234061, 1.000000000000000000, 0.8660254037844388186, 1.000000000000000000, 0.8660254037844388186, 1.000000000000000000, 0.9330127018922234061, 0.9330127018922194093 ) ) 
 REPRESENTATION_ITEM ( '' )  );
#3089 = VECTOR ( 'NONE', #4789, 1000.000000000000000 ) ;
#3090 = VERTEX_POINT ( 'NONE', #13649 ) ;
#3091 = VECTOR ( 'NONE', #14746, 1000.000000000000000 ) ;
#3092 = CARTESIAN_POINT ( 'NONE',  ( 5.196152422706629359, -2.999999999999988898, -82.71132486540521711 ) ) ;
#3093 = CARTESIAN_POINT ( 'NONE',  ( -3.175426480542816510, -5.500000000000057732, -59.37500000000005684 ) ) ;
#3094 = CARTESIAN_POINT ( 'NONE',  ( -5.999999999999963585, -1.487416814333745711E-14, -101.9136751345948397 ) ) ;
#3095 = CARTESIAN_POINT ( 'NONE',  ( 6.000000000000000888, 1.743066579297358182E-13, -62.16367513459481131 ) ) ;
#3096 = EDGE_CURVE ( 'NONE', #2061, #14641, #6515, .T. ) ;
#3097 = CARTESIAN_POINT ( 'NONE',  ( 5.412658773652739619, 3.124999999999988898, -74.18301270189225249 ) ) ;
#3098 = PRODUCT_DEFINITION_FORMATION_WITH_SPECIFIED_SOURCE ( 'ANY', '', #30020, .NOT_KNOWN. ) ;
#3099 = DIRECTION ( 'NONE',  ( 1.000000000000000000, 0.000000000000000000, 0.000000000000000000 ) ) ;
#3100 = DIRECTION ( 'NONE',  ( -7.147005652999508048E-36, 5.642372883946980038E-36, 1.000000000000000000 ) ) ;
#3101 = LINE ( 'NONE', #12674, #16794 ) ;
#3102 = CARTESIAN_POINT ( 'NONE',  ( 114.2502832217621602, 1.308140751793640533, -1.308140751793640533 ) ) ;
#3103 = CARTESIAN_POINT ( 'NONE',  ( -4.763139720814407951, -2.750000000000016431, -142.0000000000000284 ) ) ;
#3104 = CARTESIAN_POINT ( 'NONE',  ( 140.0546052829554071, -9.478432856838029608, 7.360605440459326410 ) ) ;
#3105 = CARTESIAN_POINT ( 'NONE',  ( -3.608439182435115633, 6.249999999999965361, -156.3080127018922383 ) ) ;
#3106 = CARTESIAN_POINT ( 'NONE',  ( 140.0699251345947971, 2.278174593052322283, 5.499999999999701572 ) ) ;
#3107 = CARTESIAN_POINT ( 'NONE',  ( 146.8050748654052313, 5.500000000000012434, 2.278174593052012309 ) ) ;
#3108 = CARTESIAN_POINT ( 'NONE',  ( -4.763139720814407951, -2.750000000000016431, -71.50000000000001421 ) ) ;
#3109 = CARTESIAN_POINT ( 'NONE',  ( 6.000000000000000888, 1.743066579297358182E-13, -104.1636751345948397 ) ) ;
#3110 = CARTESIAN_POINT ( 'NONE',  ( -6.350852961085760029, -1.281975124255709124E-13, -59.62500000000000000 ) ) ;
#3111 = CARTESIAN_POINT ( 'NONE',  ( -5.999999999999963585, 1.780251999655701777E-13, -53.33632486540522422 ) ) ;
#3112 = ORIENTED_EDGE ( 'NONE', *, *, #25964, .F. ) ;
#3113 = CARTESIAN_POINT ( 'NONE',  ( 141.6711002691896795, 4.999999999999989342, 2.071067811865468400 ) ) ;
#3114 = VECTOR ( 'NONE', #27005, 1000.000000000000000 ) ;
#3115 = CARTESIAN_POINT ( 'NONE',  ( 150.2812500000000284, 2.485281374238585972, 6.000000000000005329 ) ) ;
#3116 = DIRECTION ( 'NONE',  ( 1.387778780781521564E-14, -1.000000000000000000, 0.000000000000000000 ) ) ;
#3117 = CARTESIAN_POINT ( 'NONE',  ( 13.75000000000006750, 2.220446049250313081E-13, -2.000000000000001776 ) ) ;
#3118 = CLOSED_SHELL ( 'NONE', ( #27297, #16480, #4324, #11762, #15815, #460, #22447, #20192, #29348, #11691, #20753, #3993, #7311, #18109, #15673, #23345, #23384, #9993, #10570, #2425, #6503, #4560, #19088, #11359, #2103, #23683, #10066, #7714, #3329, #6432, #15990, #1973, #11478, #2924, #10844, #28411, #17418, #1004, #9611, #18567, #27710, #16544, #5718, #26824, #13035 ) ) ;
#3119 = CYLINDRICAL_SURFACE ( 'NONE', #17544, 2.000000000000012879 ) ;
#3120 = CARTESIAN_POINT ( 'NONE',  ( 115.3747167782374987, -5.551115123125782702E-14, -1.849990392679523588 ) ) ;
#3121 = ORIENTED_EDGE ( 'NONE', *, *, #22620, .F. ) ;
#3122 = CARTESIAN_POINT ( 'NONE',  ( 142.0312500000000284, -2.485281374238555774, -6.000000000000005329 ) ) ;
#3123 = EDGE_CURVE ( 'NONE', #22623, #8626, #2402, .T. ) ;
#3124 = ADVANCED_FACE ( 'NONE', ( #4380 ), #27557, .T. ) ;
#3125 = CARTESIAN_POINT ( 'NONE',  ( -4.763139720814407951, -2.750000000000016431, -178.0000000000000568 ) ) ;
#3126 = CARTESIAN_POINT ( 'NONE',  ( 16.50000000000004263, -1.999999999999835243, 0.000000000000000000 ) ) ;
#3127 = CARTESIAN_POINT ( 'NONE',  ( 5.412658773652712085, -3.125000000000086153, -153.0669872981078470 ) ) ;
#3128 = ORIENTED_EDGE ( 'NONE', *, *, #13890, .F. ) ;
#3129 = CARTESIAN_POINT ( 'NONE',  ( 0.000000000000000000, 5.499999999999991118, -78.00000000000001421 ) ) ;
#3130 = CARTESIAN_POINT ( 'NONE',  ( 3.608439182435180470, 6.249999999999982236, -102.5580127018922383 ) ) ;
#3131 = VERTEX_POINT ( 'NONE', #25256 ) ;
#3132 = CYLINDRICAL_SURFACE ( 'NONE', #531, 2.499999999999999112 ) ;
#3133 = FACE_OUTER_BOUND ( 'NONE', #17440, .T. ) ;
#3134 = CARTESIAN_POINT ( 'NONE',  ( 3.027755249632174461, -10.58056329815971175, -19.80527582512398155 ) ) ;
#3135 = LINE ( 'NONE', #19887, #4881 ) ;
#3136 = FACE_OUTER_BOUND ( 'NONE', #1711, .T. ) ;
#3137 = CARTESIAN_POINT ( 'NONE',  ( -3.175426480542816066, -5.500000000000057732, -165.8750000000000568 ) ) ;
#3138 = CARTESIAN_POINT ( 'NONE',  ( 160.9761751345948255, 3.889087296526011706, 3.889087296526011706 ) ) ;
#3139 = CARTESIAN_POINT ( 'NONE',  ( -6.350852961085760029, -1.281975124255709124E-13, -146.6250000000000284 ) ) ;
#3140 = FACE_OUTER_BOUND ( 'NONE', #8232, .T. ) ;
#3141 = CARTESIAN_POINT ( 'NONE',  ( 148.9613248654052029, -5.500000000000005329, 0.000000000000000000 ) ) ;
#3142 = CARTESIAN_POINT ( 'NONE',  ( 4.763139720814407951, -2.749999999999988454, -95.00000000000002842 ) ) ;
#3143 = FILL_AREA_STYLE ('',( #12718 ) ) ;
#3144 = CARTESIAN_POINT ( 'NONE',  ( 6.350852961086080661, -9.614813431917819062E-14, -78.37500000000001421 ) ) ;
#3145 = CARTESIAN_POINT ( 'NONE',  ( 3.464101615137852974, 5.999999999999884537, -143.8363248654052029 ) ) ;
#3146 = CARTESIAN_POINT ( 'NONE',  ( 9.500000000000092371, 1.873492889145067508, -1.873492889145011997 ) ) ;
#3147 = CARTESIAN_POINT ( 'NONE',  ( 109.4999999999998579, -2.499999999999891198, 2.220446049250313081E-13 ) ) ;
#3148 = CARTESIAN_POINT ( 'NONE',  ( 0.000000000000000000, 0.000000000000000000, 0.000000000000000000 ) ) ;
#3149 = FILL_AREA_STYLE ('',( #714 ) ) ;
#3150 = CARTESIAN_POINT ( 'NONE',  ( 161.0086076262249151, 3.226123241052607060, 4.476387269555026194 ) ) ;
#3151 = ORIENTED_EDGE ( 'NONE', *, *, #19399, .T. ) ;
#3152 = CARTESIAN_POINT ( 'NONE',  ( 160.5000000000000284, 6.000000000000005329, 0.000000000000000000 ) ) ;
#3153 = DIRECTION ( 'NONE',  ( 1.000000000000000000, -0.000000000000000000, -0.000000000000000000 ) ) ;
#3154 = CARTESIAN_POINT ( 'NONE',  ( 124.9999999999999432, -71.00000000000001421, -4.000000000000003553 ) ) ;
#3155 = CARTESIAN_POINT ( 'NONE',  ( 104.1872167782373708, -1.849990392679351725, -0.7662911109074682647 ) ) ;
#3156 = COLOUR_RGB ( '', 0.08235294, 0.09019608, 0.10196078) ;
#3157 = ORIENTED_EDGE ( 'NONE', *, *, #5433, .T. ) ;
#3158 = EDGE_CURVE ( 'NONE', #28288, #22958, #20397, .T. ) ;
#3159 = CARTESIAN_POINT ( 'NONE',  ( 146.6250000000000284, 0.000000000000000000, -6.000000000000005329 ) ) ;
#3160 = ORIENTED_EDGE ( 'NONE', *, *, #14682, .F. ) ;
#3161 = CARTESIAN_POINT ( 'NONE',  ( 4.763139720814407951, -2.749999999999988454, -102.5000000000000284 ) ) ;
#3162 = CARTESIAN_POINT ( 'NONE',  ( 20.43750000000011369, 2.649519052838478661, 1.097466725451499370 ) ) ;
#3163 = CARTESIAN_POINT ( 'NONE',  ( -5.412658773652739619, 3.124999999999975131, -126.1830127018922525 ) ) ;
#3164 = ORIENTED_EDGE ( 'NONE', *, *, #18341, .F. ) ;
#3165 = CARTESIAN_POINT ( 'NONE',  ( 113.8363248654050892, 1.414213562373145550, 1.414213562373034527 ) ) ;
#3166 = CARTESIAN_POINT ( 'NONE',  ( 7.216878364870455975, -6.409875621278545621E-14, -160.4419872981077901 ) ) ;
#3167 = CARTESIAN_POINT ( 'NONE',  ( 105.1874999999998437, 1.035533905932749299, 2.500000000000265121 ) ) ;
#3168 = CIRCLE ( 'NONE', #23811, 0.5000000000000004441 ) ;
#3169 = CIRCLE ( 'NONE', #22826, 14.99999999999998579 ) ;
#3170 = CARTESIAN_POINT ( 'NONE',  ( 3.608439182435180470, 6.249999999999982236, -62.05801270189223828 ) ) ;
#3171 = ORIENTED_EDGE ( 'NONE', *, *, #23133, .F. ) ;
#3172 = FACE_OUTER_BOUND ( 'NONE', #24288, .T. ) ;
#3173 =( BOUNDED_CURVE ( )  B_SPLINE_CURVE ( 2, ( #7581, #12249, #23744, #21285, #28322, #26027, #26317, #26172, #23882 ),
 .UNSPECIFIED., .F., .T. ) 
 B_SPLINE_CURVE_WITH_KNOTS ( ( 3, 2, 2, 2, 3 ),
 ( 0.2694444444444444309, 0.2703703703703703720, 0.2722222222222221988, 0.2740740740740740811, 0.2750000000000000222 ),
 .UNSPECIFIED. ) 
 CURVE ( )  GEOMETRIC_REPRESENTATION_ITEM ( )  RATIONAL_B_SPLINE_CURVE ( ( 0.9330127018922194093, 0.9330127018922174109, 1.000000000000000000, 0.8660254037844388186, 1.000000000000000000, 0.8660254037844388186, 1.000000000000000000, 0.9330127018922174109, 0.9330127018922194093 ) ) 
 REPRESENTATION_ITEM ( '' )  );
#3174 = CARTESIAN_POINT ( 'NONE',  ( -5.999486246981926563, 9.219878802943876295, -25.40874315777524117 ) ) ;
#3175 = PLANE ( 'NONE',  #26084 ) ;
#3176 = CARTESIAN_POINT ( 'NONE',  ( -2.775557561562891351E-14, -5.500000000000115463, -168.7500000000000000 ) ) ;
#3177 = CARTESIAN_POINT ( 'NONE',  ( 120.1874999999997016, 1.035533905932809473, 2.500000000000205169 ) ) ;
#3178 = CARTESIAN_POINT ( 'NONE',  ( -5.196152422706573404, -3.000000000000002665, -113.2113248654051887 ) ) ;
#3179 = CARTESIAN_POINT ( 'NONE',  ( 5.412658773652712085, -3.125000000000086153, -168.9330127018922099 ) ) ;
#3180 = DIRECTION ( 'NONE',  ( 0.000000000000000000, 0.9165151389911677660, 0.4000000000000004663 ) ) ;
#3181 = CARTESIAN_POINT ( 'NONE',  ( 24.06250000000009592, 2.000000000000091926, 0.8284271247461153509 ) ) ;
#3182 = CARTESIAN_POINT ( 'NONE',  ( 3.175426480543072749, -5.500000000000105693, -117.6250000000000284 ) ) ;
#3183 = CARTESIAN_POINT ( 'NONE',  ( -6.350852961085760029, -1.281975124255709124E-13, -103.1250000000000000 ) ) ;
#3184 =( BOUNDED_CURVE ( )  B_SPLINE_CURVE ( 3, ( #22646, #15768, #18359, #29685 ),
 .UNSPECIFIED., .F., .T. ) 
 B_SPLINE_CURVE_WITH_KNOTS ( ( 4, 4 ),
 ( 3.536383773289572652, 4.712388980384689674 ),
 .UNSPECIFIED. ) 
 CURVE ( )  GEOMETRIC_REPRESENTATION_ITEM ( )  RATIONAL_B_SPLINE_CURVE ( ( 1.000000000000000000, 0.8880335295585657374, 0.8880335295585657374, 1.000000000000000000 ) ) 
 REPRESENTATION_ITEM ( '' )  );
#3185 = CARTESIAN_POINT ( 'NONE',  ( 148.4136751345948539, 0.000000000000000000, -5.500000000000005329 ) ) ;
#3186 = ORIENTED_EDGE ( 'NONE', *, *, #20352, .T. ) ;
#3187 = ADVANCED_FACE ( 'NONE', ( #11500 ), #25375, .F. ) ;
#3188 = CARTESIAN_POINT ( 'NONE',  ( 120.9999999999997300, 2.500000000000113243, 3.330669073875469621E-13 ) ) ;
#3189 = DIRECTION ( 'NONE',  ( -0.000000000000000000, -0.000000000000000000, -1.000000000000000000 ) ) ;
#3190 = ORIENTED_EDGE ( 'NONE', *, *, #845, .F. ) ;
#3191 = CARTESIAN_POINT ( 'NONE',  ( 0.000000000000000000, -5.999999999999991118, -127.0386751345948255 ) ) ;
#3192 = CARTESIAN_POINT ( 'NONE',  ( 7.216878364870455975, -6.409875621278545621E-14, -83.94198729810781856 ) ) ;
#3193 = SURFACE_STYLE_USAGE ( .BOTH. , #26685 ) ;
#3194 = CARTESIAN_POINT ( 'NONE',  ( 24.77698899409918809, 1.864818660053481736, -1.235634622128368942 ) ) ;
#3195 = EDGE_CURVE ( 'NONE', #25601, #18584, #29039, .T. ) ;
#3196 = VERTEX_POINT ( 'NONE', #5539 ) ;
#3197 = CARTESIAN_POINT ( 'NONE',  ( 133.2336002691896510, -4.999999999999989342, 2.071067811865468400 ) ) ;
#3198 = ORIENTED_EDGE ( 'NONE', *, *, #30089, .F. ) ;
#3199 = AXIS2_PLACEMENT_3D ( 'NONE', #29275, #3623, #6098 ) ;
#3200 = CARTESIAN_POINT ( 'NONE',  ( -5.412658773652684552, -3.125000000000099920, -128.0669872981078470 ) ) ;
#3201 = CARTESIAN_POINT ( 'NONE',  ( 0.000000000000000000, 5.999999999999977796, -49.78867513459483973 ) ) ;
#3202 = CARTESIAN_POINT ( 'NONE',  ( 19.08632486540534501, -1.767766952966154381, 1.767766952966376426 ) ) ;
#3203 = VERTEX_POINT ( 'NONE', #16852 ) ;
#3204 = CARTESIAN_POINT ( 'NONE',  ( 17.18750000000013145, 0.8284271247463557142, 1.999999999999971800 ) ) ;
#3205 = CARTESIAN_POINT ( 'NONE',  ( 3.464101615137757051, -5.999999999999979572, -138.9136751345947971 ) ) ;
#3206 = CARTESIAN_POINT ( 'NONE',  ( -5.999999999999963585, 8.134310703387671600E-14, -136.4136751345948255 ) ) ;
#3207 = CARTESIAN_POINT ( 'NONE',  ( 138.4538997308104342, -2.071067811865468400, -4.999999999999989342 ) ) ;
#3208 = CARTESIAN_POINT ( 'NONE',  ( -3.464101615137757051, -5.999999999999979572, -99.58632486540520290 ) ) ;
#3209 = DIRECTION ( 'NONE',  ( -1.000000000000000000, -1.665334536937736783E-16, -2.220446049250315546E-16 ) ) ;
#3210 = AXIS2_PLACEMENT_3D ( 'NONE', #10135, #7366, #19504 ) ;
#3211 = PRESENTATION_STYLE_ASSIGNMENT (( #26419 ) ) ;
#3212 = FILL_AREA_STYLE ('',( #24262 ) ) ;
#3213 = CARTESIAN_POINT ( 'NONE',  ( 106.4374999999997442, -2.499999999999994671, 1.035533905932989551 ) ) ;
#3214 = CARTESIAN_POINT ( 'NONE',  ( 6.000000000000000888, 7.762456499804234384E-14, -128.1636751345948539 ) ) ;
#3215 = DIRECTION ( 'NONE',  ( 1.000000000000000000, -5.551115123125773458E-17, -1.260129944081490338E-35 ) ) ;
#3216 = VERTEX_POINT ( 'NONE', #15100 ) ;
#3217 = CARTESIAN_POINT ( 'NONE',  ( 0.000000000000000000, 5.999999999999977796, -173.7113248654052029 ) ) ;
#3218 = EDGE_CURVE ( 'NONE', #21999, #14866, #18853, .T. ) ;
#3219 = CARTESIAN_POINT ( 'NONE',  ( 6.350852961086080661, -9.614813431917819062E-14, -49.87500000000000711 ) ) ;
#3220 = CARTESIAN_POINT ( 'NONE',  ( 1101.535898384862321, 1.665334536937736830E-13, 2.220446049250315605E-13 ) ) ;
#3221 = CARTESIAN_POINT ( 'NONE',  ( 112.4136751345946692, 1.414213562373145550, 1.414213562373034527 ) ) ;
#3222 = VERTEX_POINT ( 'NONE', #10332 ) ;
#3223 = CARTESIAN_POINT ( 'NONE',  ( 113.8747167782375556, 0.000000000000000000, 1.849990392679523588 ) ) ;
#3224 = CARTESIAN_POINT ( 'NONE',  ( 135.8437500000000284, -6.000000000000005329, -2.485281374238556218 ) ) ;
#3225 = CARTESIAN_POINT ( 'NONE',  ( 10.62500000000013500, -1.414213562372979016, -1.414213562373090038 ) ) ;
#3226 = AXIS2_PLACEMENT_3D ( 'NONE', #9017, #29737, #16279 ) ;
#3227 = CARTESIAN_POINT ( 'NONE',  ( 3.608439182435180470, 6.249999999999982236, -97.19198729810780435 ) ) ;
#3228 = CARTESIAN_POINT ( 'NONE',  ( 5.196152422706629359, -2.999999999999988898, -50.28867513459483973 ) ) ;
#3229 = EDGE_CURVE ( 'NONE', #22623, #9072, #16562, .T. ) ;
#3230 = CARTESIAN_POINT ( 'NONE',  ( 11.46132486540535389, 1.110223024625156540E-13, -2.500000000000002220 ) ) ;
#3231 = CARTESIAN_POINT ( 'NONE',  ( 115.6874999999997584, -1.035533905932719101, -2.499999999999844569 ) ) ;
#3232 = CARTESIAN_POINT ( 'NONE',  ( 140.2643372958527266, -11.26433729585132681, 4.292342582647273197 ) ) ;
#3233 = AXIS2_PLACEMENT_3D ( 'NONE', #2703, #553, #16882 ) ;
#3234 = CARTESIAN_POINT ( 'NONE',  ( 10.18750000000014033, 0.8284271247463557142, 2.000000000000031530 ) ) ;
#3235 = ORIENTED_EDGE ( 'NONE', *, *, #23025, .T. ) ;
#3236 = CARTESIAN_POINT ( 'NONE',  ( 160.9860723913248819, -11.61453176910477048, 3.019692173012635372 ) ) ;
#3237 = CARTESIAN_POINT ( 'NONE',  ( -6.350852961085760029, -1.281975124255709124E-13, -58.12500000000005684 ) ) ;
#3238 = CARTESIAN_POINT ( 'NONE',  ( 159.6636751345948539, 0.000000000000000000, 5.500000000000005329 ) ) ;
#3239 = CARTESIAN_POINT ( 'NONE',  ( -1.000000000000000888, -9.000000000000007105, 4.000000000000003553 ) ) ;
#3240 = CARTESIAN_POINT ( 'NONE',  ( 0.000000000000000000, 5.999999999999977796, -67.78867513459485394 ) ) ;
#3241 = CARTESIAN_POINT ( 'NONE',  ( 116.4613248654051034, 5.551115123125782702E-14, -2.000000000000001776 ) ) ;
#3242 = CARTESIAN_POINT ( 'NONE',  ( 157.0163997308104058, 4.999999999999989342, 2.071067811865468400 ) ) ;
#3243 = CARTESIAN_POINT ( 'NONE',  ( 0.000000000000000000, 0.000000000000000000, 0.000000000000000000 ) ) ;
#3244 = CIRCLE ( 'NONE', #28275, 0.5000000000000004441 ) ;
#3245 = CARTESIAN_POINT ( 'NONE',  ( -5.999999999999956479, -1.607695154586745057, -168.7693375672974128 ) ) ;
#3246 = DIRECTION ( 'NONE',  ( 0.000000000000000000, 0.000000000000000000, -1.000000000000000000 ) ) ;
#3247 = CARTESIAN_POINT ( 'NONE',  ( 4.763139720814407951, -2.749999999999988454, -143.0000000000000284 ) ) ;
#3248 = CARTESIAN_POINT ( 'NONE',  ( -1.000000000000000888, 9.000000000000007105, 4.000000000000003553 ) ) ;
#3249 = CARTESIAN_POINT ( 'NONE',  ( 7.216878364870455975, -6.409875621278545621E-14, -153.8080127018922099 ) ) ;
#3250 = CARTESIAN_POINT ( 'NONE',  ( 139.4136751345948539, 0.000000000000000000, -5.500000000000005329 ) ) ;
#3251 = CARTESIAN_POINT ( 'NONE',  ( 0.000000000000000000, 5.999999999999977796, -67.21132486540520290 ) ) ;
#3252 = ADVANCED_FACE ( 'NONE', ( #2678 ), #9467, .F. ) ;
#3253 = CARTESIAN_POINT ( 'NONE',  ( 4.763139720814407951, -2.749999999999988454, -74.00000000000001421 ) ) ;
#3254 = CARTESIAN_POINT ( 'NONE',  ( -4.763139720814407951, 2.749999999999946709, -53.75000000000002132 ) ) ;
#3255 = DIRECTION ( 'NONE',  ( -0.000000000000000000, -0.000000000000000000, -1.000000000000000000 ) ) ;
#3256 = VERTEX_POINT ( 'NONE', #229 ) ;
#3257 = CARTESIAN_POINT ( 'NONE',  ( 137.0773502691896510, 5.000000000000004441, 0.000000000000000000 ) ) ;
#3258 = CARTESIAN_POINT ( 'NONE',  ( 154.4062500000000284, 6.000000000000005329, -2.485281374238556218 ) ) ;
#3259 = CARTESIAN_POINT ( 'NONE',  ( 139.5000000000000000, -8.944271909999162773, 8.000000000000007105 ) ) ;
#3260 = CARTESIAN_POINT ( 'NONE',  ( 15.37500000000011013, -1.414213562373034527, 1.414213562373034527 ) ) ;
#3261 = CARTESIAN_POINT ( 'NONE',  ( 0.000000000000000000, -5.999999999999991118, -88.96132486540520290 ) ) ;
#3262 = CARTESIAN_POINT ( 'NONE',  ( 114.2497167782375698, -1.308140751793557266, -1.308140751793640533 ) ) ;
#3263 = ADVANCED_FACE ( 'NONE', ( #19005 ), #28532, .F. ) ;
#3264 =( BOUNDED_CURVE ( )  B_SPLINE_CURVE ( 2, ( #17857, #18151, #29937, #13553, #27621, #8283, #25317, #8602, #4134 ),
 .UNSPECIFIED., .F., .T. ) 
 B_SPLINE_CURVE_WITH_KNOTS ( ( 3, 2, 2, 2, 3 ),
 ( 0.08055555555555556080, 0.08148148148148148806, 0.08333333333333332871, 0.08518518518518518323, 0.08611111111111111049 ),
 .UNSPECIFIED. ) 
 CURVE ( )  GEOMETRIC_REPRESENTATION_ITEM ( )  RATIONAL_B_SPLINE_CURVE ( ( 0.9330127018922194093, 0.9330127018922194093, 1.000000000000000000, 0.8660254037844388186, 1.000000000000000000, 0.8660254037844388186, 1.000000000000000000, 0.9330127018922194093, 0.9330127018922194093 ) ) 
 REPRESENTATION_ITEM ( '' )  );
#3265 = ADVANCED_FACE ( 'NONE', ( #25212 ), #2196, .T. ) ;
#3266 = VERTEX_POINT ( 'NONE', #11600 ) ;
#3267 = CARTESIAN_POINT ( 'NONE',  ( 141.4687500000000568, -2.485281374238585972, 6.000000000000005329 ) ) ;
#3268 = CARTESIAN_POINT ( 'NONE',  ( 142.8675748654052029, -5.500000000000012434, 2.278174593052012309 ) ) ;
#3269 = AXIS2_PLACEMENT_3D ( 'NONE', #15492, #15339, #29254 ) ;
#3270 = CARTESIAN_POINT ( 'NONE',  ( -3.464101615137757051, -5.999999999999979572, -102.5863248654052171 ) ) ;
#3271 = CARTESIAN_POINT ( 'NONE',  ( -3.175426480542816510, -5.500000000000057732, -177.8750000000000568 ) ) ;
#3272 = CIRCLE ( 'NONE', #4254, 14.49999999999999822 ) ;
#3273 = CARTESIAN_POINT ( 'NONE',  ( 17.81250000000015632, 0.8284271247463557142, -2.000000000000091926 ) ) ;
#3274 = CARTESIAN_POINT ( 'NONE',  ( -5.412658773652684552, -3.125000000000099920, -147.5669872981077901 ) ) ;
#3275 = ORIENTED_EDGE ( 'NONE', *, *, #6016, .T. ) ;
#3276 = CARTESIAN_POINT ( 'NONE',  ( -6.350852961085760029, -1.281975124255709124E-13, -85.12499999999998579 ) ) ;
#3277 = CARTESIAN_POINT ( 'NONE',  ( 13.18750000000012967, 1.097466725451619718, -2.649519052838358757 ) ) ;
#3278 = CARTESIAN_POINT ( 'NONE',  ( 5.412658773652739619, 3.124999999999988898, -92.18301270189222407 ) ) ;
#3279 = CARTESIAN_POINT ( 'NONE',  ( -3.464101615137725076, 5.999999999999979572, -175.6636751345948539 ) ) ;
#3280 = VECTOR ( 'NONE', #15350, 1000.000000000000000 ) ;
#3281 = DIRECTION ( 'NONE',  ( 1.000000000000000000, -5.551115123125773458E-17, -1.260129944081490338E-35 ) ) ;
#3282 = CARTESIAN_POINT ( 'NONE',  ( 0.000000000000000000, 9.000000000000007105, -3.000000000000002665 ) ) ;
#3283 = CARTESIAN_POINT ( 'NONE',  ( 135.2991173618607945, -8.337648098118274120, 8.244751738007437325 ) ) ;
#3284 = TOROIDAL_SURFACE ( 'NONE', #1346, 16.50000000000000355, 1.000000000000000000 ) ;
#3285 = CARTESIAN_POINT ( 'NONE',  ( -4.763139720814407951, -2.750000000000016431, -167.4999999999999716 ) ) ;
#3286 = LINE ( 'NONE', #12712, #12391 ) ;
#3287 = CARTESIAN_POINT ( 'NONE',  ( 4.763139720814407951, 2.750000000000002665, -150.2500000000000000 ) ) ;
#3288 = DIRECTION ( 'NONE',  ( 1.000000000000000000, -5.551115123125773458E-17, -1.260129944081490338E-35 ) ) ;
#3289 = EDGE_CURVE ( 'NONE', #8702, #19684, #9255, .T. ) ;
#3290 = CARTESIAN_POINT ( 'NONE',  ( -3.175426480542816066, 5.499999999999865885, -97.37499999999997158 ) ) ;
#3291 = CARTESIAN_POINT ( 'NONE',  ( 142.5863248654052313, 0.000000000000000000, 5.500000000000005329 ) ) ;
#3292 = DIRECTION ( 'NONE',  ( 0.000000000000000000, -1.000000000000000000, 0.000000000000000000 ) ) ;
#3293 = CARTESIAN_POINT ( 'NONE',  ( -3.175426480542816510, 5.499999999999865885, -80.87500000000002842 ) ) ;
#3294 = DIRECTION ( 'NONE',  ( 0.000000000000000000, 5.551115123125767911E-17, -1.000000000000000000 ) ) ;
#3295 = CARTESIAN_POINT ( 'NONE',  ( 151.7961002691896226, 2.071067811865468400, -4.999999999999989342 ) ) ;
#3296 = CARTESIAN_POINT ( 'NONE',  ( 0.000000000000000000, 5.999999999999977796, -64.78867513459485394 ) ) ;
#3297 = CARTESIAN_POINT ( 'NONE',  ( 139.8600870026756695, -9.432236288125531942, -7.851756037878587335 ) ) ;
#3298 = CARTESIAN_POINT ( 'NONE',  ( 0.000000000000000000, 0.000000000000000000, 0.000000000000000000 ) ) ;
#3299 = CARTESIAN_POINT ( 'NONE',  ( -3.464101615137725076, 5.999999999999979572, -128.5863248654052029 ) ) ;
#3300 = CARTESIAN_POINT ( 'NONE',  ( 104.9999999999999432, 2.775557561562891351E-14, 1.110223024625156540E-13 ) ) ;
#3301 = EDGE_CURVE ( 'NONE', #17475, #9162, #15810, .T. ) ;
#3302 = CARTESIAN_POINT ( 'NONE',  ( 0.000000000000000000, 5.999999999999977796, -78.28867513459481131 ) ) ;
#3303 = ORIENTED_EDGE ( 'NONE', *, *, #18154, .T. ) ;
#3304 = CARTESIAN_POINT ( 'NONE',  ( 3.464101615137852974, 5.999999999999884537, -73.33632486540520290 ) ) ;
#3305 = CARTESIAN_POINT ( 'NONE',  ( 3.464101615137852974, 5.999999999999884537, -82.91367513459479710 ) ) ;
#3306 = CARTESIAN_POINT ( 'NONE',  ( 6.000000000000000888, -1.859271017917181981E-14, -115.5863248654052171 ) ) ;
#3307 = CIRCLE ( 'NONE', #1860, 1.000000000000000000 ) ;
#3308 = ORIENTED_EDGE ( 'NONE', *, *, #5000, .T. ) ;
#3309 = CARTESIAN_POINT ( 'NONE',  ( 146.1562500000000853, -6.000000000000005329, 2.485281374238555774 ) ) ;
#3310 = CARTESIAN_POINT ( 'NONE',  ( 3.175426480543072749, 5.499999999999865885, -102.1250000000000142 ) ) ;
#3311 = CARTESIAN_POINT ( 'NONE',  ( 3.608439182435180470, 6.249999999999982236, -119.0580127018922667 ) ) ;
#3312 = ORIENTED_EDGE ( 'NONE', *, *, #1974, .T. ) ;
#3313 = CARTESIAN_POINT ( 'NONE',  ( -3.464101615137757051, -5.999999999999979572, -61.16367513459483263 ) ) ;
#3314 = CARTESIAN_POINT ( 'NONE',  ( -5.412658773652739619, 3.124999999999975131, -159.8169872981078470 ) ) ;
#3315 = CARTESIAN_POINT ( 'NONE',  ( -6.000000000000000888, 1.067854986875958443E-15, 7.560779664488942560E-35 ) ) ;
#3316 =( GEOMETRIC_REPRESENTATION_CONTEXT ( 3 ) GLOBAL_UNCERTAINTY_ASSIGNED_CONTEXT ( ( #22359 ) ) GLOBAL_UNIT_ASSIGNED_CONTEXT ( ( #2079, #8842, #16250 ) ) REPRESENTATION_CONTEXT ( 'NONE', 'WORKASPACE' ) );
#3317 = CARTESIAN_POINT ( 'NONE',  ( 7.216878364870455975, -6.409875621278545621E-14, -62.30801270189223828 ) ) ;
#3318 = VERTEX_POINT ( 'NONE', #15367 ) ;
#3319 = CARTESIAN_POINT ( 'NONE',  ( -5.196152422706601826, 2.999999999999975131, -117.0386751345948682 ) ) ;
#3320 = CARTESIAN_POINT ( 'NONE',  ( -5.999999999999963585, 1.780251999655701777E-13, -98.91367513459483973 ) ) ;
#3321 = CARTESIAN_POINT ( 'NONE',  ( -5.801553858104669281, 9.346157964213334779, -26.58091173639826366 ) ) ;
#3322 = LINE ( 'NONE', #22240, #578 ) ;
#3323 = CARTESIAN_POINT ( 'NONE',  ( 6.350852961086080661, -9.614813431917819062E-14, -169.8750000000000568 ) ) ;
#3324 = CARTESIAN_POINT ( 'NONE',  ( 120.8124999999997726, 1.035533905932899401, -2.499999999999844569 ) ) ;
#3325 = CARTESIAN_POINT ( 'NONE',  ( 152.4300748654052029, 2.278174593051795149, -5.500000000000228262 ) ) ;
#3326 = CARTESIAN_POINT ( 'NONE',  ( 2.775557561562891351E-14, 6.250000000000033751, -169.9330127018922099 ) ) ;
#3327 = CARTESIAN_POINT ( 'NONE',  ( -0.3085845443849983827, -9.691415455615135954, 4.244941038143176470 ) ) ;
#3328 = CARTESIAN_POINT ( 'NONE',  ( 23.31250000000007461, -0.8284271247460553989, 2.000000000000091926 ) ) ;
#3329 = ADVANCED_FACE ( 'NONE', ( #7951 ), #29286, .F. ) ;
#3330 = CARTESIAN_POINT ( 'NONE',  ( 3.175426480543072749, 5.499999999999865885, -117.1249999999999858 ) ) ;
#3331 = SURFACE_STYLE_USAGE ( .BOTH. , #28983 ) ;
#3332 = ADVANCED_FACE ( 'NONE', ( #17656 ), #17361, .T. ) ;
#3333 = CARTESIAN_POINT ( 'NONE',  ( 4.763139720814407951, -2.749999999999988454, -108.5000000000000426 ) ) ;
#3334 = CARTESIAN_POINT ( 'NONE',  ( 15.00000000000000000, 0.000000000000000000, 0.000000000000000000 ) ) ;
#3335 = EDGE_LOOP ( 'NONE', ( #12325, #19985, #15303, #21526 ) ) ;
#3336 = CARTESIAN_POINT ( 'NONE',  ( 15.75000000000006928, 1.873492889145123019, 1.873492889144734441 ) ) ;
#3337 = CARTESIAN_POINT ( 'NONE',  ( 119.5624999999998153, -2.499999999999874767, -1.035533905932629173 ) ) ;
#3338 = CARTESIAN_POINT ( 'NONE',  ( 135.0338636289978069, -7.698222997088485009, -8.313259093246843534 ) ) ;
#3339 = ORIENTED_EDGE ( 'NONE', *, *, #12241, .F. ) ;
#3340 = CARTESIAN_POINT ( 'NONE',  ( 3.175426480543072749, -5.500000000000105693, -161.1250000000000284 ) ) ;
#3341 = CARTESIAN_POINT ( 'NONE',  ( -5.196152422706601826, 2.999999999999975131, -156.0386751345948539 ) ) ;
#3342 = CARTESIAN_POINT ( 'NONE',  ( -5.412658773652684552, -3.125000000000099920, -81.56698729810784698 ) ) ;
#3343 = ORIENTED_EDGE ( 'NONE', *, *, #28060, .T. ) ;
#3344 = DIRECTION ( 'NONE',  ( -7.147005652999508048E-36, 5.642372883946980038E-36, 1.000000000000000000 ) ) ;
#3345 = ORIENTED_EDGE ( 'NONE', *, *, #2521, .F. ) ;
#3346 = CARTESIAN_POINT ( 'NONE',  ( 133.4211002691896510, -4.999999999999989342, -2.071067811865468400 ) ) ;
#3347 =( BOUNDED_CURVE ( )  B_SPLINE_CURVE ( 2, ( #2311, #14324, #30405, #9374, #16626, #9530, #4893, #29943, #8923 ),
 .UNSPECIFIED., .F., .T. ) 
 B_SPLINE_CURVE_WITH_KNOTS ( ( 3, 2, 2, 2, 3 ),
 ( 0.2638888888888888951, 0.2648148148148148362, 0.2666666666666666630, 0.2685185185185185452, 0.2694444444444444309 ),
 .UNSPECIFIED. ) 
 CURVE ( )  GEOMETRIC_REPRESENTATION_ITEM ( )  RATIONAL_B_SPLINE_CURVE ( ( 0.9330127018922194093, 0.9330127018922194093, 1.000000000000000000, 0.8660254037844388186, 1.000000000000000000, 0.8660254037844388186, 1.000000000000000000, 0.9330127018922214077, 0.9330127018922194093 ) ) 
 REPRESENTATION_ITEM ( '' )  );
#3348 = VERTEX_POINT ( 'NONE', #24532 ) ;
#3349 = CARTESIAN_POINT ( 'NONE',  ( 3.608439182435180470, -6.249999999999997335, -133.6919872981078470 ) ) ;
#3350 = DIRECTION ( 'NONE',  ( -7.147005652999508048E-36, 5.642372883946980038E-36, 1.000000000000000000 ) ) ;
#3351 = CARTESIAN_POINT ( 'NONE',  ( 5.196152422706629359, 3.000000000000002665, -47.96132486540521711 ) ) ;
#3352 = ORIENTED_EDGE ( 'NONE', *, *, #29806, .T. ) ;
#3353 = CARTESIAN_POINT ( 'NONE',  ( 14.25000000000012434, 5.551115123125782702E-14, 2.000000000000001776 ) ) ;
#3354 = CARTESIAN_POINT ( 'NONE',  ( 149.2574251345948255, -2.278174593051764951, 5.500000000000262013 ) ) ;
#3355 = CARTESIAN_POINT ( 'NONE',  ( -5.999999999999963585, 1.780251999655701777E-13, -60.83632486540522422 ) ) ;
#3356 =( BOUNDED_CURVE ( )  B_SPLINE_CURVE ( 2, ( #17551, #22755, #26869, #1385, #5830, #10795, #29492, #6154, #23371 ),
 .UNSPECIFIED., .F., .T. ) 
 B_SPLINE_CURVE_WITH_KNOTS ( ( 3, 2, 2, 2, 3 ),
 ( 0.4843750000000000000, 0.4921875000000000000, 0.5000000000000000000, 0.5078125000000000000, 0.5156250000000000000 ),
 .UNSPECIFIED. ) 
 CURVE ( )  GEOMETRIC_REPRESENTATION_ITEM ( )  RATIONAL_B_SPLINE_CURVE ( ( 1.000000000000000000, 0.9238795325112867385, 1.000000000000000000, 0.9238795325112867385, 1.000000000000000000, 0.9238795325112867385, 1.000000000000000000, 0.9238795325112867385, 1.000000000000000000 ) ) 
 REPRESENTATION_ITEM ( '' )  );
#3357 = CARTESIAN_POINT ( 'NONE',  ( 134.7038997308104058, 2.071067811865468400, 4.999999999999989342 ) ) ;
#3358 = CARTESIAN_POINT ( 'NONE',  ( 0.000000000000000000, -5.999999999999991118, -55.03867513459481842 ) ) ;
#3359 = CARTESIAN_POINT ( 'NONE',  ( 13.72617513459485927, -2.499999999999904521, 1.035533905932689347 ) ) ;
#3360 = CARTESIAN_POINT ( 'NONE',  ( 3.608439182435180470, -6.249999999999997335, -69.19198729810781856 ) ) ;
#3361 = CARTESIAN_POINT ( 'NONE',  ( -3.608439182435052128, -6.250000000000110134, -51.44198729810784698 ) ) ;
#3362 = CARTESIAN_POINT ( 'NONE',  ( -5.999999999999956479, -1.607695154586745057, -128.8466878364870354 ) ) ;
#3363 = DIRECTION ( 'NONE',  ( 0.000000000000000000, 0.3428396514843867759, 0.9393939393939395588 ) ) ;
#3364 = CARTESIAN_POINT ( 'NONE',  ( 107.3988248654050182, -0.8284271247461153509, -1.999999999999791278 ) ) ;
#3365 = EDGE_CURVE ( 'NONE', #28361, #18697, #7651, .T. ) ;
#3366 = CARTESIAN_POINT ( 'NONE',  ( 4.763139720814407951, -2.749999999999988454, -129.5000000000000000 ) ) ;
#3367 = CARTESIAN_POINT ( 'NONE',  ( 0.000000000000000000, 0.000000000000000000, 0.000000000000000000 ) ) ;
#3368 = ORIENTED_EDGE ( 'NONE', *, *, #20291, .T. ) ;
#3369 = CARTESIAN_POINT ( 'NONE',  ( 3.464101615137852974, 5.999999999999884537, -173.8363248654051461 ) ) ;
#3370 = VECTOR ( 'NONE', #29514, 1000.000000000000000 ) ;
#3371 = CARTESIAN_POINT ( 'NONE',  ( 0.000000000000000000, 0.000000000000000000, 0.000000000000000000 ) ) ;
#3372 = FACE_OUTER_BOUND ( 'NONE', #8859, .T. ) ;
#3373 = FACE_OUTER_BOUND ( 'NONE', #12431, .T. ) ;
#3374 = CARTESIAN_POINT ( 'NONE',  ( 104.9087725016132140, -1.661713789967635524, -1.038312543894557294 ) ) ;
#3375 = COLOUR_RGB ( '', 0.40784314, 0.44705882, 0.49803922) ;
#3376 = ORIENTED_EDGE ( 'NONE', *, *, #22189, .F. ) ;
#3377 = CARTESIAN_POINT ( 'NONE',  ( 112.9372167782374987, -0.7662911109076785410, 1.849990392679591977 ) ) ;
#3378 = DIRECTION ( 'NONE',  ( 1.000000000000000000, -0.000000000000000000, -0.000000000000000000 ) ) ;
#3379 = CARTESIAN_POINT ( 'NONE',  ( 11.25000000000001066, 1.110223024625156540E-13, 1.999999999999946265 ) ) ;
#3380 = CARTESIAN_POINT ( 'NONE',  ( 2.775557561562891351E-14, 6.250000000000033751, -97.06698729810780435 ) ) ;
#3381 = CARTESIAN_POINT ( 'NONE',  ( 3.464101615137757051, -5.999999999999979572, -50.41367513459484684 ) ) ;
#3382 = CARTESIAN_POINT ( 'NONE',  ( -9.999999999999772626, -90.00000000000001421, 3.000000000000002665 ) ) ;
#3383 = CARTESIAN_POINT ( 'NONE',  ( 114.4999999999998721, -2.499999999999891198, 0.000000000000000000 ) ) ;
#3384 = SURFACE_STYLE_FILL_AREA ( #8005 ) ;
#3385 = FACE_OUTER_BOUND ( 'NONE', #7622, .T. ) ;
#3386 = ORIENTED_EDGE ( 'NONE', *, *, #15305, .T. ) ;
#3387 = CARTESIAN_POINT ( 'NONE',  ( 5.196152422706629359, 3.000000000000002665, -81.53867513459483973 ) ) ;
#3388 = EDGE_CURVE ( 'NONE', #15417, #2367, #12871, .T. ) ;
#3389 = CARTESIAN_POINT ( 'NONE',  ( 6.350852961086080661, -9.614813431917819062E-14, -52.87500000000002132 ) ) ;
#3390 = VECTOR ( 'NONE', #30280, 1000.000000000000114 ) ;
#3391 = DIRECTION ( 'NONE',  ( 0.000000000000000000, 0.000000000000000000, 1.000000000000000000 ) ) ;
#3392 = CARTESIAN_POINT ( 'NONE',  ( 0.000000000000000000, -5.999999999999991118, -51.46132486540522422 ) ) ;
#3393 = CARTESIAN_POINT ( 'NONE',  ( -3.608439182435115633, 6.249999999999965361, -73.80801270189223828 ) ) ;
#3394 = CARTESIAN_POINT ( 'NONE',  ( 0.000000000000000000, -5.999999999999991118, -172.9613248654052313 ) ) ;
#3395 = CARTESIAN_POINT ( 'NONE',  ( 155.6101497308104058, 3.535533905932725318, 3.535533905932725318 ) ) ;
#3396 = FACE_OUTER_BOUND ( 'NONE', #18441, .T. ) ;
#3397 =( BOUNDED_CURVE ( )  B_SPLINE_CURVE ( 2, ( #3704, #20464, #10821, #22931, #8637, #18041, #13590, #13289, #20172 ),
 .UNSPECIFIED., .F., .F. ) 
 B_SPLINE_CURVE_WITH_KNOTS ( ( 3, 2, 2, 2, 3 ),
 ( 0.02499999999999999445, 0.02592592592592592518, 0.02777777777777777624, 0.02962962962962963076, 0.03055555555555556149 ),
 .UNSPECIFIED. ) 
 CURVE ( )  GEOMETRIC_REPRESENTATION_ITEM ( )  RATIONAL_B_SPLINE_CURVE ( ( 0.9330127018922195203, 0.9330127018922190762, 1.000000000000000000, 0.8660254037844388186, 1.000000000000000000, 0.8660254037844388186, 1.000000000000000000, 0.9330127018922189652, 0.9330127018922194093 ) ) 
 REPRESENTATION_ITEM ( '' )  );
#3398 = VECTOR ( 'NONE', #15561, 1000.000000000000000 ) ;
#3399 = CARTESIAN_POINT ( 'NONE',  ( -5.999999999999968026, -1.607695154586722186, -152.8466878364870070 ) ) ;
#3400 = CARTESIAN_POINT ( 'NONE',  ( 0.000000000000000000, 0.000000000000000000, 0.000000000000000000 ) ) ;
#3401 = CARTESIAN_POINT ( 'NONE',  ( 3.464101615137757051, -5.999999999999979572, -93.91367513459479710 ) ) ;
#3402 = EDGE_CURVE ( 'NONE', #17791, #9387, #22101, .T. ) ;
#3403 = CARTESIAN_POINT ( 'NONE',  ( -3.175426480542816066, 5.499999999999865885, -134.8750000000000284 ) ) ;
#3404 = CARTESIAN_POINT ( 'NONE',  ( 105.6011751345947260, -0.8284271247461453269, 2.000000000000212275 ) ) ;
#3405 = CARTESIAN_POINT ( 'NONE',  ( -7.216878364870328078, 0.000000000000000000, -148.5580127018922667 ) ) ;
#3406 = DIRECTION ( 'NONE',  ( 1.000000000000000000, -5.551115123125773458E-17, -1.260129944081490338E-35 ) ) ;
#3407 = CARTESIAN_POINT ( 'NONE',  ( 4.763139720814407951, -2.749999999999988454, -62.00000000000000000 ) ) ;
#3408 = CARTESIAN_POINT ( 'NONE',  ( 4.763139720814407951, -2.749999999999988454, -56.00000000000004974 ) ) ;
#3409 = DIRECTION ( 'NONE',  ( -1.000000000000000000, -0.000000000000000000, -0.000000000000000000 ) ) ;
#3410 = VERTEX_POINT ( 'NONE', #3633 ) ;
#3411 = CARTESIAN_POINT ( 'NONE',  ( 153.3750000000000284, 0.000000000000000000, 6.000000000000005329 ) ) ;
#3412 = CARTESIAN_POINT ( 'NONE',  ( 14.00000000000006750, 2.000000000000112799, 0.000000000000000000 ) ) ;
#3413 = CARTESIAN_POINT ( 'NONE',  ( 6.000000000000000888, 1.743066579297358182E-13, -98.16367513459481131 ) ) ;
#3414 = ORIENTED_EDGE ( 'NONE', *, *, #1861, .F. ) ;
#3415 = CARTESIAN_POINT ( 'NONE',  ( 143.7187500000000284, 2.485281374238555774, -6.000000000000005329 ) ) ;
#3416 = CARTESIAN_POINT ( 'NONE',  ( 161.4448303879796640, -4.634055226201747146, -3.737401695183885764 ) ) ;
#3417 = ORIENTED_EDGE ( 'NONE', *, *, #3601, .F. ) ;
#3418 = CARTESIAN_POINT ( 'NONE',  ( 0.000000000000000000, 5.499999999999991118, -147.0000000000000284 ) ) ;
#3419 = CARTESIAN_POINT ( 'NONE',  ( 17.43750000000013145, -1.999999999999851674, 0.8284271247463557142 ) ) ;
#3420 = ORIENTED_EDGE ( 'NONE', *, *, #25051, .F. ) ;
#3421 = CARTESIAN_POINT ( 'NONE',  ( 5.412658773652739619, 3.124999999999988898, -151.3169872981078186 ) ) ;
#3422 = ADVANCED_FACE ( 'NONE', ( #22249 ), #1340, .F. ) ;
#3423 = CARTESIAN_POINT ( 'NONE',  ( -3.175426480542816510, 5.499999999999865885, -80.87500000000002842 ) ) ;
#3424 = CARTESIAN_POINT ( 'NONE',  ( 7.216878364870455975, -6.409875621278545621E-14, -93.80801270189219565 ) ) ;
#3425 = CARTESIAN_POINT ( 'NONE',  ( 119.9999999999998579, 2.265773637426599318, 0.8226836970540328808 ) ) ;
#3426 = DIRECTION ( 'NONE',  ( -1.387778780781444256E-14, 1.000000000000000000, 0.000000000000000000 ) ) ;
#3427 = TOROIDAL_SURFACE ( 'NONE', #20160, 11.00000000000000355, 1.000000000000000000 ) ;
#3428 = DIRECTION ( 'NONE',  ( 0.000000000000000000, 5.551115123125767911E-17, -1.000000000000000000 ) ) ;
#3429 = CARTESIAN_POINT ( 'NONE',  ( 134.9304254777565291, -7.819842479447205896, 8.000000000000008882 ) ) ;
#3430 = EDGE_CURVE ( 'NONE', #19618, #27870, #8492, .T. ) ;
#3431 = EDGE_CURVE ( 'NONE', #4040, #1574, #22411, .T. ) ;
#3432 = CARTESIAN_POINT ( 'NONE',  ( -3.175426480542816066, -5.500000000000057732, -152.3749999999999716 ) ) ;
#3433 = LINE ( 'NONE', #19739, #6166 ) ;
#3434 = CARTESIAN_POINT ( 'NONE',  ( 4.763139720814407951, -2.749999999999988454, -146.0000000000000284 ) ) ;
#3435 = CARTESIAN_POINT ( 'NONE',  ( -9.999999999999980460, -60.00000000000001421, -3.000000000000002665 ) ) ;
#3436 = CARTESIAN_POINT ( 'NONE',  ( 4.763139720814407951, -2.749999999999988454, -96.50000000000002842 ) ) ;
#3437 = CARTESIAN_POINT ( 'NONE',  ( -3.175426480542816510, 5.499999999999865885, -77.87500000000001421 ) ) ;
#3438 =( BOUNDED_CURVE ( )  B_SPLINE_CURVE ( 2, ( #17647, #24976, #13214, #15187, #20087, #26969, #22551, #1484, #20247 ),
 .UNSPECIFIED., .F., .T. ) 
 B_SPLINE_CURVE_WITH_KNOTS ( ( 3, 2, 2, 2, 3 ),
 ( 0.4624999999999990230, 0.4687499999999992228, 0.4749999999999994782, 0.4812499999999997335, 0.4875000000000000444 ),
 .UNSPECIFIED. ) 
 CURVE ( )  GEOMETRIC_REPRESENTATION_ITEM ( )  RATIONAL_B_SPLINE_CURVE ( ( 1.000000000000012212, 0.9238795325112745260, 1.000000000000000000, 0.9238795325112867385, 1.000000000000000000, 0.9238795325112867385, 1.000000000000000000, 0.9238795325112867385, 1.000000000000000000 ) ) 
 REPRESENTATION_ITEM ( '' )  );
#3439 = CARTESIAN_POINT ( 'NONE',  ( 151.4211002691896510, -4.999999999999989342, -2.071067811865468400 ) ) ;
#3440 = CYLINDRICAL_SURFACE ( 'NONE', #16706, 6.000000000000000888 ) ;
#3441 = CARTESIAN_POINT ( 'NONE',  ( 151.6011751345948539, 3.889087296526011706, -3.889087296526011706 ) ) ;
#3442 = FACE_OUTER_BOUND ( 'NONE', #24095, .T. ) ;
#3443 = CARTESIAN_POINT ( 'NONE',  ( 112.0238248654050608, -0.8284271247460852639, 2.000000000000332179 ) ) ;
#3444 = CARTESIAN_POINT ( 'NONE',  ( -15.49999999999999289, -24.99999999999999289, -8.000000000000007105 ) ) ;
#3445 = DIRECTION ( 'NONE',  ( -7.147005652999508048E-36, 5.642372883946980038E-36, 1.000000000000000000 ) ) ;
#3446 = ORIENTED_EDGE ( 'NONE', *, *, #15487, .F. ) ;
#3447 = CARTESIAN_POINT ( 'NONE',  ( 161.4375000000000284, -4.242640687119298093, -4.242640687119298093 ) ) ;
#3448 = DIRECTION ( 'NONE',  ( -1.000000000000000000, -1.665334536937731113E-16, 1.526556658859586792E-16 ) ) ;
#3449 = CARTESIAN_POINT ( 'NONE',  ( 110.1011751345946692, 0.8284271247462654530, -1.999999999999851674 ) ) ;
#3450 = CARTESIAN_POINT ( 'NONE',  ( 120.4377832217621176, 1.849990392679562001, 0.7662911109080692285 ) ) ;
#3451 = VECTOR ( 'NONE', #18949, 1000.000000000000000 ) ;
#3452 = CARTESIAN_POINT ( 'NONE',  ( 24.89327801240793647, 1.031043948637415886, -1.842165862623910799 ) ) ;
#3453 = ORIENTED_EDGE ( 'NONE', *, *, #11147, .F. ) ;
#3454 = CIRCLE ( 'NONE', #26044, 0.5000000000000004441 ) ;
#3455 = ORIENTED_EDGE ( 'NONE', *, *, #271, .F. ) ;
#3456 = EDGE_CURVE ( 'NONE', #19810, #28850, #30213, .T. ) ;
#3457 = CARTESIAN_POINT ( 'NONE',  ( 6.350852961086080661, -9.614813431917819062E-14, -103.8750000000000000 ) ) ;
#3458 = CARTESIAN_POINT ( 'NONE',  ( -5.196152422706573404, -3.000000000000002665, -89.78867513459488237 ) ) ;
#3459 = CARTESIAN_POINT ( 'NONE',  ( -5.412658773652684552, -3.125000000000099920, -115.4330127018922099 ) ) ;
#3460 = ORIENTED_EDGE ( 'NONE', *, *, #8067, .F. ) ;
#3461 = CARTESIAN_POINT ( 'NONE',  ( 0.000000000000000000, 0.000000000000000000, 0.000000000000000000 ) ) ;
#3462 = CARTESIAN_POINT ( 'NONE',  ( 105.8124999999999574, 1.035533905932839449, -2.499999999999724221 ) ) ;
#3463 = COLOUR_RGB ( '', 0.08235294, 0.09019608, 0.10196078) ;
#3464 = CARTESIAN_POINT ( 'NONE',  ( 2.775557561562891351E-14, 6.250000000000033751, -52.93301270189220986 ) ) ;
#3465 = ORIENTED_EDGE ( 'NONE', *, *, #24886, .F. ) ;
#3466 = CARTESIAN_POINT ( 'NONE',  ( 5.999999999999974243, 1.607695154586759934, -117.5966878364870354 ) ) ;
#3467 = EDGE_CURVE ( 'NONE', #14042, #25961, #5469, .T. ) ;
#3468 = CARTESIAN_POINT ( 'NONE',  ( 116.0386751345946834, 5.551115123125782702E-14, -1.999999999999890754 ) ) ;
#3469 = CARTESIAN_POINT ( 'NONE',  ( -5.999999999999963585, 8.134310703387671600E-14, -135.8363248654052597 ) ) ;
#3470 = LINE ( 'NONE', #5626, #19221 ) ;
#3471 = CARTESIAN_POINT ( 'NONE',  ( -3.175426480542816510, -5.500000000000057732, -167.3750000000000568 ) ) ;
#3472 = CARTESIAN_POINT ( 'NONE',  ( 105.2502832217622881, 1.308140751793668288, -1.308140751793640533 ) ) ;
#3473 = CARTESIAN_POINT ( 'NONE',  ( -5.999999999999919176, 1.607695154586804565, -107.4033121635130072 ) ) ;
#3474 = CARTESIAN_POINT ( 'NONE',  ( 5.412658773652739619, 3.124999999999988898, -170.1830127018922383 ) ) ;
#3475 = CARTESIAN_POINT ( 'NONE',  ( -0.8691260360719469391, -9.261747927856070817, 4.026027341348647148 ) ) ;
#3476 = VECTOR ( 'NONE', #12338, 1000.000000000000000 ) ;
#3477 = CARTESIAN_POINT ( 'NONE',  ( 6.350852961086080661, -9.614813431917819062E-14, -117.3750000000000000 ) ) ;
#3478 = CARTESIAN_POINT ( 'NONE',  ( 6.000000000000000888, -3.330669073875464691E-16, -7.560779664488942560E-35 ) ) ;
#3479 = CARTESIAN_POINT ( 'NONE',  ( -2.775557561562891351E-14, -5.500000000000115463, -107.2500000000000142 ) ) ;
#3480 = CARTESIAN_POINT ( 'NONE',  ( 0.000000000000000000, 0.000000000000000000, 0.000000000000000000 ) ) ;
#3481 = DIRECTION ( 'NONE',  ( 0.000000000000000000, 0.000000000000000000, -1.000000000000000000 ) ) ;
#3482 = CARTESIAN_POINT ( 'NONE',  ( -3.464101615137757051, -5.999999999999979572, -84.58632486540520290 ) ) ;
#3483 =( BOUNDED_CURVE ( )  B_SPLINE_CURVE ( 3, ( #21384, #28412, #26121, #5068 ),
 .UNSPECIFIED., .F., .T. ) 
 B_SPLINE_CURVE_WITH_KNOTS ( ( 4, 4 ),
 ( 0.000000000000000000, 1.570796326794896558 ),
 .UNSPECIFIED. ) 
 CURVE ( )  GEOMETRIC_REPRESENTATION_ITEM ( )  RATIONAL_B_SPLINE_CURVE ( ( 1.000000000000000000, 0.8047378541243649375, 0.8047378541243649375, 1.000000000000000000 ) ) 
 REPRESENTATION_ITEM ( '' )  );
#3484 = AXIS2_PLACEMENT_3D ( 'NONE', #11118, #20467, #29825 ) ;
#3485 = VERTEX_POINT ( 'NONE', #18724 ) ;
#3486 = CARTESIAN_POINT ( 'NONE',  ( 14.87500000000002665, 1.665334536937734811E-13, 2.649519052838278377 ) ) ;
#3487 = AXIS2_PLACEMENT_3D ( 'NONE', #15111, #807, #7862 ) ;
#3488 = CARTESIAN_POINT ( 'NONE',  ( 118.9374999999996589, 2.500000000000234479, -1.035533905932568777 ) ) ;
#3489 = CARTESIAN_POINT ( 'NONE',  ( 6.000000000000000888, 1.743066579297358182E-13, -71.16367513459481131 ) ) ;
#3490 = DIRECTION ( 'NONE',  ( 1.000000000000000000, -5.551115123125774074E-17, -1.260129944081490070E-35 ) ) ;
#3491 = VERTEX_POINT ( 'NONE', #19901 ) ;
#3492 = CARTESIAN_POINT ( 'NONE',  ( -4.763139720814407951, 2.749999999999946709, -161.7500000000000568 ) ) ;
#3493 = AXIS2_PLACEMENT_3D ( 'NONE', #16183, #20439, #18161 ) ;
#3494 = CARTESIAN_POINT ( 'NONE',  ( 138.9300748654052029, 2.278174593051671692, -5.500000000000352607 ) ) ;
#3495 = CARTESIAN_POINT ( 'NONE',  ( -5.412658773652739619, 3.124999999999975131, -78.81698729810781856 ) ) ;
#3496 = CARTESIAN_POINT ( 'NONE',  ( -5.196152422706573404, -3.000000000000002665, -97.28867513459482552 ) ) ;
#3497 = ORIENTED_EDGE ( 'NONE', *, *, #20101, .T. ) ;
#3498 = CARTESIAN_POINT ( 'NONE',  ( -5.999999999999963585, -1.487416814333745711E-14, -143.9136751345948255 ) ) ;
#3499 = VERTEX_POINT ( 'NONE', #28945 ) ;
#3500 = CARTESIAN_POINT ( 'NONE',  ( 156.7500000000000284, -6.000000000000005329, 0.000000000000000000 ) ) ;
#3501 = ADVANCED_FACE ( 'NONE', ( #28794 ), #5297, .T. ) ;
#3502 = EDGE_CURVE ( 'NONE', #27301, #22988, #24130, .T. ) ;
#3503 = CARTESIAN_POINT ( 'NONE',  ( 2.775557561562891351E-14, -6.250000000000061284, -139.1830127018922667 ) ) ;
#3504 = EDGE_LOOP ( 'NONE', ( #1431, #26587, #1475, #1499 ) ) ;
#3505 = CARTESIAN_POINT ( 'NONE',  ( 157.3988248654052313, 3.889087296526011706, 3.889087296526011706 ) ) ;
#3506 = CARTESIAN_POINT ( 'NONE',  ( 3.608439182435180470, -6.249999999999997335, -124.6919872981078043 ) ) ;
#3507 = DIRECTION ( 'NONE',  ( -1.000000000000000000, 0.000000000000000000, 0.000000000000000000 ) ) ;
#3508 = CARTESIAN_POINT ( 'NONE',  ( -6.350852961085760029, -1.281975124255709124E-13, -173.6250000000000284 ) ) ;
#3509 = DIRECTION ( 'NONE',  ( 1.665334536937739001E-16, -1.000000000000000000, -8.881784197001260212E-16 ) ) ;
#3510 = ORIENTED_EDGE ( 'NONE', *, *, #21687, .T. ) ;
#3511 = CARTESIAN_POINT ( 'NONE',  ( 17.25000000000001421, 1.665334536937734811E-13, 2.000000000000001776 ) ) ;
#3512 = CARTESIAN_POINT ( 'NONE',  ( -3.464101615137725076, 5.999999999999979572, -135.1636751345948539 ) ) ;
#3513 = CARTESIAN_POINT ( 'NONE',  ( 6.000000000000000888, -1.859271017917181981E-14, -172.5863248654052029 ) ) ;
#3514 = DIRECTION ( 'NONE',  ( -7.147005652999508048E-36, 5.642372883946980038E-36, 1.000000000000000000 ) ) ;
#3515 = DIRECTION ( 'NONE',  ( 1.000000000000000000, 0.000000000000000000, 0.000000000000000000 ) ) ;
#3516 = CARTESIAN_POINT ( 'NONE',  ( 6.000000000000000888, 1.743066579297358182E-13, -107.1636751345948539 ) ) ;
#3517 = FACE_OUTER_BOUND ( 'NONE', #612, .T. ) ;
#3518 = CARTESIAN_POINT ( 'NONE',  ( 5.412658773652712085, -3.125000000000086153, -70.56698729810784698 ) ) ;
#3519 = CARTESIAN_POINT ( 'NONE',  ( 135.0000000000000568, 3.752929936578043080, 4.235410701944677392 ) ) ;
#3520 = LINE ( 'NONE', #17699, #16113 ) ;
#3521 = CARTESIAN_POINT ( 'NONE',  ( -5.196152422706601826, 2.999999999999975131, -127.5386751345948255 ) ) ;
#3522 = CARTESIAN_POINT ( 'NONE',  ( 4.763139720814407951, -2.749999999999988454, -131.0000000000000000 ) ) ;
#3523 = FACE_OUTER_BOUND ( 'NONE', #3529, .T. ) ;
#3524 = ORIENTED_EDGE ( 'NONE', *, *, #14977, .T. ) ;
#3525 = CARTESIAN_POINT ( 'NONE',  ( -5.999999999999944933, 1.607695154586759934, -131.9806624327025872 ) ) ;
#3526 = CARTESIAN_POINT ( 'NONE',  ( -0.5000000000000004441, -10.50000000000000888, 8.500000000000007105 ) ) ;
#3527 = FACE_OUTER_BOUND ( 'NONE', #11967, .T. ) ;
#3528 = CARTESIAN_POINT ( 'NONE',  ( 5.196152422706629359, -2.999999999999988898, -99.78867513459482552 ) ) ;
#3529 = EDGE_LOOP ( 'NONE', ( #21935, #4451, #1512, #24034 ) ) ;
#3530 = CARTESIAN_POINT ( 'NONE',  ( 111.9372167782374703, -0.7662911109077388261, 1.849990392679652151 ) ) ;
#3531 = CARTESIAN_POINT ( 'NONE',  ( 0.000000000000000000, 0.000000000000000000, -43.99152654425658682 ) ) ;
#3532 = CARTESIAN_POINT ( 'NONE',  ( -5.412658773652739619, 3.124999999999975131, -93.81698729810783277 ) ) ;
#3533 = CARTESIAN_POINT ( 'NONE',  ( 135.0000000000001705, 4.957041246451966643, -2.976925002759783112 ) ) ;
#3534 =( BOUNDED_CURVE ( )  B_SPLINE_CURVE ( 2, ( #12874, #3759, #3441, #5904, #10868, #17324, #17469, #13029, #26783 ),
 .UNSPECIFIED., .F., .T. ) 
 B_SPLINE_CURVE_WITH_KNOTS ( ( 3, 2, 2, 2, 3 ),
 ( 0.6375000000000001776, 0.6437500000000000444, 0.6499999999999996891, 0.6562499999999994449, 0.6624999999999992006 ),
 .UNSPECIFIED. ) 
 CURVE ( )  GEOMETRIC_REPRESENTATION_ITEM ( )  RATIONAL_B_SPLINE_CURVE ( ( 0.9999999999999973355, 0.9238795325112894030, 1.000000000000000000, 0.9238795325112867385, 1.000000000000000000, 0.9238795325112867385, 1.000000000000000000, 0.9238795325112961754, 0.9999999999999905631 ) ) 
 REPRESENTATION_ITEM ( '' )  );
#3535 = FACE_OUTER_BOUND ( 'NONE', #5228, .T. ) ;
#3536 = CARTESIAN_POINT ( 'NONE',  ( 115.1249999999998863, 1.767766952966376426, 1.767766952966320915 ) ) ;
#3537 = CARTESIAN_POINT ( 'NONE',  ( 140.6083823193137334, -11.80419115965730015, 4.059228028636210794 ) ) ;
#3538 = EDGE_CURVE ( 'NONE', #1389, #8961, #29474, .T. ) ;
#3539 =( BOUNDED_CURVE ( )  B_SPLINE_CURVE ( 2, ( #14600, #18914, #21349, #9368, #9975, #23952, #21508, #2308, #2890 ),
 .UNSPECIFIED., .F., .F. ) 
 B_SPLINE_CURVE_WITH_KNOTS ( ( 3, 2, 2, 2, 3 ),
 ( 0.01388888888888883955, 0.01481481481481483620, 0.01666666666666671848, 0.01851851851851848973, 0.01944444444444448639 ),
 .UNSPECIFIED. ) 
 CURVE ( )  GEOMETRIC_REPRESENTATION_ITEM ( )  RATIONAL_B_SPLINE_CURVE ( ( 0.9330127018922194093, 0.9330127018922154125, 1.000000000000000000, 0.8660254037844388186, 1.000000000000000000, 0.8660254037844388186, 1.000000000000000000, 0.9330127018922154125, 0.9330127018922194093 ) ) 
 REPRESENTATION_ITEM ( '' )  );
#3540 = CARTESIAN_POINT ( 'NONE',  ( 9.750000000000119016, 1.665334536937734811E-13, -1.999999999999890754 ) ) ;
#3541 = CARTESIAN_POINT ( 'NONE',  ( -3.464101615137725076, 5.999999999999979572, -81.16367513459479710 ) ) ;
#3542 = CARTESIAN_POINT ( 'NONE',  ( -6.350852961085760029, -1.281975124255709124E-13, -52.12500000000002132 ) ) ;
#3543 = CARTESIAN_POINT ( 'NONE',  ( 24.93750000000011013, 2.000000000000151879, -0.8284271247462354770 ) ) ;
#3544 = CARTESIAN_POINT ( 'NONE',  ( 0.000000000000000000, 0.000000000000000000, 0.000000000000000000 ) ) ;
#3545 = CARTESIAN_POINT ( 'NONE',  ( 3.464101615137852974, 5.999999999999884537, -61.91367513459483263 ) ) ;
#3546 = CARTESIAN_POINT ( 'NONE',  ( -7.216878364870328078, 0.000000000000000000, -75.05801270189223828 ) ) ;
#3547 = FACE_OUTER_BOUND ( 'NONE', #721, .T. ) ;
#3548 = VECTOR ( 'NONE', #26567, 1000.000000000000000 ) ;
#3549 = CARTESIAN_POINT ( 'NONE',  ( 152.1413997308104058, 2.071067811865468400, -4.999999999999989342 ) ) ;
#3550 = DIRECTION ( 'NONE',  ( -7.147005652999508048E-36, 5.642372883946980038E-36, 1.000000000000000000 ) ) ;
#3551 = CARTESIAN_POINT ( 'NONE',  ( 0.000000000000000000, 0.000000000000000000, 0.000000000000000000 ) ) ;
#3552 = CARTESIAN_POINT ( 'NONE',  ( 0.000000000000000000, 5.999999999999977796, -79.78867513459486815 ) ) ;
#3553 = CYLINDRICAL_SURFACE ( 'NONE', #16780, 6.000000000000000888 ) ;
#3554 = MECHANICAL_DESIGN_GEOMETRIC_PRESENTATION_REPRESENTATION (  '', ( #30058 ), #10480 ) ;
#3555 = CARTESIAN_POINT ( 'NONE',  ( -2.775557561562891351E-14, -5.500000000000115463, -128.2500000000000284 ) ) ;
#3556 = DIRECTION ( 'NONE',  ( -0.000000000000000000, 0.000000000000000000, 1.000000000000000000 ) ) ;
#3557 = CARTESIAN_POINT ( 'NONE',  ( 16.47617513459488237, 1.035533905932929599, 2.499999999999844569 ) ) ;
#3558 = ORIENTED_EDGE ( 'NONE', *, *, #13066, .F. ) ;
#3559 = CARTESIAN_POINT ( 'NONE',  ( -4.763139720814407951, 2.749999999999946709, -62.75000000000002842 ) ) ;
#3560 = DIRECTION ( 'NONE',  ( 0.000000000000000000, 0.000000000000000000, -1.000000000000000000 ) ) ;
#3561 = CARTESIAN_POINT ( 'NONE',  ( 6.350852961086080661, -9.614813431917819062E-14, -60.37500000000000000 ) ) ;
#3562 = VERTEX_POINT ( 'NONE', #5446 ) ;
#3563 = CARTESIAN_POINT ( 'NONE',  ( 145.2187500000000000, 2.485281374238556218, -6.000000000000005329 ) ) ;
#3564 = CARTESIAN_POINT ( 'NONE',  ( -5.999999999999963585, -1.487416814333745711E-14, -118.4136751345948255 ) ) ;
#3565 = ADVANCED_FACE ( 'NONE', ( #28638 ), #7609, .T. ) ;
#3566 = CARTESIAN_POINT ( 'NONE',  ( -6.000000000000007105, -1.607695154586655129, -104.8466878364870212 ) ) ;
#3567 = CARTESIAN_POINT ( 'NONE',  ( 110.8122167782374987, 0.7662911109077388261, 1.849990392679772278 ) ) ;
#3568 = CIRCLE ( 'NONE', #19288, 10.49999999999998224 ) ;
#3569 = VERTEX_POINT ( 'NONE', #24054 ) ;
#3570 = CARTESIAN_POINT ( 'NONE',  ( 144.8437500000000000, -6.000000000000005329, -2.485281374238555774 ) ) ;
#3571 = DIRECTION ( 'NONE',  ( -7.147005652999508048E-36, 5.642372883946980038E-36, 1.000000000000000000 ) ) ;
#3572 = ORIENTED_EDGE ( 'NONE', *, *, #29688, .T. ) ;
#3573 = CARTESIAN_POINT ( 'NONE',  ( 3.175426480543072749, -5.500000000000105693, -149.1250000000000284 ) ) ;
#3574 = EDGE_CURVE ( 'NONE', #27416, #13233, #10395, .T. ) ;
#3575 = CARTESIAN_POINT ( 'NONE',  ( -7.216878364870328078, 0.000000000000000000, -50.19198729810784698 ) ) ;
#3576 = CARTESIAN_POINT ( 'NONE',  ( 16.25000000000009948, 1.665334536937734811E-13, 2.000000000000001776 ) ) ;
#3577 = ORIENTED_EDGE ( 'NONE', *, *, #20951, .T. ) ;
#3578 = CARTESIAN_POINT ( 'NONE',  ( 5.412658773652712085, -3.125000000000086153, -148.5669872981077901 ) ) ;
#3579 = CARTESIAN_POINT ( 'NONE',  ( -6.350852961085760029, -1.281975124255709124E-13, -73.12500000000005684 ) ) ;
#3580 = CARTESIAN_POINT ( 'NONE',  ( 13.12500000000013678, 1.665334536937734811E-13, -2.649519052838444910 ) ) ;
#3581 = CARTESIAN_POINT ( 'NONE',  ( 3.608439182435180470, -6.249999999999997335, -91.05801270189225249 ) ) ;
#3582 = VERTEX_POINT ( 'NONE', #21765 ) ;
#3583 = CARTESIAN_POINT ( 'NONE',  ( -1.595708107228580142, -10.89084870836962970, -30.79786109011545392 ) ) ;
#3584 = CARTESIAN_POINT ( 'NONE',  ( 3.464101615137757051, -5.999999999999979572, -96.33632486540517448 ) ) ;
#3585 = CARTESIAN_POINT ( 'NONE',  ( 106.3988248654049471, -0.8284271247462053900, -1.999999999999791278 ) ) ;
#3586 = CARTESIAN_POINT ( 'NONE',  ( 6.000000000000000888, 1.743066579297358182E-13, -99.08632486540518869 ) ) ;
#3587 = CARTESIAN_POINT ( 'NONE',  ( -2.775557561562891351E-14, -5.500000000000115463, -153.7500000000000568 ) ) ;
#3588 = FACE_OUTER_BOUND ( 'NONE', #13778, .T. ) ;
#3589 = CARTESIAN_POINT ( 'NONE',  ( -6.350852961085760029, -1.281975124255709124E-13, -149.6250000000000568 ) ) ;
#3590 = CARTESIAN_POINT ( 'NONE',  ( 156.3675748654052029, -5.500000000000012434, 2.278174593052012309 ) ) ;
#3591 = PRESENTATION_LAYER_ASSIGNMENT (  '', '', ( #10514 ) ) ;
#3592 = UNCERTAINTY_MEASURE_WITH_UNIT (LENGTH_MEASURE( 1.000000000000000082E-05 ), #15981, 'distance_accuracy_value', 'NONE');
#3593 = CARTESIAN_POINT ( 'NONE',  ( -3.175426480542816066, -5.500000000000057732, -83.37500000000004263 ) ) ;
#3594 = CARTESIAN_POINT ( 'NONE',  ( 104.3122167782373992, -0.7662911109076785410, -1.849990392679291551 ) ) ;
#3595 = DIRECTION ( 'NONE',  ( -1.000000000000000000, 0.000000000000000000, 0.000000000000000000 ) ) ;
#3596 = CARTESIAN_POINT ( 'NONE',  ( 0.000000000000000000, 5.499999999999991118, -81.00000000000001421 ) ) ;
#3597 = CARTESIAN_POINT ( 'NONE',  ( 5.196152422706629359, -2.999999999999988898, -74.28867513459481131 ) ) ;
#3598 = CARTESIAN_POINT ( 'NONE',  ( 154.3273502691896510, -5.000000000000004441, 0.000000000000000000 ) ) ;
#3599 = CARTESIAN_POINT ( 'NONE',  ( 140.0000000000000284, -10.00000000000000888, -7.500000000000007105 ) ) ;
#3600 = CARTESIAN_POINT ( 'NONE',  ( 5.196152422706629359, -2.999999999999988898, -149.2886751345948824 ) ) ;
#3601 = EDGE_CURVE ( 'NONE', #23494, #15347, #11417, .T. ) ;
#3602 = CARTESIAN_POINT ( 'NONE',  ( 124.9999999999999432, -69.50000000000000000, 8.000000000000007105 ) ) ;
#3603 = CARTESIAN_POINT ( 'NONE',  ( 120.4372167782375271, 0.7662911109078588412, -1.849990392679291551 ) ) ;
#3604 = DIRECTION ( 'NONE',  ( 0.000000000000000000, -5.551115123125768527E-17, 1.000000000000000000 ) ) ;
#3605 = ORIENTED_EDGE ( 'NONE', *, *, #27533, .T. ) ;
#3606 = LINE ( 'NONE', #15340, #27311 ) ;
#3607 = CARTESIAN_POINT ( 'NONE',  ( -5.999999999999963585, -1.487416814333745711E-14, -80.33632486540523132 ) ) ;
#3608 = CARTESIAN_POINT ( 'NONE',  ( 6.000000000000000888, 1.743066579297358182E-13, -66.66367513459481131 ) ) ;
#3609 = VERTEX_POINT ( 'NONE', #27546 ) ;
#3610 = ADVANCED_FACE ( 'NONE', ( #22979 ), #13480, .T. ) ;
#3611 = ORIENTED_EDGE ( 'NONE', *, *, #9332, .F. ) ;
#3612 = CARTESIAN_POINT ( 'NONE',  ( -6.350852961085760029, -1.281975124255709124E-13, -94.12500000000004263 ) ) ;
#3613 = CARTESIAN_POINT ( 'NONE',  ( 0.000000000000000000, 0.000000000000000000, 0.000000000000000000 ) ) ;
#3614 = CARTESIAN_POINT ( 'NONE',  ( 2.775557561562891351E-14, -6.250000000000061284, -112.1830127018922383 ) ) ;
#3615 = EDGE_LOOP ( 'NONE', ( #10910, #25155, #29145, #21063 ) ) ;
#3616 = CYLINDRICAL_SURFACE ( 'NONE', #8803, 0.5000000000000004441 ) ;
#3617 = CARTESIAN_POINT ( 'NONE',  ( 135.0000000000000284, -8.850103465153400961, 7.500000000000122569 ) ) ;
#3618 = CARTESIAN_POINT ( 'NONE',  ( 3.608439182435180470, 6.249999999999982236, -50.05801270189224539 ) ) ;
#3619 = ORIENTED_EDGE ( 'NONE', *, *, #29167, .T. ) ;
#3620 = CARTESIAN_POINT ( 'NONE',  ( -19.99999999999998224, -25.00000000000010658, 8.000000000000007105 ) ) ;
#3621 = CARTESIAN_POINT ( 'NONE',  ( 115.9761751345946408, -0.8284271247461753029, -1.999999999999851674 ) ) ;
#3622 =( BOUNDED_CURVE ( )  B_SPLINE_CURVE ( 2, ( #986, #17774, #1450, #27094, #15475, #24799, #14993, #8680, #3747 ),
 .UNSPECIFIED., .F., .T. ) 
 B_SPLINE_CURVE_WITH_KNOTS ( ( 3, 2, 2, 2, 3 ),
 ( 0.8125000000000013323, 0.8187500000000010880, 0.8250000000000007327, 0.8312500000000004885, 0.8375000000000002442 ),
 .UNSPECIFIED. ) 
 CURVE ( )  GEOMETRIC_REPRESENTATION_ITEM ( )  RATIONAL_B_SPLINE_CURVE ( ( 0.9999999999999837907, 0.9238795325113029477, 1.000000000000000000, 0.9238795325112867385, 1.000000000000000000, 0.9238795325112867385, 1.000000000000000000, 0.9238795325112840739, 1.000000000000002665 ) ) 
 REPRESENTATION_ITEM ( '' )  );
#3623 = DIRECTION ( 'NONE',  ( -1.000000000000000000, -1.665334536937731113E-16, 1.526556658859586792E-16 ) ) ;
#3624 = DIRECTION ( 'NONE',  ( -1.000000000000000000, -1.665334536937731113E-16, 1.526556658859586792E-16 ) ) ;
#3625 = CARTESIAN_POINT ( 'NONE',  ( 4.763139720814407951, 2.750000000000002665, -172.7500000000000284 ) ) ;
#3626 = CARTESIAN_POINT ( 'NONE',  ( 118.8749999999998295, 1.767766952966320915, -1.767766952966320915 ) ) ;
#3627 = CARTESIAN_POINT ( 'NONE',  ( 5.196152422706629359, -2.999999999999988898, -157.7113248654052313 ) ) ;
#3628 = CARTESIAN_POINT ( 'NONE',  ( 2.775557561562891351E-14, -6.250000000000061284, -172.1830127018922383 ) ) ;
#3629 = CARTESIAN_POINT ( 'NONE',  ( 3.464101615137852974, 5.999999999999884537, -48.41367513459483263 ) ) ;
#3630 = CARTESIAN_POINT ( 'NONE',  ( 4.763139720814407951, -2.749999999999988454, -108.5000000000000426 ) ) ;
#3631 = CARTESIAN_POINT ( 'NONE',  ( 0.000000000000000000, 0.000000000000000000, 0.000000000000000000 ) ) ;
#3632 = CARTESIAN_POINT ( 'NONE',  ( -4.763139720814407951, -2.750000000000016431, -106.0000000000000426 ) ) ;
#3633 = CARTESIAN_POINT ( 'NONE',  ( 158.3363248654052313, 0.000000000000000000, -5.500000000000005329 ) ) ;
#3634 = FILL_AREA_STYLE_COLOUR ( '', #19445 ) ;
#3635 = SURFACE_SIDE_STYLE ('',( #4099 ) ) ;
#3636 = CARTESIAN_POINT ( 'NONE',  ( 0.000000000000000000, 5.999999999999977796, -145.2113248654052313 ) ) ;
#3637 = CARTESIAN_POINT ( 'NONE',  ( 14.00000000000020606, -1.873492889144789952, 1.873492889144956486 ) ) ;
#3638 = DIRECTION ( 'NONE',  ( 1.000000000000000000, -5.551115123125773458E-17, -1.260129944081490338E-35 ) ) ;
#3639 = EDGE_CURVE ( 'NONE', #17215, #25878, #22525, .T. ) ;
#3640 = CARTESIAN_POINT ( 'NONE',  ( 110.4377832217621034, 1.849990392679562001, 0.7662911109079489913 ) ) ;
#3641 = EDGE_LOOP ( 'NONE', ( #20645, #16995, #11387, #21182 ) ) ;
#3642 = CARTESIAN_POINT ( 'NONE',  ( 3.175426480543072749, 5.499999999999865885, -160.6250000000000284 ) ) ;
#3643 = CARTESIAN_POINT ( 'NONE',  ( 5.999999999999949374, 1.607695154586804565, -66.01933756729745539 ) ) ;
#3644 = CARTESIAN_POINT ( 'NONE',  ( 109.5622167782374277, 1.849990392679501827, -0.7662911109077087390 ) ) ;
#3645 = CARTESIAN_POINT ( 'NONE',  ( -3.608439182435052128, -6.250000000000110134, -82.94198729810780435 ) ) ;
#3646 = CARTESIAN_POINT ( 'NONE',  ( -3.464101615137757051, -5.999999999999979572, -97.16367513459481131 ) ) ;
#3647 = ORIENTED_EDGE ( 'NONE', *, *, #13236, .F. ) ;
#3648 = EDGE_CURVE ( 'NONE', #9719, #9700, #9501, .T. ) ;
#3649 = CARTESIAN_POINT ( 'NONE',  ( 116.0238248654051034, -0.8284271247460852639, 2.000000000000212275 ) ) ;
#3650 = ORIENTED_EDGE ( 'NONE', *, *, #4461, .F. ) ;
#3651 = VERTEX_POINT ( 'NONE', #25101 ) ;
#3652 = CARTESIAN_POINT ( 'NONE',  ( 154.6875000000000284, 4.242640687119269671, 4.242640687119298093 ) ) ;
#3653 = CARTESIAN_POINT ( 'NONE',  ( 6.350852961086080661, -9.614813431917819062E-14, -132.3750000000000284 ) ) ;
#3654 = CARTESIAN_POINT ( 'NONE',  ( -3.608439182435052128, -6.250000000000110134, -139.3080127018922667 ) ) ;
#3655 = VERTEX_POINT ( 'NONE', #13026 ) ;
#3656 = CARTESIAN_POINT ( 'NONE',  ( 6.000000000000052403, -1.607695154586662678, -57.15331216351299304 ) ) ;
#3657 = CARTESIAN_POINT ( 'NONE',  ( -7.216878364870328078, 0.000000000000000000, -120.6919872981078043 ) ) ;
#3658 =( NAMED_UNIT ( * ) SI_UNIT ( $, .STERADIAN. ) SOLID_ANGLE_UNIT ( ) );
#3659 = CARTESIAN_POINT ( 'NONE',  ( 4.763139720814407951, 2.750000000000002665, -171.2500000000000000 ) ) ;
#3660 = ORIENTED_EDGE ( 'NONE', *, *, #19184, .F. ) ;
#3661 = CARTESIAN_POINT ( 'NONE',  ( 15.87500000000008349, 1.414213562373201061, -1.414213562373090038 ) ) ;
#3662 = FACE_OUTER_BOUND ( 'NONE', #5787, .T. ) ;
#3664 = VECTOR ( 'NONE', #21183, 1000.000000000000000 ) ;
#3663 = CARTESIAN_POINT ( 'NONE',  ( 3.464101615137757051, -5.999999999999979572, -117.3363248654052171 ) ) ;
#3665 = DIRECTION ( 'NONE',  ( -0.000000000000000000, -0.000000000000000000, -1.000000000000000000 ) ) ;
#3666 = CARTESIAN_POINT ( 'NONE',  ( 13.97617513459482730, -1.035533905932629173, -2.499999999999904521 ) ) ;
#3667 = CARTESIAN_POINT ( 'NONE',  ( 114.9377832217620750, -1.849990392679501827, -0.7662911109076485650 ) ) ;
#3668 = CARTESIAN_POINT ( 'NONE',  ( 3.608439182435180470, 6.249999999999982236, -64.19198729810784698 ) ) ;
#3669 = CARTESIAN_POINT ( 'NONE',  ( 7.216878364870455975, -6.409875621278545621E-14, -52.44198729810779014 ) ) ;
#3670 = CARTESIAN_POINT ( 'NONE',  ( 119.6488248654049755, 2.000000000000091926, -0.8284271247460553989 ) ) ;
#3671 = SURFACE_STYLE_USAGE ( .BOTH. , #26860 ) ;
#3672 = CARTESIAN_POINT ( 'NONE',  ( -10.00000000000000178, -12.00000000000001066, -4.000000000000003553 ) ) ;
#3673 = CARTESIAN_POINT ( 'NONE',  ( 107.4613248654051176, 5.551115123125782702E-14, -1.999999999999890754 ) ) ;
#3674 = CARTESIAN_POINT ( 'NONE',  ( -4.763139720814407951, 2.749999999999946709, -133.2500000000000284 ) ) ;
#3675 = CARTESIAN_POINT ( 'NONE',  ( 0.000000000000000000, 5.999999999999977796, -50.71132486540519579 ) ) ;
#3676 = ORIENTED_EDGE ( 'NONE', *, *, #30129, .T. ) ;
#3677 = CARTESIAN_POINT ( 'NONE',  ( -5.999999999999963585, 8.134310703387671600E-14, -131.9136751345948255 ) ) ;
#3678 = AXIS2_PLACEMENT_3D ( 'NONE', #5600, #15002, #22213 ) ;
#3679 = EDGE_CURVE ( 'NONE', #26998, #26866, #22364, .T. ) ;
#3680 = CARTESIAN_POINT ( 'NONE',  ( 6.000000000000000888, -1.859271017917181981E-14, -120.0863248654052313 ) ) ;
#3681 = CARTESIAN_POINT ( 'NONE',  ( -5.999999999999963585, 8.134310703387671600E-14, -129.8363248654052313 ) ) ;
#3682 = ADVANCED_FACE ( 'NONE', ( #24948 ), #29571, .T. ) ;
#3683 = VERTEX_POINT ( 'NONE', #20056 ) ;
#3684 = CARTESIAN_POINT ( 'NONE',  ( 112.5622167782374703, 1.849990392679562001, -0.7662911109077087390 ) ) ;
#3685 = CARTESIAN_POINT ( 'NONE',  ( -5.412658773652684552, -3.125000000000099920, -113.0669872981078186 ) ) ;
#3686 = B_SPLINE_CURVE_WITH_KNOTS ( 'NONE', 3,
 ( #8124, #10617, #8446, #17692, #27018, #5983, #15867, #29933 ),
 .UNSPECIFIED., .F., .F.,
 ( 4, 2, 2, 4 ),
 ( 0.000000000000000000, 0.0001164977210824447509, 0.0002329954421648895019, 0.0004659908843297791122 ),
 .UNSPECIFIED. ) ;
#3687 = CIRCLE ( 'NONE', #23822, 2.000000000000003109 ) ;
#3688 = CARTESIAN_POINT ( 'NONE',  ( 19.66367513459493921, -1.767766952966209892, 1.767766952966376426 ) ) ;
#3689 = VECTOR ( 'NONE', #9022, 1000.000000000000000 ) ;
#3690 = CARTESIAN_POINT ( 'NONE',  ( 113.8749999999998721, 1.767766952966431937, -1.767766952966209892 ) ) ;
#3691 = ORIENTED_EDGE ( 'NONE', *, *, #21983, .F. ) ;
#3692 = FACE_OUTER_BOUND ( 'NONE', #2674, .T. ) ;
#3693 = CARTESIAN_POINT ( 'NONE',  ( 144.5625000000000284, -4.242640687119298093, 4.242640687119298093 ) ) ;
#3694 = EDGE_LOOP ( 'NONE', ( #5564, #3803, #18937, #9323 ) ) ;
#3695 = CARTESIAN_POINT ( 'NONE',  ( 136.0238248654052029, 3.889087296526011706, -3.889087296526011706 ) ) ;
#3696 =( GEOMETRIC_REPRESENTATION_CONTEXT ( 3 ) GLOBAL_UNCERTAINTY_ASSIGNED_CONTEXT ( ( #12130 ) ) GLOBAL_UNIT_ASSIGNED_CONTEXT ( ( #678, #370, #19441 ) ) REPRESENTATION_CONTEXT ( 'NONE', 'WORKASPACE' ) );
#3697 = CARTESIAN_POINT ( 'NONE',  ( -3.175426480542816510, -5.500000000000057732, -50.37500000000001421 ) ) ;
#3698 = CARTESIAN_POINT ( 'NONE',  ( 159.3824251345948255, 5.500000000000012434, 2.278174593052012309 ) ) ;
#3699 = CARTESIAN_POINT ( 'NONE',  ( -5.999999999999963585, 1.780251999655701777E-13, -51.83632486540522422 ) ) ;
#3700 = CARTESIAN_POINT ( 'NONE',  ( -3.464101615137725076, 5.999999999999979572, -61.66367513459484684 ) ) ;
#3701 = CARTESIAN_POINT ( 'NONE',  ( -3.608439182435115633, 6.249999999999965361, -78.30801270189225249 ) ) ;
#3702 = CARTESIAN_POINT ( 'NONE',  ( 0.000000000000000000, -10.50000000000000888, -7.500000000000007105 ) ) ;
#3703 = CARTESIAN_POINT ( 'NONE',  ( 148.1101497308104058, 3.535533905932725318, 3.535533905932725318 ) ) ;
#3704 = CARTESIAN_POINT ( 'NONE',  ( -5.999999999999963585, 3.021315404115420679E-15, -178.4136751345947971 ) ) ;
#3705 = FACE_OUTER_BOUND ( 'NONE', #2127, .T. ) ;
#3706 = CARTESIAN_POINT ( 'NONE',  ( -9.999999999999765521, -90.00000000000001421, 4.000000000000003553 ) ) ;
#3707 =( LENGTH_UNIT ( ) NAMED_UNIT ( * ) SI_UNIT ( .MILLI., .METRE. ) );
#3708 = CARTESIAN_POINT ( 'NONE',  ( 135.4710248857196859, -8.959958897678786727, 8.000000000000005329 ) ) ;
#3709 = CARTESIAN_POINT ( 'NONE',  ( 4.763139720814407951, 2.750000000000002665, -133.7500000000000284 ) ) ;
#3710 = CARTESIAN_POINT ( 'NONE',  ( 0.000000000000000000, 5.999999999999977796, -68.71132486540520290 ) ) ;
#3711 = CARTESIAN_POINT ( 'NONE',  ( -5.412658773652684552, -3.125000000000099920, -146.9330127018922383 ) ) ;
#3712 = CARTESIAN_POINT ( 'NONE',  ( 16.22617513459482552, 2.500000000000144773, -1.035533905932869425 ) ) ;
#3713 = CARTESIAN_POINT ( 'NONE',  ( 6.000000000000001776, 5.345404176511898156E-15, -178.5863248654052313 ) ) ;
#3714 = ORIENTED_EDGE ( 'NONE', *, *, #29804, .F. ) ;
#3715 = EDGE_CURVE ( 'NONE', #1086, #15338, #17134, .T. ) ;
#3716 = CARTESIAN_POINT ( 'NONE',  ( -4.763139720814407951, 2.749999999999946709, -59.75000000000002842 ) ) ;
#3717 = DIRECTION ( 'NONE',  ( -1.000000000000000000, -1.665334536937736783E-16, -2.220446049250315546E-16 ) ) ;
#3718 = CARTESIAN_POINT ( 'NONE',  ( 5.999999999999949374, 1.607695154586804565, -70.51933756729742697 ) ) ;
#3719 =( BOUNDED_CURVE ( )  B_SPLINE_CURVE ( 2, ( #25015, #5812, #22278, #22738, #29317, #8275, #6589, #27919, #29930 ),
 .UNSPECIFIED., .F., .F. ) 
 B_SPLINE_CURVE_WITH_KNOTS ( ( 3, 2, 2, 2, 3 ),
 ( 0.1305555555555555636, 0.1314814814814814770, 0.1333333333333333315, 0.1351851851851851860, 0.1361111111111110994 ),
 .UNSPECIFIED. ) 
 CURVE ( )  GEOMETRIC_REPRESENTATION_ITEM ( )  RATIONAL_B_SPLINE_CURVE ( ( 0.9330127018922194093, 0.9330127018922204085, 1.000000000000000000, 0.8660254037844388186, 1.000000000000000000, 0.8660254037844388186, 1.000000000000000000, 0.9330127018922205195, 0.9330127018922196314 ) ) 
 REPRESENTATION_ITEM ( '' )  );
#3720 = EDGE_CURVE ( 'NONE', #15258, #28330, #8648, .T. ) ;
#3721 = CARTESIAN_POINT ( 'NONE',  ( -5.196152422706573404, -3.000000000000002665, -163.2886751345948255 ) ) ;
#3722 = ORIENTED_EDGE ( 'NONE', *, *, #18431, .T. ) ;
#3723 = CARTESIAN_POINT ( 'NONE',  ( 109.3124999999999147, -1.035533905932598975, 2.500000000000265121 ) ) ;
#3724 = CARTESIAN_POINT ( 'NONE',  ( 143.4375000000000284, -4.242640687119298093, -4.242640687119298093 ) ) ;
#3725 = CARTESIAN_POINT ( 'NONE',  ( 2.775557561562891351E-14, 5.874999999999977796, -46.28349364905393060 ) ) ;
#3726 =( BOUNDED_CURVE ( )  B_SPLINE_CURVE ( 2, ( #17392, #29021, #10313, #17859, #22444, #27177, #7986, #22135, #8454 ),
 .UNSPECIFIED., .F., .T. ) 
 B_SPLINE_CURVE_WITH_KNOTS ( ( 3, 2, 2, 2, 3 ),
 ( 0.2083333333333333703, 0.2092592592592592560, 0.2111111111111111382, 0.2129629629629629095, 0.2138888888888887951 ),
 .UNSPECIFIED. ) 
 CURVE ( )  GEOMETRIC_REPRESENTATION_ITEM ( )  RATIONAL_B_SPLINE_CURVE ( ( 0.9330127018922194093, 0.9330127018922234061, 1.000000000000000000, 0.8660254037844388186, 1.000000000000000000, 0.8660254037844388186, 1.000000000000000000, 0.9330127018922234061, 0.9330127018922194093 ) ) 
 REPRESENTATION_ITEM ( '' )  );
#3727 = ORIENTED_EDGE ( 'NONE', *, *, #2046, .T. ) ;
#3728 = CARTESIAN_POINT ( 'NONE',  ( 140.9062500000000568, 6.000000000000005329, -2.485281374238555774 ) ) ;
#3729 = CARTESIAN_POINT ( 'NONE',  ( 142.6800748654051745, -2.278174593051950136, 5.500000000000074607 ) ) ;
#3730 = VERTEX_POINT ( 'NONE', #4823 ) ;
#3731 = CARTESIAN_POINT ( 'NONE',  ( 4.763139720814407951, -2.749999999999988454, -144.5000000000000284 ) ) ;
#3732 = ORIENTED_EDGE ( 'NONE', *, *, #18337, .F. ) ;
#3733 = CARTESIAN_POINT ( 'NONE',  ( 18.81250000000011013, 0.8284271247462354770, -2.000000000000091926 ) ) ;
#3734 = ORIENTED_EDGE ( 'NONE', *, *, #29061, .F. ) ;
#3735 = AXIS2_PLACEMENT_3D ( 'NONE', #30287, #27961, #6938 ) ;
#3736 = CARTESIAN_POINT ( 'NONE',  ( 4.763139720814407951, -2.749999999999988454, -71.00000000000001421 ) ) ;
#3737 = CARTESIAN_POINT ( 'NONE',  ( 13.68750000000000178, -1.097466725451499370, 2.649519052838178457 ) ) ;
#3738 = CARTESIAN_POINT ( 'NONE',  ( 3.608439182435180470, 6.249999999999982236, -93.55801270189226670 ) ) ;
#3739 = CARTESIAN_POINT ( 'NONE',  ( -9.999999999999772626, -90.00000000000001421, -3.000000000000002665 ) ) ;
#3740 = EDGE_CURVE ( 'NONE', #10931, #10419, #25540, .T. ) ;
#3741 = CARTESIAN_POINT ( 'NONE',  ( 0.000000000000000000, -5.999999999999991118, -83.53867513459483973 ) ) ;
#3742 = CARTESIAN_POINT ( 'NONE',  ( -3.464101615137757051, -5.999999999999979572, -151.1636751345947971 ) ) ;
#3743 = CARTESIAN_POINT ( 'NONE',  ( -5.196152422706601826, 2.999999999999975131, -98.46132486540520290 ) ) ;
#3744 = CARTESIAN_POINT ( 'NONE',  ( 0.000000000000000000, -5.999999999999991118, -64.96132486540523132 ) ) ;
#3745 = DIRECTION ( 'NONE',  ( 0.000000000000000000, 0.000000000000000000, 1.000000000000000000 ) ) ;
#3746 = CARTESIAN_POINT ( 'NONE',  ( 0.000000000000000000, 5.499999999999991118, -159.0000000000000284 ) ) ;
#3747 = CARTESIAN_POINT ( 'NONE',  ( 136.5863248654052313, 0.000000000000000000, 5.500000000000005329 ) ) ;
#3748 = CARTESIAN_POINT ( 'NONE',  ( 19.77382486540529172, 2.500000000000144773, 1.035533905932629173 ) ) ;
#3749 = VECTOR ( 'NONE', #22160, 1000.000000000000000 ) ;
#3750 = PRODUCT_DEFINITION_SHAPE ( 'NONE', 'NONE',  #21369 ) ;
#3751 = CARTESIAN_POINT ( 'NONE',  ( -3.175426480542816066, 5.499999999999865885, -89.87500000000001421 ) ) ;
#3752 = CIRCLE ( 'NONE', #16558, 28.99999999999999645 ) ;
#3753 = CARTESIAN_POINT ( 'NONE',  ( 104.6817643459960578, 1.849990392679531137, 0.6994407051579113466 ) ) ;
#3754 =( NAMED_UNIT ( * ) SI_UNIT ( $, .STERADIAN. ) SOLID_ANGLE_UNIT ( ) );
#3755 = CARTESIAN_POINT ( 'NONE',  ( 0.000000000000000000, 5.499999999999991118, -82.50000000000001421 ) ) ;
#3756 = EDGE_CURVE ( 'NONE', #10765, #8441, #14401, .T. ) ;
#3757 = CARTESIAN_POINT ( 'NONE',  ( 151.3273502691896510, -5.000000000000004441, 0.000000000000000000 ) ) ;
#3758 = CARTESIAN_POINT ( 'NONE',  ( 161.0000000000000284, -5.424442335930618420, -0.9085292203135086897 ) ) ;
#3759 = CARTESIAN_POINT ( 'NONE',  ( 151.5074251345948255, 2.278174593052074925, -5.499999999999950262 ) ) ;
#3760 = CARTESIAN_POINT ( 'NONE',  ( -5.999999999999963585, 1.780251999655701777E-13, -103.4136751345948255 ) ) ;
#3761 = CARTESIAN_POINT ( 'NONE',  ( 21.81250000000009592, 0.8284271247462955401, -2.000000000000151879 ) ) ;
#3762 = CARTESIAN_POINT ( 'NONE',  ( -4.999999999999990230, -55.00000000000002132, -7.500000000000007105 ) ) ;
#3763 = CARTESIAN_POINT ( 'NONE',  ( -5.999999999999971578, 1.607695154586715303, -134.4033121635129930 ) ) ;
#3764 = ORIENTED_EDGE ( 'NONE', *, *, #11537, .F. ) ;
#3765 = FACE_OUTER_BOUND ( 'NONE', #28995, .T. ) ;
#3766 = CARTESIAN_POINT ( 'NONE',  ( 135.0000000000000284, -11.07692307692306777, 4.615384615384604317 ) ) ;
#3767 = CARTESIAN_POINT ( 'NONE',  ( 117.5002832217622455, 1.308140751793696044, 1.308140751793862577 ) ) ;
#3768 = DIRECTION ( 'NONE',  ( 0.000000000000000000, 5.551115123125768527E-17, -1.000000000000000000 ) ) ;
#3769 = ORIENTED_EDGE ( 'NONE', *, *, #9184, .T. ) ;
#3770 = AXIS2_PLACEMENT_3D ( 'NONE', #2548, #21754, #538 ) ;
#3771 = AXIS2_PLACEMENT_3D ( 'NONE', #8592, #8905, #20734 ) ;
#3772 = CARTESIAN_POINT ( 'NONE',  ( -3.175426480542816510, 5.499999999999865885, -100.3750000000000000 ) ) ;
#3773 = CARTESIAN_POINT ( 'NONE',  ( -5.196152422706601826, 2.999999999999975131, -70.53867513459482552 ) ) ;
#3774 = CARTESIAN_POINT ( 'NONE',  ( 2.775557561562891351E-14, 6.250000000000033751, -118.9330127018922667 ) ) ;
#3775 = EDGE_LOOP ( 'NONE', ( #15878, #21323, #16042, #5177 ) ) ;
#3776 = CARTESIAN_POINT ( 'NONE',  ( 0.000000000000000000, 5.999999999999977796, -91.78867513459482552 ) ) ;
#3777 = CARTESIAN_POINT ( 'NONE',  ( 139.5000000000000284, -8.798545334315205579, -8.160000000000000142 ) ) ;
#3778 = EDGE_CURVE ( 'NONE', #29507, #22623, #11684, .T. ) ;
#3779 = EDGE_CURVE ( 'NONE', #7022, #10874, #16334, .T. ) ;
#3780 = CARTESIAN_POINT ( 'NONE',  ( -3.608439182435052128, -6.250000000000110134, -55.30801270189220276 ) ) ;
#3781 = ORIENTED_EDGE ( 'NONE', *, *, #28923, .T. ) ;
#3782 = DIRECTION ( 'NONE',  ( 0.000000000000000000, 0.000000000000000000, 1.000000000000000000 ) ) ;
#3783 = CARTESIAN_POINT ( 'NONE',  ( 125.0000000000000568, -55.00000000000000711, 8.000000000000007105 ) ) ;
#3784 = CARTESIAN_POINT ( 'NONE',  ( -4.763139720814407951, 2.749999999999946709, -172.2500000000000000 ) ) ;
#3785 = CARTESIAN_POINT ( 'NONE',  ( 115.4374999999997868, -2.499999999999934719, 1.035533905932929599 ) ) ;
#3786 = SURFACE_SIDE_STYLE ('',( #22555 ) ) ;
#3787 = CARTESIAN_POINT ( 'NONE',  ( -1.000000000000002220, -9.000000000000007105, 4.000000000000005329 ) ) ;
#3788 = CARTESIAN_POINT ( 'NONE',  ( 0.000000000000000000, 5.499999999999991118, -110.9999999999999858 ) ) ;
#3789 = CARTESIAN_POINT ( 'NONE',  ( 13.22617513459483618, 2.500000000000024425, -1.035533905932929599 ) ) ;
#3790 = ADVANCED_FACE ( 'NONE', ( #21276 ), #6982, .F. ) ;
#3791 = CARTESIAN_POINT ( 'NONE',  ( -4.763139720814407951, -2.750000000000016431, -107.5000000000000426 ) ) ;
#3792 = CARTESIAN_POINT ( 'NONE',  ( 135.0000000000000284, -7.797751917820416878, 7.985411280316564664 ) ) ;
#3793 = VERTEX_POINT ( 'NONE', #15124 ) ;
#3794 = CARTESIAN_POINT ( 'NONE',  ( 14.62500000000013856, 2.649519052838555933, 1.110223024625156540E-13 ) ) ;
#3795 = CARTESIAN_POINT ( 'NONE',  ( 117.5624999999997584, -2.499999999999904521, -1.035533905932508825 ) ) ;
#3796 = AXIS2_PLACEMENT_3D ( 'NONE', #26788, #17327, #16885 ) ;
#3797 = CARTESIAN_POINT ( 'NONE',  ( 110.5627832217621318, 0.7662911109079189043, 1.849990392679652151 ) ) ;
#3798 = CARTESIAN_POINT ( 'NONE',  ( -5.999999999999963585, -1.487416814333745711E-14, -134.3363248654052313 ) ) ;
#3799 = ORIENTED_EDGE ( 'NONE', *, *, #1359, .F. ) ;
#3800 = CARTESIAN_POINT ( 'NONE',  ( 139.2113248654052313, 5.500000000000005329, 0.000000000000000000 ) ) ;
#3801 = CARTESIAN_POINT ( 'NONE',  ( 3.608439182435180470, 6.249999999999982236, -79.19198729810786119 ) ) ;
#3802 = CARTESIAN_POINT ( 'NONE',  ( 3.464101615137757051, -5.999999999999979572, -102.9136751345948255 ) ) ;
#3803 = ORIENTED_EDGE ( 'NONE', *, *, #23220, .F. ) ;
#3804 = CARTESIAN_POINT ( 'NONE',  ( -5.196152422706573404, -3.000000000000002665, -75.71132486540521711 ) ) ;
#3805 = ORIENTED_EDGE ( 'NONE', *, *, #21805, .F. ) ;
#3806 = CARTESIAN_POINT ( 'NONE',  ( 154.4062500000000284, 6.000000000000005329, -2.485281374238555774 ) ) ;
#3807 = CARTESIAN_POINT ( 'NONE',  ( 4.763139720814407951, 2.750000000000002665, -124.7500000000000284 ) ) ;
#3808 =( BOUNDED_CURVE ( )  B_SPLINE_CURVE ( 2, ( #15377, #8739, #8257, #5957, #27294, #3802, #24704, #1052, #15847 ),
 .UNSPECIFIED., .F., .F. ) 
 B_SPLINE_CURVE_WITH_KNOTS ( ( 3, 2, 2, 2, 3 ),
 ( 0.5805555555555554914, 0.5814814814814814881, 0.5833333333333333703, 0.5851851851851851416, 0.5861111111111111382 ),
 .UNSPECIFIED. ) 
 CURVE ( )  GEOMETRIC_REPRESENTATION_ITEM ( )  RATIONAL_B_SPLINE_CURVE ( ( 0.9330127018922194093, 0.9330127018922154125, 1.000000000000000000, 0.8660254037844388186, 1.000000000000000000, 0.8660254037844388186, 1.000000000000000000, 0.9330127018922154125, 0.9330127018922194093 ) ) 
 REPRESENTATION_ITEM ( '' )  );
#3809 = CARTESIAN_POINT ( 'NONE',  ( 2.775557561562891351E-14, -6.250000000000061284, -142.1830127018922667 ) ) ;
#3810 = ORIENTED_EDGE ( 'NONE', *, *, #21573, .F. ) ;
#3811 = DIRECTION ( 'NONE',  ( 0.000000000000000000, -1.000000000000000000, 0.000000000000000000 ) ) ;
#3812 = CARTESIAN_POINT ( 'NONE',  ( 2.775557561562891351E-14, 6.250000000000033751, -122.5669872981078328 ) ) ;
#3813 = PRESENTATION_STYLE_ASSIGNMENT (( #23681 ) ) ;
#3814 = VECTOR ( 'NONE', #7793, 1000.000000000000000 ) ;
#3815 = CARTESIAN_POINT ( 'NONE',  ( 3.175426480543072749, 5.499999999999865885, -169.6250000000000000 ) ) ;
#3816 =( LENGTH_UNIT ( ) NAMED_UNIT ( * ) SI_UNIT ( .MILLI., .METRE. ) );
#3817 = ADVANCED_FACE ( 'NONE', ( #19863 ), #19433, .T. ) ;
#3818 = ORIENTED_EDGE ( 'NONE', *, *, #23282, .T. ) ;
#3819 = CARTESIAN_POINT ( 'NONE',  ( -40.00000000000000000, -20.00000000000021316, -3.000000000000002665 ) ) ;
#3820 = LINE ( 'NONE', #6283, #27542 ) ;
#3821 = CARTESIAN_POINT ( 'NONE',  ( -5.999999999999971578, 1.607695154586715303, -170.9806624327026157 ) ) ;
#3822 = CARTESIAN_POINT ( 'NONE',  ( 13.60117513459492145, -1.035533905932689347, 2.499999999999904521 ) ) ;
#3823 = CARTESIAN_POINT ( 'NONE',  ( 111.0002832217622597, -1.308140751793557266, -1.308140751793640533 ) ) ;
#3824 = CARTESIAN_POINT ( 'NONE',  ( -7.216878364870328078, 0.000000000000000000, -68.19198729810780435 ) ) ;
#3825 = CARTESIAN_POINT ( 'NONE',  ( -5.412658773652684552, -3.125000000000099920, -56.06698729810782567 ) ) ;
#3826 = CARTESIAN_POINT ( 'NONE',  ( 119.3363248654050324, -1.414213562373228816, -1.414213562373034527 ) ) ;
#3827 = CARTESIAN_POINT ( 'NONE',  ( -2.775557561562891351E-14, -5.500000000000115463, -48.75000000000001421 ) ) ;
#3828 = CARTESIAN_POINT ( 'NONE',  ( 119.9999999999996447, 1.338994316733504109, -1.808804601859313133 ) ) ;
#3829 = EDGE_CURVE ( 'NONE', #14180, #19519, #58, .T. ) ;
#3830 = CARTESIAN_POINT ( 'NONE',  ( 4.763139720814407951, 2.750000000000002665, -130.7500000000000284 ) ) ;
#3831 = EDGE_CURVE ( 'NONE', #18461, #16010, #3752, .T. ) ;
#3832 = CARTESIAN_POINT ( 'NONE',  ( 5.999999999999974243, 1.607695154586759934, -138.5966878364870354 ) ) ;
#3833 = CARTESIAN_POINT ( 'NONE',  ( 104.7401757384972711, -1.469686010816039889, -1.130075799885433163 ) ) ;
#3834 = ORIENTED_EDGE ( 'NONE', *, *, #9953, .F. ) ;
#3835 = CARTESIAN_POINT ( 'NONE',  ( 23.81250000000009948, 1.097466725451619718, 2.649519052838298805 ) ) ;
#3836 = CARTESIAN_POINT ( 'NONE',  ( 160.0238248654052313, 3.889087296526011706, -3.889087296526011706 ) ) ;
#3837 = CARTESIAN_POINT ( 'NONE',  ( -3.464101615137725076, 5.999999999999979572, -97.08632486540518869 ) ) ;
#3838 = CARTESIAN_POINT ( 'NONE',  ( 136.7961002691896510, 2.071067811865468400, -4.999999999999989342 ) ) ;
#3839 = ORIENTED_EDGE ( 'NONE', *, *, #24312, .T. ) ;
#3840 = CARTESIAN_POINT ( 'NONE',  ( 115.1247167782376692, -1.849990392679523588, 0.000000000000000000 ) ) ;
#3841 = CARTESIAN_POINT ( 'NONE',  ( 6.000000000000000888, -1.607695154586752384, -109.6533121635129930 ) ) ;
#3842 = CARTESIAN_POINT ( 'NONE',  ( 10.00000000000014921, 2.023458278065096039, 0.3436007916004408802 ) ) ;
#3843 = ORIENTED_EDGE ( 'NONE', *, *, #22645, .F. ) ;
#3844 = CARTESIAN_POINT ( 'NONE',  ( 0.000000000000000000, 0.000000000000000000, 0.000000000000000000 ) ) ;
#3845 = CARTESIAN_POINT ( 'NONE',  ( 141.7500000000000568, -6.000000000000005329, 0.000000000000000000 ) ) ;
#3846 = ORIENTED_EDGE ( 'NONE', *, *, #809, .T. ) ;
#3847 = PRESENTATION_STYLE_ASSIGNMENT (( #22920 ) ) ;
#3848 = FILL_AREA_STYLE ('',( #24901 ) ) ;
#3849 = DIRECTION ( 'NONE',  ( -1.000000000000000000, 0.000000000000000000, 0.000000000000000000 ) ) ;
#3850 = EDGE_CURVE ( 'NONE', #25854, #8489, #671, .T. ) ;
#3851 = CARTESIAN_POINT ( 'NONE',  ( 22.43750000000002842, -1.999999999999851674, 0.8284271247462354770 ) ) ;
#3852 = CARTESIAN_POINT ( 'NONE',  ( 0.000000000000000000, 0.000000000000000000, 0.000000000000000000 ) ) ;
#3853 = CARTESIAN_POINT ( 'NONE',  ( 6.000000000000000888, -1.859271017917181981E-14, -166.5863248654052029 ) ) ;
#3854 = CARTESIAN_POINT ( 'NONE',  ( 7.216878364870455975, -6.409875621278545621E-14, -71.30801270189220986 ) ) ;
#3855 = CARTESIAN_POINT ( 'NONE',  ( 147.2663997308104058, -4.999999999999989342, -2.071067811865468400 ) ) ;
#3856 = CARTESIAN_POINT ( 'NONE',  ( 0.000000000000000000, 0.000000000000000000, 0.000000000000000000 ) ) ;
#3857 = CARTESIAN_POINT ( 'NONE',  ( 12.41367513459484861, 1.767766952966431937, 1.767766952966209892 ) ) ;
#3858 =( BOUNDED_CURVE ( )  B_SPLINE_CURVE ( 2, ( #15504, #17641, #15660, #26964, #3776, #3921, #13350, #4080, #5925 ),
 .UNSPECIFIED., .F., .F. ) 
 B_SPLINE_CURVE_WITH_KNOTS ( ( 3, 2, 2, 2, 3 ),
 ( 0.6638888888888889728, 0.6648148148148148584, 0.6666666666666666297, 0.6685185185185185119, 0.6694444444444443976 ),
 .UNSPECIFIED. ) 
 CURVE ( )  GEOMETRIC_REPRESENTATION_ITEM ( )  RATIONAL_B_SPLINE_CURVE ( ( 0.9330127018922194093, 0.9330127018922234061, 1.000000000000000000, 0.8660254037844388186, 1.000000000000000000, 0.8660254037844388186, 1.000000000000000000, 0.9330127018922234061, 0.9330127018922194093 ) ) 
 REPRESENTATION_ITEM ( '' )  );
#3859 = ADVANCED_FACE ( 'NONE', ( #9906 ), #6219, .T. ) ;
#3860 = CARTESIAN_POINT ( 'NONE',  ( -3.175426480542816066, -5.500000000000057732, -135.8750000000000284 ) ) ;
#3861 = AXIS2_PLACEMENT_3D ( 'NONE', #23367, #7365, #12017 ) ;
#3862 = CARTESIAN_POINT ( 'NONE',  ( 2.775557561562891351E-14, -6.250000000000061284, -148.1830127018922667 ) ) ;
#3863 = CARTESIAN_POINT ( 'NONE',  ( -6.000000000000000888, 1.067854986875958443E-15, 7.560779664488942560E-35 ) ) ;
#3864 = DIRECTION ( 'NONE',  ( 1.000000000000000000, -0.000000000000000000, -0.000000000000000000 ) ) ;
#3865 = ORIENTED_EDGE ( 'NONE', *, *, #13519, .T. ) ;
#3866 = CARTESIAN_POINT ( 'NONE',  ( -4.763139720814407951, -2.750000000000016431, -65.50000000000000000 ) ) ;
#3867 = FACE_OUTER_BOUND ( 'NONE', #24961, .T. ) ;
#3868 = CARTESIAN_POINT ( 'NONE',  ( 125.0000000000000568, -55.00000000000000711, -8.000000000000007105 ) ) ;
#3869 = CARTESIAN_POINT ( 'NONE',  ( -5.999999999999962697, 3.323446944526963891E-14, -163.4136751345948539 ) ) ;
#3870 = ORIENTED_EDGE ( 'NONE', *, *, #30228, .F. ) ;
#3871 = CARTESIAN_POINT ( 'NONE',  ( 110.6249999999998437, -1.767766952966376426, -1.767766952966320915 ) ) ;
#3872 = CARTESIAN_POINT ( 'NONE',  ( 143.2500000000000568, -6.000000000000005329, 0.000000000000000000 ) ) ;
#3873 = CYLINDRICAL_SURFACE ( 'NONE', #24616, 2.000000000000012879 ) ;
#3874 = FACE_OUTER_BOUND ( 'NONE', #1463, .T. ) ;
#3875 = ORIENTED_EDGE ( 'NONE', *, *, #23559, .T. ) ;
#3876 = CARTESIAN_POINT ( 'NONE',  ( 135.6562500000000284, -6.000000000000005329, 2.485281374238555774 ) ) ;
#3877 = CARTESIAN_POINT ( 'NONE',  ( 6.000000000000000888, 7.762456499804234384E-14, -121.5863248654052455 ) ) ;
#3878 = ORIENTED_EDGE ( 'NONE', *, *, #22677, .F. ) ;
#3879 = CARTESIAN_POINT ( 'NONE',  ( -3.175426480542816510, -5.500000000000057732, -147.8750000000000284 ) ) ;
#3880 = CARTESIAN_POINT ( 'NONE',  ( 12.50000000000012257, -1.999999999999835243, 0.000000000000000000 ) ) ;
#3881 = VERTEX_POINT ( 'NONE', #14675 ) ;
#3882 = CARTESIAN_POINT ( 'NONE',  ( -2.775557561562891351E-14, -5.500000000000115463, -69.75000000000002842 ) ) ;
#3883 = ADVANCED_FACE ( 'NONE', ( #7874 ), #24455, .T. ) ;
#3884 = EDGE_CURVE ( 'NONE', #22716, #18315, #14027, .T. ) ;
#3885 = CARTESIAN_POINT ( 'NONE',  ( 5.412658773652712085, -3.125000000000086153, -93.93301270189225249 ) ) ;
#3886 = CARTESIAN_POINT ( 'NONE',  ( -5.959413262067409178, -9.246315551493122342, -24.19612909832621384 ) ) ;
#3887 = CARTESIAN_POINT ( 'NONE',  ( 141.0000000000000284, -12.00000000000001066, 4.000000000000003553 ) ) ;
#3888 = DIRECTION ( 'NONE',  ( -1.000000000000000000, -1.387778780781444413E-14, 0.000000000000000000 ) ) ;
#3889 = CARTESIAN_POINT ( 'NONE',  ( 116.0000000000000142, 0.000000000000000000, -5.500000000000000000 ) ) ;
#3890 = CARTESIAN_POINT ( 'NONE',  ( -3.464101615137757051, -5.999999999999979572, -65.08632486540523132 ) ) ;
#3891 = APPLICATION_PROTOCOL_DEFINITION ( 'draft international standard', 'automotive_design', 1998, #25767 ) ;
#3892 =( BOUNDED_CURVE ( )  B_SPLINE_CURVE ( 2, ( #27737, #25439, #4403, #13671, #9331, #9174, #27431, #18416, #16289 ),
 .UNSPECIFIED., .F., .T. ) 
 B_SPLINE_CURVE_WITH_KNOTS ( ( 3, 2, 2, 2, 3 ),
 ( 0.1138888888888888867, 0.1148148148148148140, 0.1166666666666666685, 0.1185185185185185230, 0.1194444444444444503 ),
 .UNSPECIFIED. ) 
 CURVE ( )  GEOMETRIC_REPRESENTATION_ITEM ( )  RATIONAL_B_SPLINE_CURVE ( ( 0.9330127018922194093, 0.9330127018922194093, 1.000000000000000000, 0.8660254037844388186, 1.000000000000000000, 0.8660254037844388186, 1.000000000000000000, 0.9330127018922189652, 0.9330127018922194093 ) ) 
 REPRESENTATION_ITEM ( '' )  );
#3893 = CARTESIAN_POINT ( 'NONE',  ( -4.763139720814407951, -2.750000000000016431, -154.0000000000000284 ) ) ;
#3894 = DIRECTION ( 'NONE',  ( 1.000000000000000000, -5.551115123125773458E-17, -1.260129944081490338E-35 ) ) ;
#3895 = CARTESIAN_POINT ( 'NONE',  ( -0.5896198263027827569, 5.540201351793362150, -180.0000000000000853 ) ) ;
#3896 = VECTOR ( 'NONE', #6096, 1000.000000000000000 ) ;
#3897 = CARTESIAN_POINT ( 'NONE',  ( -2.775557561562891351E-14, -5.500000000000115463, -84.74999999999998579 ) ) ;
#3898 = CARTESIAN_POINT ( 'NONE',  ( 0.000000000000000000, -5.999999999999991118, -140.5386751345948255 ) ) ;
#3899 = FACE_OUTER_BOUND ( 'NONE', #20079, .T. ) ;
#3900 = CARTESIAN_POINT ( 'NONE',  ( 3.175426480543072749, -5.500000000000105693, -71.12500000000004263 ) ) ;
#3901 = AXIS2_PLACEMENT_3D ( 'NONE', #12409, #12858, #694 ) ;
#3902 = CARTESIAN_POINT ( 'NONE',  ( 154.6086002691896510, -2.071067811865468400, -4.999999999999989342 ) ) ;
#3903 = DIRECTION ( 'NONE',  ( 1.000000000000000000, -5.551115123125773458E-17, -1.260129944081490338E-35 ) ) ;
#3904 = CARTESIAN_POINT ( 'NONE',  ( 1.110223024625164183E-16, -2.000000000000012879, -1.776356839400262692E-15 ) ) ;
#3905 = CIRCLE ( 'NONE', #22576, 9.999999999999998224 ) ;
#3906 = CARTESIAN_POINT ( 'NONE',  ( 114.5863248654051887, 1.414213562373145550, -1.414213562373145550 ) ) ;
#3907 = CARTESIAN_POINT ( 'NONE',  ( 0.000000000000000000, 5.999999999999977796, -55.21132486540525264 ) ) ;
#3908 = CARTESIAN_POINT ( 'NONE',  ( 150.7425748654052313, -2.278174593052229469, -5.499999999999796607 ) ) ;
#3909 = DIRECTION ( 'NONE',  ( 0.000000000000000000, -1.000000000000000000, 0.000000000000000000 ) ) ;
#3910 = ORIENTED_EDGE ( 'NONE', *, *, #19622, .F. ) ;
#3911 = CARTESIAN_POINT ( 'NONE',  ( 153.9375000000000284, -4.242640687119298093, -4.242640687119298093 ) ) ;
#3912 = FACE_OUTER_BOUND ( 'NONE', #18123, .T. ) ;
#3913 = CARTESIAN_POINT ( 'NONE',  ( 24.86659270085223739, 0.5400564011831616718, -2.082004388006507778 ) ) ;
#3914 = ORIENTED_EDGE ( 'NONE', *, *, #19067, .T. ) ;
#3915 = ORIENTED_EDGE ( 'NONE', *, *, #12634, .F. ) ;
#3916 = CARTESIAN_POINT ( 'NONE',  ( -2.775557561562891351E-14, -5.500000000000115463, -93.75000000000000000 ) ) ;
#3917 = CARTESIAN_POINT ( 'NONE',  ( -5.999999999999963585, 1.780251999655701777E-13, -70.41367513459482552 ) ) ;
#3918 = EDGE_CURVE ( 'NONE', #4112, #15998, #11871, .T. ) ;
#3919 = CARTESIAN_POINT ( 'NONE',  ( -5.412658773652739619, 3.124999999999975131, -114.1830127018922383 ) ) ;
#3920 = ORIENTED_EDGE ( 'NONE', *, *, #11751, .F. ) ;
#3921 = CARTESIAN_POINT ( 'NONE',  ( -3.464101615137725076, 5.999999999999979572, -91.66367513459485394 ) ) ;
#3922 = FACE_OUTER_BOUND ( 'NONE', #17373, .T. ) ;
#3923 = CARTESIAN_POINT ( 'NONE',  ( 5.196152422706629359, -2.999999999999988898, -143.2886751345948255 ) ) ;
#3924 = AXIS2_PLACEMENT_3D ( 'NONE', #28870, #1078, #24421 ) ;
#3925 = CARTESIAN_POINT ( 'NONE',  ( -7.216878364870328078, 0.000000000000000000, -51.05801270189225249 ) ) ;
#3926 = ORIENTED_EDGE ( 'NONE', *, *, #20453, .T. ) ;
#3927 = LINE ( 'NONE', #1637, #3896 ) ;
#3928 = CARTESIAN_POINT ( 'NONE',  ( -3.464101615137757051, -5.999999999999979572, -62.08632486540521711 ) ) ;
#3929 = CARTESIAN_POINT ( 'NONE',  ( -4.763139720814407951, -2.750000000000016431, -161.5000000000000284 ) ) ;
#3930 = CARTESIAN_POINT ( 'NONE',  ( 116.8124999999998010, 1.035533905932719101, -2.499999999999784173 ) ) ;
#3931 = CARTESIAN_POINT ( 'NONE',  ( 0.000000000000000000, 5.999999999999977796, -107.7113248654052455 ) ) ;
#3932 = CARTESIAN_POINT ( 'NONE',  ( 23.71132486540528106, 2.500000000000168754, -1.110223024625156540E-13 ) ) ;
#3933 = CARTESIAN_POINT ( 'NONE',  ( -4.763139720814407951, -2.750000000000016431, -94.00000000000002842 ) ) ;
#3934 = CARTESIAN_POINT ( 'NONE',  ( -5.196152422706601826, 2.999999999999975131, -151.5386751345948539 ) ) ;
#3935 = FILL_AREA_STYLE ('',( #10588 ) ) ;
#3936 = CARTESIAN_POINT ( 'NONE',  ( -5.196152422706573404, -3.000000000000002665, -82.28867513459481131 ) ) ;
#3937 = EDGE_LOOP ( 'NONE', ( #2254, #7187, #22109 ) ) ;
#3938 = CARTESIAN_POINT ( 'NONE',  ( 15.06250000000013323, -2.649519052838178457, 1.097466725451439196 ) ) ;
#3939 = CARTESIAN_POINT ( 'NONE',  ( 117.4999999999999574, -2.499999999999891198, 0.000000000000000000 ) ) ;
#3940 = MECHANICAL_DESIGN_GEOMETRIC_PRESENTATION_REPRESENTATION (  '', ( #23108 ), #15786 ) ;
#3941 = CARTESIAN_POINT ( 'NONE',  ( 111.1252832217622597, -5.551115123125782702E-14, -1.849990392679523588 ) ) ;
#3942 = TOROIDAL_SURFACE ( 'NONE', #12833, 10.49999999999998934, 0.5000000000000000000 ) ;
#3943 = ORIENTED_EDGE ( 'NONE', *, *, #17363, .F. ) ;
#3944 = CARTESIAN_POINT ( 'NONE',  ( 4.763139720814407951, 2.750000000000002665, -162.2500000000000000 ) ) ;
#3945 = CARTESIAN_POINT ( 'NONE',  ( 6.000000000000000888, -1.859271017917181981E-14, -169.5863248654052029 ) ) ;
#3946 = CARTESIAN_POINT ( 'NONE',  ( 108.9372167782374987, -0.7662911109077087390, 1.849990392679591977 ) ) ;
#3947 = CONICAL_SURFACE ( 'NONE', #4922, 1000.000000000000682, 0.7853981633974479459 ) ;
#3948 = ADVANCED_FACE ( 'NONE', ( #25068 ), #6190, .T. ) ;
#3949 = CARTESIAN_POINT ( 'NONE',  ( -5.412658773652684552, -3.125000000000099920, -87.56698729810786119 ) ) ;
#3950 = LINE ( 'NONE', #27150, #20502 ) ;
#3951 = VERTEX_POINT ( 'NONE', #26903 ) ;
#3952 = CARTESIAN_POINT ( 'NONE',  ( -2.691259848637789442, 10.67213569177517840, -30.37695071776534661 ) ) ;
#3953 = VECTOR ( 'NONE', #20634, 1000.000000000000000 ) ;
#3954 = ORIENTED_EDGE ( 'NONE', *, *, #21438, .F. ) ;
#3955 = ORIENTED_EDGE ( 'NONE', *, *, #12405, .T. ) ;
#3956 = CARTESIAN_POINT ( 'NONE',  ( 158.9062500000000284, 6.000000000000005329, -2.485281374238555774 ) ) ;
#3957 = CARTESIAN_POINT ( 'NONE',  ( 3.175426480543072749, 5.499999999999865885, -123.1250000000000426 ) ) ;
#3958 = EDGE_CURVE ( 'NONE', #28373, #16384, #1205, .T. ) ;
#3959 = VERTEX_POINT ( 'NONE', #24919 ) ;
#3960 = CARTESIAN_POINT ( 'NONE',  ( 140.0769230769231228, -11.53846153846155254, -4.615384615384604317 ) ) ;
#3961 = CARTESIAN_POINT ( 'NONE',  ( 3.608439182435180470, 6.249999999999982236, -121.1919872981077901 ) ) ;
#3962 = CARTESIAN_POINT ( 'NONE',  ( -5.412658773652684552, -3.125000000000099920, -174.5669872981078186 ) ) ;
#3963 = CARTESIAN_POINT ( 'NONE',  ( 3.175426480543072749, 5.499999999999865885, -172.6250000000000000 ) ) ;
#3964 = CARTESIAN_POINT ( 'NONE',  ( 159.3293511854687949, -12.04413325411710467, 3.946525873397269457 ) ) ;
#3965 = CARTESIAN_POINT ( 'NONE',  ( 20.39882486540528816, -1.035533905932689347, -2.499999999999904521 ) ) ;
#3966 = AXIS2_PLACEMENT_3D ( 'NONE', #3243, #946, #17730 ) ;
#3967 = VERTEX_POINT ( 'NONE', #15606 ) ;
#3968 = CARTESIAN_POINT ( 'NONE',  ( 11.25000000000001066, 1.110223024625156540E-13, 1.999999999999946265 ) ) ;
#3969 = DIRECTION ( 'NONE',  ( -1.000000000000000000, 0.000000000000000000, 0.000000000000000000 ) ) ;
#3970 = CARTESIAN_POINT ( 'NONE',  ( 5.196152422706629359, -2.999999999999988898, -117.2113248654052029 ) ) ;
#3971 = CARTESIAN_POINT ( 'NONE',  ( 125.0000000000000568, -55.00000000000000711, 4.000000000000003553 ) ) ;
#3972 = AXIS2_PLACEMENT_3D ( 'NONE', #4867, #30377, #16449 ) ;
#3973 = CARTESIAN_POINT ( 'NONE',  ( 112.6488248654049045, 2.000000000000061728, -0.8284271247459952248 ) ) ;
#3974 = CARTESIAN_POINT ( 'NONE',  ( 113.1877832217620892, 0.7662911109079189043, -1.849990392679291551 ) ) ;
#3975 = CARTESIAN_POINT ( 'NONE',  ( -3.608439182435115633, 6.249999999999965361, -69.94198729810781856 ) ) ;
#3976 = CARTESIAN_POINT ( 'NONE',  ( 2.775557561562891351E-14, -6.250000000000061284, -54.31698729810785409 ) ) ;
#3977 = CARTESIAN_POINT ( 'NONE',  ( -5.999999999999919176, 1.607695154586804565, -110.4033121635129788 ) ) ;
#3978 = CARTESIAN_POINT ( 'NONE',  ( 6.350852961086080661, -9.614813431917819062E-14, -46.87500000000000000 ) ) ;
#3979 = CARTESIAN_POINT ( 'NONE',  ( 119.9999999999998153, -0.1589013571467045582, -2.047736629971486977 ) ) ;
#3980 = CARTESIAN_POINT ( 'NONE',  ( 0.000000000000000000, -5.999999999999991118, -153.4613248654052029 ) ) ;
#3981 = CARTESIAN_POINT ( 'NONE',  ( -4.763139720814407951, 2.749999999999946709, -131.7500000000000284 ) ) ;
#3982 = DIRECTION ( 'NONE',  ( 0.000000000000000000, 0.000000000000000000, -1.000000000000000000 ) ) ;
#3983 = ORIENTED_EDGE ( 'NONE', *, *, #3430, .F. ) ;
#3984 = CARTESIAN_POINT ( 'NONE',  ( 3.464101615137852974, 5.999999999999884537, -157.9136751345947971 ) ) ;
#3985 = DIRECTION ( 'NONE',  ( -7.147005652999508048E-36, 5.642372883946980038E-36, 1.000000000000000000 ) ) ;
#3986 = FACE_OUTER_BOUND ( 'NONE', #3641, .T. ) ;
#3987 =( BOUNDED_CURVE ( )  B_SPLINE_CURVE ( 2, ( #21009, #14130, #29888, #95, #16426, #18864, #28037, #2261, #11351 ),
 .UNSPECIFIED., .F., .F. ) 
 B_SPLINE_CURVE_WITH_KNOTS ( ( 3, 2, 2, 2, 3 ),
 ( 0.1250000000000000000, 0.1259259259259258856, 0.1277777777777777679, 0.1296296296296296502, 0.1305555555555556468 ),
 .UNSPECIFIED. ) 
 CURVE ( )  GEOMETRIC_REPRESENTATION_ITEM ( )  RATIONAL_B_SPLINE_CURVE ( ( 0.9330127018922194093, 0.9330127018922194093, 1.000000000000000000, 0.8660254037844388186, 1.000000000000000000, 0.8660254037844388186, 1.000000000000000000, 0.9330127018922154125, 0.9330127018922194093 ) ) 
 REPRESENTATION_ITEM ( '' )  );
#3988 = CARTESIAN_POINT ( 'NONE',  ( 137.7336002691896510, -4.999999999999989342, 2.071067811865468400 ) ) ;
#3989 = ORIENTED_EDGE ( 'NONE', *, *, #21467, .T. ) ;
#3990 = CARTESIAN_POINT ( 'NONE',  ( 109.1872167782375413, -1.849990392679441875, -0.7662911109077087390 ) ) ;
#3991 = SURFACE_SIDE_STYLE ('',( #15576 ) ) ;
#3992 = CARTESIAN_POINT ( 'NONE',  ( 9.875000000000023093, 1.414213562373201061, -1.414213562373090038 ) ) ;
#3993 = ADVANCED_FACE ( 'NONE', ( #29367 ), #5867, .F. ) ;
#3994 = CARTESIAN_POINT ( 'NONE',  ( -5.412658773652684552, -3.125000000000099920, -114.5669872981078186 ) ) ;
#3995 = CIRCLE ( 'NONE', #17759, 11.00000000000001599 ) ;
#3996 = CARTESIAN_POINT ( 'NONE',  ( 135.0000000000000284, 3.979704198237310919, -4.051284705845048961 ) ) ;
#3997 =( BOUNDED_CURVE ( )  B_SPLINE_CURVE ( 2, ( #2650, #24003, #19414, #345, #18976, #9586, #14521, #12226, #28145 ),
 .UNSPECIFIED., .F., .T. ) 
 B_SPLINE_CURVE_WITH_KNOTS ( ( 3, 2, 2, 2, 3 ),
 ( 0.4861111111111111049, 0.4870370370370370461, 0.4888888888888888729, 0.4907407407407407551, 0.4916666666666666408 ),
 .UNSPECIFIED. ) 
 CURVE ( )  GEOMETRIC_REPRESENTATION_ITEM ( )  RATIONAL_B_SPLINE_CURVE ( ( 0.9330127018922194093, 0.9330127018922194093, 1.000000000000000000, 0.8660254037844388186, 1.000000000000000000, 0.8660254037844388186, 1.000000000000000000, 0.9330127018922214077, 0.9330127018922194093 ) ) 
 REPRESENTATION_ITEM ( '' )  );
#3998 = DIRECTION ( 'NONE',  ( 1.000000000000000000, 0.000000000000000000, 0.000000000000000000 ) ) ;
#3999 = ORIENTED_EDGE ( 'NONE', *, *, #21874, .T. ) ;
#4000 = CARTESIAN_POINT ( 'NONE',  ( 159.8141916148839812, -12.30834012067592020, 3.594214859449901933 ) ) ;
#4001 = CARTESIAN_POINT ( 'NONE',  ( 141.2812500000000284, 2.485281374238585972, 6.000000000000005329 ) ) ;
#4002 = MANIFOLD_SOLID_BREP ( 'Cut-Sweep1', #29107 ) ;
#4003 = EDGE_CURVE ( 'NONE', #17334, #2061, #10672, .T. ) ;
#4004 = VERTEX_POINT ( 'NONE', #2201 ) ;
#4005 = ORIENTED_EDGE ( 'NONE', *, *, #16747, .T. ) ;
#4006 = CIRCLE ( 'NONE', #12889, 0.5000000000000004441 ) ;
#4007 = VECTOR ( 'NONE', #11154, 1000.000000000000000 ) ;
#4008 = CARTESIAN_POINT ( 'NONE',  ( -2.775557561562891351E-14, -5.500000000000115463, -51.75000000000002132 ) ) ;
#4009 = CARTESIAN_POINT ( 'NONE',  ( 22.18750000000018119, 0.8284271247464156662, 1.999999999999971800 ) ) ;
#4010 = SURFACE_STYLE_USAGE ( .BOTH. , #2027 ) ;
#4011 = CARTESIAN_POINT ( 'NONE',  ( 140.0000000000000284, -10.00000000000000888, 7.500000000000007105 ) ) ;
#4012 = CARTESIAN_POINT ( 'NONE',  ( 3.608439182435180470, 6.249999999999982236, -69.55801270189228092 ) ) ;
#4013 = CARTESIAN_POINT ( 'NONE',  ( 151.2976497308104058, 0.000000000000000000, 5.000000000000004441 ) ) ;
#4014 = DIRECTION ( 'NONE',  ( 0.000000000000000000, -5.551115123125767911E-17, 1.000000000000000000 ) ) ;
#4015 = FACE_OUTER_BOUND ( 'NONE', #28181, .T. ) ;
#4016 = DIRECTION ( 'NONE',  ( 0.000000000000000000, -1.000000000000000000, 0.000000000000000000 ) ) ;
#4017 = CARTESIAN_POINT ( 'NONE',  ( 16.53867513459489302, 5.551115123125782702E-14, 2.500000000000002220 ) ) ;
#4018 = CARTESIAN_POINT ( 'NONE',  ( -3.175426480542816066, -5.500000000000057732, -131.3750000000000284 ) ) ;
#4019 = CARTESIAN_POINT ( 'NONE',  ( 3.608439182435180470, 6.249999999999982236, -143.0580127018922667 ) ) ;
#4020 = CARTESIAN_POINT ( 'NONE',  ( 16.53867513459489302, 5.551115123125782702E-14, 2.500000000000002220 ) ) ;
#4021 = EDGE_LOOP ( 'NONE', ( #21601, #2613, #13305 ) ) ;
#4022 = CARTESIAN_POINT ( 'NONE',  ( -3.175426480542816066, -5.500000000000057732, -63.87500000000001421 ) ) ;
#4023 = DIRECTION ( 'NONE',  ( -7.147005652999508048E-36, 5.642372883946980038E-36, 1.000000000000000000 ) ) ;
#4024 = CARTESIAN_POINT ( 'NONE',  ( 6.000000000000000888, 1.743066579297358182E-13, -76.58632486540521711 ) ) ;
#4025 = CARTESIAN_POINT ( 'NONE',  ( -19.49999999999998224, -24.99999999999999289, 7.500000000000007105 ) ) ;
#4026 = VERTEX_POINT ( 'NONE', #2637 ) ;
#4027 = CARTESIAN_POINT ( 'NONE',  ( 108.3749999999998437, -1.767766952966209892, 1.767766952966431937 ) ) ;
#4028 = CARTESIAN_POINT ( 'NONE',  ( 147.3750000000000284, 0.000000000000000000, 6.000000000000005329 ) ) ;
#4029 = DIRECTION ( 'NONE',  ( 6.938893903907221278E-15, -1.000000000000000000, 0.000000000000000000 ) ) ;
#4030 = CIRCLE ( 'NONE', #4989, 0.5000000000000004441 ) ;
#4031 = EDGE_CURVE ( 'NONE', #21964, #25175, #11455, .T. ) ;
#4032 = ORIENTED_EDGE ( 'NONE', *, *, #28023, .F. ) ;
#4033 = CARTESIAN_POINT ( 'NONE',  ( 137.4375000000000568, -4.242640687119298093, -4.242640687119298093 ) ) ;
#4034 = PLANE ( 'NONE',  #21496 ) ;
#4035 = SHAPE_REPRESENTATION ( 'Handle', ( #18805 ), #1104 ) ;
#4036 = ORIENTED_EDGE ( 'NONE', *, *, #23880, .F. ) ;
#4037 = EDGE_CURVE ( 'NONE', #6912, #8542, #14215, .T. ) ;
#4038 = CARTESIAN_POINT ( 'NONE',  ( 3.175426480543072749, 5.499999999999865885, -144.1250000000000000 ) ) ;
#4039 = CARTESIAN_POINT ( 'NONE',  ( 12.43750000000010836, -1.999999999999851674, 0.8284271247462955401 ) ) ;
#4040 = VERTEX_POINT ( 'NONE', #20644 ) ;
#4041 = CARTESIAN_POINT ( 'NONE',  ( -2.775557561562891351E-14, -5.500000000000115463, -75.75000000000004263 ) ) ;
#4042 = CARTESIAN_POINT ( 'NONE',  ( -6.000000000000000888, 1.067854986875958443E-15, 7.560779664488942560E-35 ) ) ;
#4043 = CARTESIAN_POINT ( 'NONE',  ( -5.412658773652684552, -3.125000000000099920, -88.43301270189223828 ) ) ;
#4044 = ORIENTED_EDGE ( 'NONE', *, *, #2521, .T. ) ;
#4045 = CARTESIAN_POINT ( 'NONE',  ( -0.4044047236350920005, -11.00000000000001243, -31.00000000000003908 ) ) ;
#4046 = CARTESIAN_POINT ( 'NONE',  ( -6.000000000000007105, -1.607695154586655129, -83.84668783648703538 ) ) ;
#4047 = DIRECTION ( 'NONE',  ( -7.147005652999508048E-36, 5.642372883946980038E-36, 1.000000000000000000 ) ) ;
#4048 = CARTESIAN_POINT ( 'NONE',  ( 140.5000000000000284, 0.000000000000000000, 0.000000000000000000 ) ) ;
#4049 = DIRECTION ( 'NONE',  ( 5.740823738863761535E-21, -0.9186787455452134488, -0.3950055220923793797 ) ) ;
#4050 = CARTESIAN_POINT ( 'NONE',  ( -4.763139720814407951, -2.750000000000016431, -158.5000000000000284 ) ) ;
#4051 = LINE ( 'NONE', #22973, #4007 ) ;
#4052 = LINE ( 'NONE', #30019, #17923 ) ;
#4053 = CARTESIAN_POINT ( 'NONE',  ( 0.000000000000000000, 5.499999999999991118, -88.50000000000002842 ) ) ;
#4054 = CARTESIAN_POINT ( 'NONE',  ( 104.2497167782374845, -1.308140751793640533, -1.308140751793640533 ) ) ;
#4055 = CYLINDRICAL_SURFACE ( 'NONE', #20513, 5.500000000000000000 ) ;
#4056 = CARTESIAN_POINT ( 'NONE',  ( -3.175426480542816510, 5.499999999999865885, -70.37500000000004263 ) ) ;
#4057 = AXIS2_PLACEMENT_3D ( 'NONE', #27772, #11396, #11554 ) ;
#4058 = CARTESIAN_POINT ( 'NONE',  ( 148.7961002691896510, 2.071067811865468400, -4.999999999999989342 ) ) ;
#4059 = CARTESIAN_POINT ( 'NONE',  ( 5.196152422706629359, 3.000000000000002665, -164.9613248654052029 ) ) ;
#4060 = CARTESIAN_POINT ( 'NONE',  ( 6.000000000000000888, -3.330669073875464691E-16, -7.560779664488942560E-35 ) ) ;
#4061 = CARTESIAN_POINT ( 'NONE',  ( 114.2738248654049045, -1.999999999999941602, -0.8284271247459350507 ) ) ;
#4062 = CARTESIAN_POINT ( 'NONE',  ( 20.06250000000006395, 2.000000000000151879, 0.8284271247461753029 ) ) ;
#4063 = DIRECTION ( 'NONE',  ( 1.000000000000000000, 1.067522139062651904E-16, -0.000000000000000000 ) ) ;
#4064 = EDGE_CURVE ( 'NONE', #11180, #6328, #20956, .T. ) ;
#4065 = FACE_OUTER_BOUND ( 'NONE', #11416, .T. ) ;
#4066 = CARTESIAN_POINT ( 'NONE',  ( 161.0000000000000284, 0.000000000000000000, 0.000000000000000000 ) ) ;
#4067 = EDGE_CURVE ( 'NONE', #15286, #18931, #28652, .T. ) ;
#4068 = ORIENTED_EDGE ( 'NONE', *, *, #27920, .F. ) ;
#4069 = PRODUCT_RELATED_PRODUCT_CATEGORY ( 'part', '', ( #6978 ) ) ;
#4070 = CARTESIAN_POINT ( 'NONE',  ( 156.8437500000000284, -6.000000000000005329, -2.485281374238555774 ) ) ;
#4071 = DIRECTION ( 'NONE',  ( 1.000000000000000000, -5.551115123125774690E-17, 0.000000000000000000 ) ) ;
#4072 = CARTESIAN_POINT ( 'NONE',  ( 118.5002832217622171, 1.308140751793723799, 1.308140751793862577 ) ) ;
#4073 = CARTESIAN_POINT ( 'NONE',  ( -6.000000000000023093, 1.607695154586625819, -156.9033121635130215 ) ) ;
#4074 = VERTEX_POINT ( 'NONE', #7100 ) ;
#4075 = VERTEX_POINT ( 'NONE', #11916 ) ;
#4076 = CARTESIAN_POINT ( 'NONE',  ( 3.175426480543072749, -5.500000000000105693, -96.62500000000004263 ) ) ;
#4077 = CARTESIAN_POINT ( 'NONE',  ( 6.000000000000000888, -3.330669073875464691E-16, -7.560779664488942560E-35 ) ) ;
#4078 =( BOUNDED_CURVE ( )  B_SPLINE_CURVE ( 2, ( #3607, #12429, #12581, #21923, #15170, #14864, #1311, #8218, #26503 ),
 .UNSPECIFIED., .F., .T. ) 
 B_SPLINE_CURVE_WITH_KNOTS ( ( 3, 2, 2, 2, 3 ),
 ( 0.2527777777777777679, 0.2537037037037036535, 0.2555555555555555358, 0.2574074074074074181, 0.2583333333333333037 ),
 .UNSPECIFIED. ) 
 CURVE ( )  GEOMETRIC_REPRESENTATION_ITEM ( )  RATIONAL_B_SPLINE_CURVE ( ( 0.9330127018922194093, 0.9330127018922194093, 1.000000000000000000, 0.8660254037844388186, 1.000000000000000000, 0.8660254037844388186, 1.000000000000000000, 0.9330127018922234061, 0.9330127018922194093 ) ) 
 REPRESENTATION_ITEM ( '' )  );
#4079 = CARTESIAN_POINT ( 'NONE',  ( 3.608439182435180470, -6.249999999999997335, -106.0580127018922525 ) ) ;
#4080 = CARTESIAN_POINT ( 'NONE',  ( -5.999999999999919176, 1.607695154586804565, -91.48066243270262987 ) ) ;
#4081 = CARTESIAN_POINT ( 'NONE',  ( 0.000000000000000000, 0.000000000000000000, 0.000000000000000000 ) ) ;
#4082 =( GEOMETRIC_REPRESENTATION_CONTEXT ( 3 ) GLOBAL_UNCERTAINTY_ASSIGNED_CONTEXT ( ( #19186 ) ) GLOBAL_UNIT_ASSIGNED_CONTEXT ( ( #18415, #21310, #25438 ) ) REPRESENTATION_CONTEXT ( 'NONE', 'WORKASPACE' ) );
#4083 = CARTESIAN_POINT ( 'NONE',  ( 0.7669223171414760731, -15.58766199952932396, 7.954545454545463912 ) ) ;
#4084 = CARTESIAN_POINT ( 'NONE',  ( 3.175426480543072749, -5.500000000000105693, -164.1249999999999716 ) ) ;
#4085 = CARTESIAN_POINT ( 'NONE',  ( 2.775557561562891351E-14, 6.250000000000033751, -51.43301270189226670 ) ) ;
#4086 = DIRECTION ( 'NONE',  ( 0.000000000000000000, 0.000000000000000000, -1.000000000000000000 ) ) ;
#4087 = ORIENTED_EDGE ( 'NONE', *, *, #15454, .F. ) ;
#4088 = CARTESIAN_POINT ( 'NONE',  ( -9.999999999999998224, 1.868746227032927028E-15, -44.99152654425658682 ) ) ;
#4089 = DIRECTION ( 'NONE',  ( -1.000000000000000000, -1.067522139062651904E-16, 0.000000000000000000 ) ) ;
#4090 = CARTESIAN_POINT ( 'NONE',  ( -5.196152422706573404, -3.000000000000002665, -62.21132486540520290 ) ) ;
#4091 = CARTESIAN_POINT ( 'NONE',  ( -3.175426480542816510, -5.500000000000057732, -159.8750000000000284 ) ) ;
#4092 = CARTESIAN_POINT ( 'NONE',  ( 117.9374999999998721, 2.500000000000114575, -1.035533905932448873 ) ) ;
#4093 = DIRECTION ( 'NONE',  ( -7.147005652999508048E-36, 5.642372883946980038E-36, 1.000000000000000000 ) ) ;
#4094 = CARTESIAN_POINT ( 'NONE',  ( -3.175426480542816066, 5.499999999999865885, -110.8750000000000426 ) ) ;
#4095 = DIRECTION ( 'NONE',  ( -1.000000000000000000, -1.665334536937736783E-16, -2.220446049250315546E-16 ) ) ;
#4096 = DIRECTION ( 'NONE',  ( 5.551115123125783935E-17, -1.000000000000000000, -8.881784197001254296E-16 ) ) ;
#4097 = CARTESIAN_POINT ( 'NONE',  ( -3.175426480542816510, -5.500000000000057732, -93.87500000000002842 ) ) ;
#4098 = CARTESIAN_POINT ( 'NONE',  ( 161.0773502691896510, 5.000000000000004441, 0.000000000000000000 ) ) ;
#4099 = SURFACE_STYLE_FILL_AREA ( #3935 ) ;
#4100 = CARTESIAN_POINT ( 'NONE',  ( -0.08258755314531825154, -15.14553112961706560, 7.837970064863971409 ) ) ;
#4101 = ORIENTED_EDGE ( 'NONE', *, *, #17077, .F. ) ;
#4102 = CARTESIAN_POINT ( 'NONE',  ( 11.93750000000005507, -1.097466725451379244, 2.649519052838238409 ) ) ;
#4103 = CARTESIAN_POINT ( 'NONE',  ( 117.0624999999998579, 2.500000000000234479, 1.035533905932989551 ) ) ;
#4104 = CARTESIAN_POINT ( 'NONE',  ( 111.0627832217621602, -0.7662911109077987781, -1.849990392679291551 ) ) ;
#4105 = CARTESIAN_POINT ( 'NONE',  ( 108.1488248654049755, -2.000000000000001776, 0.8284271247464157772 ) ) ;
#4106 = EDGE_CURVE ( 'NONE', #4711, #16677, #8966, .T. ) ;
#4107 = ORIENTED_EDGE ( 'NONE', *, *, #6430, .F. ) ;
#4108 = CARTESIAN_POINT ( 'NONE',  ( 2.775557561562891351E-14, 6.250000000000033751, -89.56698729810786119 ) ) ;
#4109 = CARTESIAN_POINT ( 'NONE',  ( 116.0000000000000142, 0.000000000000000000, -5.500000000000000000 ) ) ;
#4110 = ORIENTED_EDGE ( 'NONE', *, *, #3068, .T. ) ;
#4111 = DIRECTION ( 'NONE',  ( -0.9230769230769190203, 0.000000000000000000, -0.3846153846153945177 ) ) ;
#4112 = VERTEX_POINT ( 'NONE', #27672 ) ;
#4113 = CARTESIAN_POINT ( 'NONE',  ( 157.5000000000000284, 6.000000000000005329, 0.000000000000000000 ) ) ;
#4114 = ORIENTED_EDGE ( 'NONE', *, *, #17047, .F. ) ;
#4115 = CARTESIAN_POINT ( 'NONE',  ( -4.763139720814407951, -2.750000000000016431, -118.0000000000000000 ) ) ;
#4116 = CARTESIAN_POINT ( 'NONE',  ( 10.31249999999998934, -0.8284271247461753029, 1.999999999999911626 ) ) ;
#4117 = CARTESIAN_POINT ( 'NONE',  ( -3.608439182435115633, 6.249999999999965361, -141.3080127018922099 ) ) ;
#4118 = ORIENTED_EDGE ( 'NONE', *, *, #26758, .T. ) ;
#4119 = CARTESIAN_POINT ( 'NONE',  ( 6.000000000000000888, 1.743066579297358182E-13, -57.66367513459481842 ) ) ;
#4120 = CARTESIAN_POINT ( 'NONE',  ( 5.412658773652739619, 3.124999999999988898, -124.3169872981078043 ) ) ;
#4121 = CARTESIAN_POINT ( 'NONE',  ( 3.608439182435180470, 6.249999999999982236, -178.1919872981078470 ) ) ;
#4122 = CARTESIAN_POINT ( 'NONE',  ( 159.9946976994248757, -11.54806779403923045, 3.290164197027113602 ) ) ;
#4123 =( LENGTH_UNIT ( ) NAMED_UNIT ( * ) SI_UNIT ( .MILLI., .METRE. ) );
#4124 = VERTEX_POINT ( 'NONE', #25989 ) ;
#4125 = CARTESIAN_POINT ( 'NONE',  ( 12.62500000000013678, -1.414213562372979016, -1.414213562373145550 ) ) ;
#4126 = CYLINDRICAL_SURFACE ( 'NONE', #5875, 6.000000000000000888 ) ;
#4127 = CARTESIAN_POINT ( 'NONE',  ( 159.0000000000000284, -12.00000000000000000, -4.000000000000002665 ) ) ;
#4128 = DIRECTION ( 'NONE',  ( 1.000000000000000000, 0.000000000000000000, 0.000000000000000000 ) ) ;
#4129 = DIRECTION ( 'NONE',  ( -1.000000000000000000, -1.665334536937731113E-16, 1.526556658859586792E-16 ) ) ;
#4130 = CARTESIAN_POINT ( 'NONE',  ( 111.4377832217621744, 1.849990392679532247, 0.7662911109078888172 ) ) ;
#4131 = CARTESIAN_POINT ( 'NONE',  ( -7.216878364870328078, 0.000000000000000000, -74.19198729810783277 ) ) ;
#4132 = CARTESIAN_POINT ( 'NONE',  ( 3.608439182435180470, -6.249999999999997335, -63.19198729810784698 ) ) ;
#4133 = EDGE_CURVE ( 'NONE', #17999, #13456, #16071, .T. ) ;
#4134 = CARTESIAN_POINT ( 'NONE',  ( 6.000000000000000888, -1.859271017917181981E-14, -170.1636751345948539 ) ) ;
#4135 = CARTESIAN_POINT ( 'NONE',  ( 4.763139720814407951, 2.750000000000002665, -49.75000000000001421 ) ) ;
#4136 = LINE ( 'NONE', #27928, #20998 ) ;
#4137 = CARTESIAN_POINT ( 'NONE',  ( 5.196152422706629359, -2.999999999999988898, -47.28867513459483973 ) ) ;
#4138 = CARTESIAN_POINT ( 'NONE',  ( 6.350852961086080661, -9.614813431917819062E-14, -118.8750000000000142 ) ) ;
#4139 = CARTESIAN_POINT ( 'NONE',  ( 104.7401757384972285, 0.4802581235374116519, -1.790660471610974636 ) ) ;
#4140 = EDGE_LOOP ( 'NONE', ( #6308, #4388, #17370, #1595 ) ) ;
#4141 = CARTESIAN_POINT ( 'NONE',  ( 3.464101615137757051, -5.999999999999979572, -118.8363248654052171 ) ) ;
#4142 = CARTESIAN_POINT ( 'NONE',  ( -1.000000000000000888, 0.000000000000000000, -5.000000000000004441 ) ) ;
#4143 = DIRECTION ( 'NONE',  ( -1.000000000000000000, -1.665334536937731113E-16, 1.526556658859586792E-16 ) ) ;
#4144 = CARTESIAN_POINT ( 'NONE',  ( 138.2023502691896510, 0.000000000000000000, -5.000000000000004441 ) ) ;
#4145 = DIRECTION ( 'NONE',  ( 1.000000000000000000, 1.067522139062651411E-16, -0.000000000000000000 ) ) ;
#4146 = EDGE_CURVE ( 'NONE', #16363, #4876, #13840, .T. ) ;
#4147 = ORIENTED_EDGE ( 'NONE', *, *, #4283, .T. ) ;
#4148 = CARTESIAN_POINT ( 'NONE',  ( 107.9372167782375840, -0.7662911109077987781, 1.849990392679532247 ) ) ;
#4149 = DIRECTION ( 'NONE',  ( 1.000000000000000000, -5.551115123125773458E-17, -1.260129944081490338E-35 ) ) ;
#4150 = CARTESIAN_POINT ( 'NONE',  ( 113.2497167782375982, -1.308140751793585022, -1.308140751793640533 ) ) ;
#4151 = CARTESIAN_POINT ( 'NONE',  ( -3.608439182435115633, 6.249999999999965361, -111.9419872981078186 ) ) ;
#4152 = CARTESIAN_POINT ( 'NONE',  ( -3.464101615137757051, -5.999999999999979572, -54.58632486540518158 ) ) ;
#4153 = EDGE_LOOP ( 'NONE', ( #23060, #23566, #28693, #23317 ) ) ;
#4154 = ORIENTED_EDGE ( 'NONE', *, *, #17380, .T. ) ;
#4155 = CARTESIAN_POINT ( 'NONE',  ( 139.8750000000000284, 0.000000000000000000, 6.000000000000005329 ) ) ;
#4156 = VERTEX_POINT ( 'NONE', #17403 ) ;
#4157 = CARTESIAN_POINT ( 'NONE',  ( 2.775557561562891351E-14, 6.250000000000033751, -148.0669872981078470 ) ) ;
#4158 = ORIENTED_EDGE ( 'NONE', *, *, #6293, .F. ) ;
#4159 = CARTESIAN_POINT ( 'NONE',  ( -3.464101615137725076, 5.999999999999979572, -151.0863248654051745 ) ) ;
#4160 = CARTESIAN_POINT ( 'NONE',  ( 21.37500000000011724, -1.414213562373090038, 1.414213562373034527 ) ) ;
#4161 = CARTESIAN_POINT ( 'NONE',  ( 3.464101615137852974, 5.999999999999884537, -120.4136751345947829 ) ) ;
#4162 = CARTESIAN_POINT ( 'NONE',  ( 136.2261751345948539, -3.889087296526011706, -3.889087296526011706 ) ) ;
#4163 = CARTESIAN_POINT ( 'NONE',  ( 3.608439182435180470, -6.249999999999997335, -68.55801270189226670 ) ) ;
#4164 = CARTESIAN_POINT ( 'NONE',  ( 135.5105870461000279, -9.078052452530132044, -8.000000000000007105 ) ) ;
#4165 = CARTESIAN_POINT ( 'NONE',  ( 145.6726497308104058, -5.000000000000004441, 0.000000000000000000 ) ) ;
#4166 = DIRECTION ( 'NONE',  ( -0.000000000000000000, -0.6000000000000000888, -0.8000000000000001554 ) ) ;
#4167 = CARTESIAN_POINT ( 'NONE',  ( 4.325218075994005005E-32, 10.49588505988223375, 3.091235803958481245E-67 ) ) ;
#4168 = CARTESIAN_POINT ( 'NONE',  ( 6.000000000000000888, -1.859271017917181981E-14, -146.1636751345948255 ) ) ;
#4169 = VECTOR ( 'NONE', #11840, 1000.000000000000000 ) ;
#4170 = EDGE_CURVE ( 'NONE', #18931, #137, #25162, .T. ) ;
#4171 = CARTESIAN_POINT ( 'NONE',  ( -4.999999999999886313, -15.00000000000001421, 7.500000000000007105 ) ) ;
#4172 = DIRECTION ( 'NONE',  ( 1.000000000000000000, -0.000000000000000000, -0.000000000000000000 ) ) ;
#4173 =( BOUNDED_CURVE ( )  B_SPLINE_CURVE ( 2, ( #6484, #27811, #18639, #9095, #27960, #11117, #29824, #20935, #6784 ),
 .UNSPECIFIED., .F., .F. ) 
 B_SPLINE_CURVE_WITH_KNOTS ( ( 3, 2, 2, 2, 3 ),
 ( 0.1194444444444444503, 0.1203703703703703637, 0.1222222222222222182, 0.1240740740740740727, 0.1249999999999999861 ),
 .UNSPECIFIED. ) 
 CURVE ( )  GEOMETRIC_REPRESENTATION_ITEM ( )  RATIONAL_B_SPLINE_CURVE ( ( 0.9330127018922194093, 0.9330127018922198534, 1.000000000000000000, 0.8660254037844388186, 1.000000000000000000, 0.8660254037844388186, 1.000000000000000000, 0.9330127018922198534, 0.9330127018922194093 ) ) 
 REPRESENTATION_ITEM ( '' )  );
#4174 = CARTESIAN_POINT ( 'NONE',  ( -4.763139720814407951, -2.750000000000016431, -121.0000000000000000 ) ) ;
#4175 = CYLINDRICAL_SURFACE ( 'NONE', #5805, 6.000000000000000888 ) ;
#4176 = DIRECTION ( 'NONE',  ( -0.000000000000000000, -1.000000000000000000, 0.000000000000000000 ) ) ;
#4177 = DIRECTION ( 'NONE',  ( 1.000000000000000000, -5.551115123125773458E-17, -1.260129944081490338E-35 ) ) ;
#4178 = ORIENTED_EDGE ( 'NONE', *, *, #24090, .F. ) ;
#4179 = APPLICATION_CONTEXT ( 'automotive_design' ) ;
#4180 = CARTESIAN_POINT ( 'NONE',  ( -3.175426480542816066, -5.500000000000057732, -53.37500000000002842 ) ) ;
#4181 = DIRECTION ( 'NONE',  ( -1.000000000000000000, -1.665334536937731113E-16, 1.526556658859586792E-16 ) ) ;
#4182 = EDGE_CURVE ( 'NONE', #3683, #18704, #23414, .T. ) ;
#4183 = CARTESIAN_POINT ( 'NONE',  ( 0.000000000000000000, 0.000000000000000000, 0.000000000000000000 ) ) ;
#4184 =( BOUNDED_CURVE ( )  B_SPLINE_CURVE ( 2, ( #30004, #8978, #1746, #8830, #27841, #25549, #25389, #29697, #4347 ),
 .UNSPECIFIED., .F., .T. ) 
 B_SPLINE_CURVE_WITH_KNOTS ( ( 3, 2, 2, 2, 3 ),
 ( 0.5156250000000000000, 0.5234375000000000000, 0.5312500000000000000, 0.5390625000000000000, 0.5468750000000000000 ),
 .UNSPECIFIED. ) 
 CURVE ( )  GEOMETRIC_REPRESENTATION_ITEM ( )  RATIONAL_B_SPLINE_CURVE ( ( 1.000000000000000000, 0.9238795325112867385, 1.000000000000000000, 0.9238795325112867385, 1.000000000000000000, 0.9238795325112867385, 1.000000000000000000, 0.9238795325112867385, 1.000000000000000000 ) ) 
 REPRESENTATION_ITEM ( '' )  );
#4185 = EDGE_CURVE ( 'NONE', #26400, #27302, #26507, .T. ) ;
#4186 = CARTESIAN_POINT ( 'NONE',  ( 6.000000000000000888, -1.859271017917181981E-14, -171.0863248654052029 ) ) ;
#4187 = ORIENTED_EDGE ( 'NONE', *, *, #24710, .F. ) ;
#4188 = CARTESIAN_POINT ( 'NONE',  ( 119.6872167782376408, 1.849990392679562001, 0.7662911109079489913 ) ) ;
#4189 = CARTESIAN_POINT ( 'NONE',  ( 148.6875000000000284, 4.242640687119269671, 4.242640687119298093 ) ) ;
#4190 = CARTESIAN_POINT ( 'NONE',  ( 13.00000000000003908, 2.000000000000112799, 0.000000000000000000 ) ) ;
#4191 = CARTESIAN_POINT ( 'NONE',  ( 140.2500000000000284, -6.000000000000005329, 0.000000000000000000 ) ) ;
#4192 = CARTESIAN_POINT ( 'NONE',  ( 119.8749999999998863, 1.767766952966320915, -1.767766952966320915 ) ) ;
#4193 = ORIENTED_EDGE ( 'NONE', *, *, #18370, .T. ) ;
#4194 = CARTESIAN_POINT ( 'NONE',  ( -3.175426480542816510, -5.500000000000057732, -137.3750000000000568 ) ) ;
#4195 = CARTESIAN_POINT ( 'NONE',  ( 12.68750000000013678, -0.8284271247459952248, -1.999999999999911626 ) ) ;
#4196 = VERTEX_POINT ( 'NONE', #29139 ) ;
#4197 = CARTESIAN_POINT ( 'NONE',  ( 3.175426480543072749, -5.500000000000105693, -75.62500000000000000 ) ) ;
#4198 = ORIENTED_EDGE ( 'NONE', *, *, #12094, .T. ) ;
#4199 = CIRCLE ( 'NONE', #11606, 9.999999999999980460 ) ;
#4200 = CARTESIAN_POINT ( 'NONE',  ( -3.031145847945085681, -10.57562584360016800, -30.18173774084352345 ) ) ;
#4201 = CIRCLE ( 'NONE', #25284, 1.000000000000000000 ) ;
#4202 = ADVANCED_FACE ( 'NONE', ( #26828 ), #12173, .T. ) ;
#4203 = CARTESIAN_POINT ( 'NONE',  ( -5.999999999999963585, -1.487416814333745711E-14, -106.4136751345948113 ) ) ;
#4204 = CARTESIAN_POINT ( 'NONE',  ( 140.5384615384615756, -11.07692307692308908, -4.615384615384614975 ) ) ;
#4205 = DIRECTION ( 'NONE',  ( 0.000000000000000000, -1.000000000000000000, 0.000000000000000000 ) ) ;
#4206 = PRODUCT_CONTEXT ( 'NONE', #24772, 'mechanical' ) ;
#4207 = CARTESIAN_POINT ( 'NONE',  ( 6.350852961086080661, -9.614813431917819062E-14, -151.8749999999999716 ) ) ;
#4208 = CARTESIAN_POINT ( 'NONE',  ( -6.000000000000000888, 1.067854986875958443E-15, 7.560779664488942560E-35 ) ) ;
#4209 = CARTESIAN_POINT ( 'NONE',  ( -3.608439182435115633, 6.249999999999965361, -157.8080127018922383 ) ) ;
#4210 = CARTESIAN_POINT ( 'NONE',  ( -9.999999999999793943, 9.000000000000007105, 4.000000000000003553 ) ) ;
#4211 = MECHANICAL_DESIGN_GEOMETRIC_PRESENTATION_REPRESENTATION (  '', ( #8718 ), #25292 ) ;
#4212 = CARTESIAN_POINT ( 'NONE',  ( -3.175426480542816066, 5.499999999999865885, -83.87500000000004263 ) ) ;
#4213 = ADVANCED_FACE ( 'NONE', ( #4678 ), #14110, .T. ) ;
#4214 = CARTESIAN_POINT ( 'NONE',  ( 0.000000000000000000, 5.499999999999991118, -76.50000000000001421 ) ) ;
#4215 = ADVANCED_FACE ( 'NONE', ( #223 ), #19133, .T. ) ;
#4216 = CARTESIAN_POINT ( 'NONE',  ( 148.2336002691896510, -4.999999999999989342, 2.071067811865468400 ) ) ;
#4217 = DIRECTION ( 'NONE',  ( 1.000000000000000000, 0.000000000000000000, 0.000000000000000000 ) ) ;
#4218 = DIRECTION ( 'NONE',  ( 1.000000000000000000, 1.067522139062651411E-16, -0.000000000000000000 ) ) ;
#4219 = DIRECTION ( 'NONE',  ( 0.000000000000000000, 0.000000000000000000, 1.000000000000000000 ) ) ;
#4220 =( NAMED_UNIT ( * ) PLANE_ANGLE_UNIT ( ) SI_UNIT ( $, .RADIAN. ) );
#4221 = CARTESIAN_POINT ( 'NONE',  ( 18.31249999999999289, -0.8284271247460552878, 2.000000000000031530 ) ) ;
#4222 = CARTESIAN_POINT ( 'NONE',  ( 6.000000000000000888, 1.743066579297358182E-13, -55.58632486540519579 ) ) ;
#4223 = CARTESIAN_POINT ( 'NONE',  ( 117.9372167782374419, -0.7662911109077987781, 1.849990392679591977 ) ) ;
#4224 = CARTESIAN_POINT ( 'NONE',  ( -5.999999999999963585, 9.296355089585909904E-15, -169.4136751345948539 ) ) ;
#4225 = VERTEX_POINT ( 'NONE', #21436 ) ;
#4226 = CARTESIAN_POINT ( 'NONE',  ( 153.6562500000000568, -6.000000000000005329, 2.485281374238555774 ) ) ;
#4227 = CARTESIAN_POINT ( 'NONE',  ( -5.999999999999963585, 1.780251999655701777E-13, -109.4136751345948113 ) ) ;
#4228 = CARTESIAN_POINT ( 'NONE',  ( 118.7502832217622455, -1.308140751793529510, 1.308140751793640533 ) ) ;
#4229 = DIRECTION ( 'NONE',  ( -7.147005652999508048E-36, 5.642372883946980038E-36, 1.000000000000000000 ) ) ;
#4230 = ORIENTED_EDGE ( 'NONE', *, *, #10693, .F. ) ;
#4231 = ORIENTED_EDGE ( 'NONE', *, *, #22296, .T. ) ;
#4232 = ORIENTED_EDGE ( 'NONE', *, *, #20711, .F. ) ;
#4233 = CARTESIAN_POINT ( 'NONE',  ( -3.175426480542816510, -5.500000000000057732, -98.37500000000000000 ) ) ;
#4234 = CARTESIAN_POINT ( 'NONE',  ( 2.775557561562891351E-14, -6.250000000000061284, -106.1830127018922383 ) ) ;
#4235 = ORIENTED_EDGE ( 'NONE', *, *, #5864, .T. ) ;
#4236 = CARTESIAN_POINT ( 'NONE',  ( 159.0000000000000284, -12.00000000000001066, 5.000000000000004441 ) ) ;
#4237 = CARTESIAN_POINT ( 'NONE',  ( 140.0000000000000284, -54.99999999999990763, 7.500000000000007105 ) ) ;
#4238 = EDGE_CURVE ( 'NONE', #20811, #6421, #8176, .T. ) ;
#4239 = CARTESIAN_POINT ( 'NONE',  ( 6.000000000000000888, -1.607695154586752384, -105.7306624327026299 ) ) ;
#4240 = EDGE_LOOP ( 'NONE', ( #16191, #3054, #29890, #30048 ) ) ;
#4241 = CARTESIAN_POINT ( 'NONE',  ( -5.196152422706601826, 2.999999999999975131, -159.9613248654052597 ) ) ;
#4242 = CARTESIAN_POINT ( 'NONE',  ( 1.110223024625164183E-16, -2.000000000000012879, -1.776356839400262692E-15 ) ) ;
#4243 = CARTESIAN_POINT ( 'NONE',  ( 147.5550748654052313, -5.500000000000012434, -2.278174593052012309 ) ) ;
#4244 = CARTESIAN_POINT ( 'NONE',  ( 4.763139720814407951, 2.750000000000002665, -166.7500000000000000 ) ) ;
#4245 = VECTOR ( 'NONE', #9431, 1000.000000000000000 ) ;
#4246 = CARTESIAN_POINT ( 'NONE',  ( 117.6250000000000000, -1.767766952966376426, -1.767766952966320915 ) ) ;
#4247 = CARTESIAN_POINT ( 'NONE',  ( 3.175426480543072749, -5.500000000000105693, -110.1249999999999716 ) ) ;
#4248 = CARTESIAN_POINT ( 'NONE',  ( 21.33632486540526685, -1.767766952966265404, -1.767766952966487448 ) ) ;
#4249 = EDGE_CURVE ( 'NONE', #23925, #25684, #5337, .T. ) ;
#4250 = CARTESIAN_POINT ( 'NONE',  ( -3.175426480542816510, 5.499999999999865885, -98.87499999999998579 ) ) ;
#4251 = CARTESIAN_POINT ( 'NONE',  ( 158.6398502691896510, -3.535533905932752852, 3.535533905932725318 ) ) ;
#4252 = DIRECTION ( 'NONE',  ( -1.000000000000000000, -1.665334536937731113E-16, 1.526556658859586792E-16 ) ) ;
#4253 = CARTESIAN_POINT ( 'NONE',  ( 0.7528846038989732703, -15.55265717403477232, 8.022794483535989229 ) ) ;
#4254 = AXIS2_PLACEMENT_3D ( 'NONE', #6078, #10876, #1001 ) ;
#4255 = ORIENTED_EDGE ( 'NONE', *, *, #16710, .F. ) ;
#4256 = CARTESIAN_POINT ( 'NONE',  ( 12.50000000000009415, 1.873492889145011997, -1.873492889144900975 ) ) ;
#4257 = CARTESIAN_POINT ( 'NONE',  ( 118.4999999999998437, -2.499999999999919176, 0.000000000000000000 ) ) ;
#4258 = CARTESIAN_POINT ( 'NONE',  ( 12.64882486540515671, 2.500000000000084821, -1.035533905932929599 ) ) ;
#4259 = CARTESIAN_POINT ( 'NONE',  ( 111.5627832217621744, 0.7662911109078588412, 1.849990392679712103 ) ) ;
#4260 = CARTESIAN_POINT ( 'NONE',  ( 158.0699251345948255, 2.278174593052198382, 5.499999999999826805 ) ) ;
#4261 = ORIENTED_EDGE ( 'NONE', *, *, #20032, .T. ) ;
#4262 = SURFACE_SIDE_STYLE ('',( #6569 ) ) ;
#4263 = CARTESIAN_POINT ( 'NONE',  ( 107.9372167782375840, -0.7662911109077987781, 1.849990392679532247 ) ) ;
#4264 = CARTESIAN_POINT ( 'NONE',  ( -7.216878364870328078, 0.000000000000000000, -86.19198729810781856 ) ) ;
#4265 = EDGE_LOOP ( 'NONE', ( #2573, #14572, #29950, #29119 ) ) ;
#4266 = VECTOR ( 'NONE', #4794, 1000.000000000000000 ) ;
#4267 = CARTESIAN_POINT ( 'NONE',  ( 159.0863248654052597, 0.000000000000000000, 5.500000000000005329 ) ) ;
#4268 =( BOUNDED_CURVE ( )  B_SPLINE_CURVE ( 2, ( #28977, #24382, #28669, #23949, #14597, #7644, #19196, #28525, #17053 ),
 .UNSPECIFIED., .F., .T. ) 
 B_SPLINE_CURVE_WITH_KNOTS ( ( 3, 2, 2, 2, 3 ),
 ( 0.09166666666666666019, 0.09259259259259258745, 0.09444444444444444198, 0.09629629629629629650, 0.09722222222222222376 ),
 .UNSPECIFIED. ) 
 CURVE ( )  GEOMETRIC_REPRESENTATION_ITEM ( )  RATIONAL_B_SPLINE_CURVE ( ( 0.9330127018922194093, 0.9330127018922189652, 1.000000000000000000, 0.8660254037844388186, 1.000000000000000000, 0.8660254037844388186, 1.000000000000000000, 0.9330127018922194093, 0.9330127018922194093 ) ) 
 REPRESENTATION_ITEM ( '' )  );
#4269 = ORIENTED_EDGE ( 'NONE', *, *, #11894, .F. ) ;
#4270 = VERTEX_POINT ( 'NONE', #18998 ) ;
#4271 = CARTESIAN_POINT ( 'NONE',  ( 149.7187500000000568, 2.485281374238555774, -6.000000000000005329 ) ) ;
#4272 = ORIENTED_EDGE ( 'NONE', *, *, #10270, .F. ) ;
#4273 = CARTESIAN_POINT ( 'NONE',  ( -3.175426480542816510, -5.500000000000057732, -122.3749999999999716 ) ) ;
#4274 = CARTESIAN_POINT ( 'NONE',  ( 21.68750000000009592, -1.097466725451439196, 2.649519052838298805 ) ) ;
#4275 = CARTESIAN_POINT ( 'NONE',  ( 7.216878364870455975, -6.409875621278545621E-14, -129.8080127018922383 ) ) ;
#4276 = ORIENTED_EDGE ( 'NONE', *, *, #3068, .F. ) ;
#4277 = CARTESIAN_POINT ( 'NONE',  ( -5.999999999999963585, 1.780251999655701777E-13, -57.83632486540521711 ) ) ;
#4278 = CARTESIAN_POINT ( 'NONE',  ( -5.412658773652684552, -3.125000000000099920, -171.5669872981078186 ) ) ;
#4279 = CARTESIAN_POINT ( 'NONE',  ( 2.775557561562891351E-14, -6.250000000000061284, -174.3169872981078470 ) ) ;
#4280 = AXIS2_PLACEMENT_3D ( 'NONE', #12252, #2974, #23885 ) ;
#4281 = PRESENTATION_STYLE_ASSIGNMENT (( #9054 ) ) ;
#4282 = LINE ( 'NONE', #20419, #12813 ) ;
#4283 = EDGE_CURVE ( 'NONE', #28542, #27987, #9608, .T. ) ;
#4284 = CARTESIAN_POINT ( 'NONE',  ( 13.31250000000012612, -0.8284271247460552878, 1.999999999999911626 ) ) ;
#4285 = LINE ( 'NONE', #9205, #22081 ) ;
#4286 = EDGE_CURVE ( 'NONE', #11502, #13173, #26170, .T. ) ;
#4287 = CARTESIAN_POINT ( 'NONE',  ( -5.999999999999963585, 1.780251999655701777E-13, -95.33632486540520290 ) ) ;
#4288 = CARTESIAN_POINT ( 'NONE',  ( 3.464101615137852974, 5.999999999999884537, -133.3363248654052313 ) ) ;
#4289 = DIRECTION ( 'NONE',  ( -1.000000000000000000, 0.000000000000000000, 0.000000000000000000 ) ) ;
#4290 = CARTESIAN_POINT ( 'NONE',  ( 110.5627832217621318, 0.7662911109079189043, 1.849990392679652151 ) ) ;
#4291 = CARTESIAN_POINT ( 'NONE',  ( -3.608439182435115633, 6.249999999999965361, -75.94198729810784698 ) ) ;
#4292 = CARTESIAN_POINT ( 'NONE',  ( 5.412658773652739619, 3.124999999999988898, -58.31698729810786119 ) ) ;
#4293 = CARTESIAN_POINT ( 'NONE',  ( 0.000000000000000000, 5.499999999999991118, -52.49999999999999289 ) ) ;
#4294 = CARTESIAN_POINT ( 'NONE',  ( -0.4963810631259262252, -9.251809468437068418, -4.126213593628771825 ) ) ;
#4295 = CARTESIAN_POINT ( 'NONE',  ( -5.999999999999963585, 1.780251999655701777E-13, -47.91367513459483973 ) ) ;
#4296 = AXIS2_PLACEMENT_3D ( 'NONE', #3300, #29098, #8058 ) ;
#4297 = CARTESIAN_POINT ( 'NONE',  ( -5.999999999999963585, 1.780251999655701777E-13, -63.83632486540523132 ) ) ;
#4298 = CARTESIAN_POINT ( 'NONE',  ( 6.350852961086080661, -9.614813431917819062E-14, -120.3750000000000142 ) ) ;
#4299 = CARTESIAN_POINT ( 'NONE',  ( -2.775557561562891351E-14, -5.500000000000115463, -156.7500000000000568 ) ) ;
#4300 = CARTESIAN_POINT ( 'NONE',  ( -3.464101615137725076, 5.999999999999979572, -138.1636751345948824 ) ) ;
#4301 = CARTESIAN_POINT ( 'NONE',  ( 136.4136751345948539, 0.000000000000000000, -5.500000000000005329 ) ) ;
#4302 = EDGE_LOOP ( 'NONE', ( #26549, #17154, #853, #5721 ) ) ;
#4303 = DIRECTION ( 'NONE',  ( 1.000000000000000000, 0.000000000000000000, 0.000000000000000000 ) ) ;
#4304 = DIRECTION ( 'NONE',  ( 1.000000000000000000, -5.551115123125773458E-17, -1.260129944081490338E-35 ) ) ;
#4305 = CARTESIAN_POINT ( 'NONE',  ( 136.6086002691896510, -2.071067811865468400, -4.999999999999989342 ) ) ;
#4306 = EDGE_LOOP ( 'NONE', ( #23629, #17186, #10557, #7384 ) ) ;
#4307 = CARTESIAN_POINT ( 'NONE',  ( 108.8122167782374703, 0.7662911109077987781, 1.849990392679712103 ) ) ;
#4308 = CARTESIAN_POINT ( 'NONE',  ( 151.2113248654052313, 5.500000000000005329, 0.000000000000000000 ) ) ;
#4309 = CARTESIAN_POINT ( 'NONE',  ( 113.9372167782373566, -0.7662911109077388261, 1.849990392679652151 ) ) ;
#4310 = CARTESIAN_POINT ( 'NONE',  ( -7.216878364870328078, 0.000000000000000000, -111.6919872981078186 ) ) ;
#4311 = CARTESIAN_POINT ( 'NONE',  ( 17.27382486540533080, -2.499999999999844569, -1.035533905932809473 ) ) ;
#4312 = CARTESIAN_POINT ( 'NONE',  ( 104.7401757384975411, 1.651227484510909616, 0.8637895383429113894 ) ) ;
#4313 = AXIS2_PLACEMENT_3D ( 'NONE', #9104, #16914, #4177 ) ;
#4314 = ORIENTED_EDGE ( 'NONE', *, *, #6293, .T. ) ;
#4315 = CARTESIAN_POINT ( 'NONE',  ( 21.64882486540524553, 2.500000000000084821, -1.035533905932929599 ) ) ;
#4316 = CARTESIAN_POINT ( 'NONE',  ( 142.1250000000000284, 0.000000000000000000, -6.000000000000005329 ) ) ;
#4317 = CARTESIAN_POINT ( 'NONE',  ( 5.412658773652739619, 3.124999999999988898, -50.81698729810779724 ) ) ;
#4318 = COLOUR_RGB ( '', 0.66274510, 0.83137255, 0.94901961) ;
#4319 = ORIENTED_EDGE ( 'NONE', *, *, #3289, .F. ) ;
#4320 = CARTESIAN_POINT ( 'NONE',  ( -5.412658773652684552, -3.125000000000099920, -149.0669872981078470 ) ) ;
#4321 = PRESENTATION_STYLE_ASSIGNMENT (( #30123 ) ) ;
#4322 = CARTESIAN_POINT ( 'NONE',  ( 23.75000000000013145, 1.665334536937734811E-13, -2.000000000000057288 ) ) ;
#4323 = CARTESIAN_POINT ( 'NONE',  ( 7.216878364870455975, -6.409875621278545621E-14, -65.30801270189225249 ) ) ;
#4324 = ADVANCED_FACE ( 'NONE', ( #11797 ), #2531, .F. ) ;
#4325 = CARTESIAN_POINT ( 'NONE',  ( 143.7038997308103774, 2.071067811865468400, 4.999999999999989342 ) ) ;
#4326 = CARTESIAN_POINT ( 'NONE',  ( -5.196152422706573404, -3.000000000000002665, -125.2113248654052029 ) ) ;
#4327 = CARTESIAN_POINT ( 'NONE',  ( -3.464101615137757051, -5.999999999999979572, -70.16367513459481131 ) ) ;
#4328 = CARTESIAN_POINT ( 'NONE',  ( 0.000000000000000000, -5.999999999999991118, -155.5386751345948539 ) ) ;
#4329 = DIRECTION ( 'NONE',  ( 0.000000000000000000, 1.000000000000000000, 0.000000000000000000 ) ) ;
#4330 = CARTESIAN_POINT ( 'NONE',  ( 110.3124999999999005, -1.035533905932659149, 2.500000000000144773 ) ) ;
#4331 = CARTESIAN_POINT ( 'NONE',  ( -6.000000000000007105, -1.607695154586655129, -95.26933756729739855 ) ) ;
#4332 = CARTESIAN_POINT ( 'NONE',  ( 4.763139720814407951, -2.749999999999988454, -120.5000000000000568 ) ) ;
#4333 = LINE ( 'NONE', #25062, #16235 ) ;
#4334 = EDGE_LOOP ( 'NONE', ( #21111, #21534, #22640, #12031, #23846 ) ) ;
#4335 = CARTESIAN_POINT ( 'NONE',  ( 3.175426480543072749, -5.500000000000105693, -53.12500000000002842 ) ) ;
#4336 = CARTESIAN_POINT ( 'NONE',  ( -3.464101615137725076, 5.999999999999979572, -70.08632486540525974 ) ) ;
#4337 = VERTEX_POINT ( 'NONE', #25731 ) ;
#4338 = CARTESIAN_POINT ( 'NONE',  ( 141.7500000000000568, -6.000000000000005329, 0.000000000000000000 ) ) ;
#4339 = CARTESIAN_POINT ( 'NONE',  ( 140.0000000000000284, -8.500000000000007105, 5.000000000000004441 ) ) ;
#4340 = CARTESIAN_POINT ( 'NONE',  ( 139.1250000000000284, 0.000000000000000000, -6.000000000000005329 ) ) ;
#4341 = EDGE_CURVE ( 'NONE', #29376, #12844, #30183, .T. ) ;
#4342 = CARTESIAN_POINT ( 'NONE',  ( -3.175426480542816510, 5.499999999999865885, -140.8750000000000568 ) ) ;
#4343 = EDGE_LOOP ( 'NONE', ( #26254, #10604, #6763 ) ) ;
#4344 = CARTESIAN_POINT ( 'NONE',  ( 13.12500000000016342, 1.414213562373145550, 1.414213562373034527 ) ) ;
#4345 = ORIENTED_EDGE ( 'NONE', *, *, #19325, .T. ) ;
#4346 = CARTESIAN_POINT ( 'NONE',  ( -3.175426480542816510, -5.500000000000057732, -62.37500000000001421 ) ) ;
#4347 = CARTESIAN_POINT ( 'NONE',  ( 18.53867513459497829, 1.665334536937734811E-13, 2.499999999999946709 ) ) ;
#4348 =( BOUNDED_CURVE ( )  B_SPLINE_CURVE ( 2, ( #12914, #6110, #5786, #22710, #20259, #8094, #29605, #22103, #24986 ),
 .UNSPECIFIED., .F., .T. ) 
 B_SPLINE_CURVE_WITH_KNOTS ( ( 3, 2, 2, 2, 3 ),
 ( 0.5305555555555555580, 0.5314814814814814437, 0.5333333333333333259, 0.5351851851851852082, 0.5361111111111110938 ),
 .UNSPECIFIED. ) 
 CURVE ( )  GEOMETRIC_REPRESENTATION_ITEM ( )  RATIONAL_B_SPLINE_CURVE ( ( 0.9330127018922194093, 0.9330127018922194093, 1.000000000000000000, 0.8660254037844388186, 1.000000000000000000, 0.8660254037844388186, 1.000000000000000000, 0.9330127018922194093, 0.9330127018922194093 ) ) 
 REPRESENTATION_ITEM ( '' )  );
#4349 = CARTESIAN_POINT ( 'NONE',  ( -7.216878364870328078, 0.000000000000000000, -90.05801270189223828 ) ) ;
#4350 = EDGE_CURVE ( 'NONE', #19051, #14937, #21283, .T. ) ;
#4351 = CARTESIAN_POINT ( 'NONE',  ( 10.18750000000014033, 0.8284271247463557142, 2.000000000000031530 ) ) ;
#4352 =( GEOMETRIC_REPRESENTATION_CONTEXT ( 3 ) GLOBAL_UNCERTAINTY_ASSIGNED_CONTEXT ( ( #15325 ) ) GLOBAL_UNIT_ASSIGNED_CONTEXT ( ( #20636, #6791, #22206 ) ) REPRESENTATION_CONTEXT ( 'NONE', 'WORKASPACE' ) );
#4353 = CARTESIAN_POINT ( 'NONE',  ( 112.7113248654049897, 2.000000000000057288, 0.000000000000000000 ) ) ;
#4354 = CARTESIAN_POINT ( 'NONE',  ( 5.999999999999999112, 2.951592740943527306E-14, -150.6636751345948539 ) ) ;
#4355 = CARTESIAN_POINT ( 'NONE',  ( 119.5627832217620750, 0.7662911109078588412, 1.849990392679712103 ) ) ;
#4356 = CARTESIAN_POINT ( 'NONE',  ( 175.7502279533883325, 118.0927510566918670, 256.7417555831058849 ) ) ;
#4357 =( BOUNDED_CURVE ( )  B_SPLINE_CURVE ( 2, ( #8143, #21848, #17408, #10179, #5685, #3084, #10329, #28727, #28581 ),
 .UNSPECIFIED., .F., .T. ) 
 B_SPLINE_CURVE_WITH_KNOTS ( ( 3, 2, 2, 2, 3 ),
 ( 0.2361111111111110494, 0.2370370370370370461, 0.2388888888888889284, 0.2407407407407406996, 0.2416666666666666963 ),
 .UNSPECIFIED. ) 
 CURVE ( )  GEOMETRIC_REPRESENTATION_ITEM ( )  RATIONAL_B_SPLINE_CURVE ( ( 0.9330127018922194093, 0.9330127018922154125, 1.000000000000000000, 0.8660254037844388186, 1.000000000000000000, 0.8660254037844388186, 1.000000000000000000, 0.9330127018922154125, 0.9330127018922194093 ) ) 
 REPRESENTATION_ITEM ( '' )  );
#4358 = CARTESIAN_POINT ( 'NONE',  ( 6.350852961086080661, -9.614813431917819062E-14, -150.3749999999999716 ) ) ;
#4359 = CARTESIAN_POINT ( 'NONE',  ( 19.53867513459495342, 5.551115123125782702E-14, 2.500000000000002220 ) ) ;
#4360 = CARTESIAN_POINT ( 'NONE',  ( 3.175426480543072749, -5.500000000000105693, -141.6250000000000000 ) ) ;
#4361 = CARTESIAN_POINT ( 'NONE',  ( -3.608439182435052128, -6.250000000000110134, -163.3080127018922667 ) ) ;
#4362 = CARTESIAN_POINT ( 'NONE',  ( -0.3854532388872732307, -9.307273380556338793, 4.200333198739636842 ) ) ;
#4363 = CARTESIAN_POINT ( 'NONE',  ( 6.000000000000000888, 1.743066579297358182E-13, -49.58632486540520290 ) ) ;
#4364 = CARTESIAN_POINT ( 'NONE',  ( 4.763139720814407951, -2.749999999999988454, -80.00000000000001421 ) ) ;
#4365 = CARTESIAN_POINT ( 'NONE',  ( 116.8988248654051176, 0.8284271247462654530, 2.000000000000212275 ) ) ;
#4366 = CARTESIAN_POINT ( 'NONE',  ( -3.175426480542816510, 5.499999999999865885, -74.87500000000000000 ) ) ;
#4367 = CARTESIAN_POINT ( 'NONE',  ( 0.000000000000000000, 5.999999999999977796, -154.7886751345948255 ) ) ;
#4368 = DIRECTION ( 'NONE',  ( 0.000000000000000000, 0.000000000000000000, 1.000000000000000000 ) ) ;
#4369 = CARTESIAN_POINT ( 'NONE',  ( 157.5937500000000284, 6.000000000000005329, 2.485281374238585972 ) ) ;
#4370 = DIRECTION ( 'NONE',  ( -1.000000000000000000, -1.665334536937736783E-16, -2.220446049250315546E-16 ) ) ;
#4371 = CARTESIAN_POINT ( 'NONE',  ( -5.999999999999963585, -1.487416814333745711E-14, -118.4136751345948255 ) ) ;
#4372 = CIRCLE ( 'NONE', #21563, 15.00000000000000000 ) ;
#4373 = CARTESIAN_POINT ( 'NONE',  ( 117.8747167782375840, 2.775557561562891351E-14, 1.849990392679523588 ) ) ;
#4374 = FILL_AREA_STYLE_COLOUR ( '', #14540 ) ;
#4375 = ORIENTED_EDGE ( 'NONE', *, *, #22507, .F. ) ;
#4376 = CARTESIAN_POINT ( 'NONE',  ( 156.5625000000000284, -4.242640687119298093, 4.242640687119298093 ) ) ;
#4377 = PLANE ( 'NONE',  #7230 ) ;
#4378 = CARTESIAN_POINT ( 'NONE',  ( 115.6877832217621744, -0.7662911109077087390, 1.849990392679712103 ) ) ;
#4379 = ADVANCED_FACE ( 'NONE', ( #368 ), #19509, .F. ) ;
#4380 = FACE_OUTER_BOUND ( 'NONE', #28546, .T. ) ;
#4381 = ORIENTED_EDGE ( 'NONE', *, *, #17113, .F. ) ;
#4382 = ORIENTED_EDGE ( 'NONE', *, *, #27363, .F. ) ;
#4383 = ORIENTED_EDGE ( 'NONE', *, *, #4839, .T. ) ;
#4384 = CARTESIAN_POINT ( 'NONE',  ( -4.763139720814407951, -2.750000000000016431, -91.00000000000002842 ) ) ;
#4385 = EDGE_CURVE ( 'NONE', #15456, #21925, #24186, .T. ) ;
#4386 = CARTESIAN_POINT ( 'NONE',  ( -5.412658773652739619, 3.124999999999975131, -111.1830127018922383 ) ) ;
#4387 = EDGE_CURVE ( 'NONE', #12154, #87, #4547, .T. ) ;
#4388 = ORIENTED_EDGE ( 'NONE', *, *, #26976, .T. ) ;
#4389 = DIRECTION ( 'NONE',  ( 1.000000000000000000, -5.551115123125774074E-17, -1.260129944081490070E-35 ) ) ;
#4390 = CARTESIAN_POINT ( 'NONE',  ( 1.000000000000000888, -14.99923475244191451, 9.015151515151503148 ) ) ;
#4391 = CARTESIAN_POINT ( 'NONE',  ( 4.513192036456002754, -10.03241344175769534, -28.95831720094627926 ) ) ;
#4392 = EDGE_LOOP ( 'NONE', ( #21286, #10171, #17906, #1588 ) ) ;
#4393 = CARTESIAN_POINT ( 'NONE',  ( 0.000000000000000000, 5.999999999999977796, -46.78867513459483973 ) ) ;
#4394 = CARTESIAN_POINT ( 'NONE',  ( -9.999999999999994671, -71.00000000000002842, 5.000000000000004441 ) ) ;
#4395 = CONICAL_SURFACE ( 'NONE', #24975, 2.499999999999999112, 0.7853981633974522758 ) ;
#4396 = CARTESIAN_POINT ( 'NONE',  ( -3.175426480542816066, 5.499999999999865885, -173.8750000000000568 ) ) ;
#4397 = CARTESIAN_POINT ( 'NONE',  ( 147.4613248654052029, -5.500000000000005329, 0.000000000000000000 ) ) ;
#4398 = CARTESIAN_POINT ( 'NONE',  ( 6.350852961086080661, -9.614813431917819062E-14, -163.8750000000000284 ) ) ;
#4399 = CARTESIAN_POINT ( 'NONE',  ( 115.1874999999998437, 1.035533905932719101, 2.500000000000265121 ) ) ;
#4400 = VECTOR ( 'NONE', #3514, 1000.000000000000000 ) ;
#4401 =( BOUNDED_CURVE ( )  B_SPLINE_CURVE ( 2, ( #23507, #11861, #27771, #6748, #21201, #9523, #16168, #25473, #13863 ),
 .UNSPECIFIED., .F., .F. ) 
 B_SPLINE_CURVE_WITH_KNOTS ( ( 3, 2, 2, 2, 3 ),
 ( 0.3305555555555555469, 0.3314814814814814881, 0.3333333333333333148, 0.3351851851851851971, 0.3361111111111110827 ),
 .UNSPECIFIED. ) 
 CURVE ( )  GEOMETRIC_REPRESENTATION_ITEM ( )  RATIONAL_B_SPLINE_CURVE ( ( 0.9330127018922194093, 0.9330127018922194093, 1.000000000000000000, 0.8660254037844388186, 1.000000000000000000, 0.8660254037844388186, 1.000000000000000000, 0.9330127018922214077, 0.9330127018922194093 ) ) 
 REPRESENTATION_ITEM ( '' )  );
#4402 = CARTESIAN_POINT ( 'NONE',  ( 3.175426480543072749, -5.500000000000105693, -102.6250000000000142 ) ) ;
#4403 = CARTESIAN_POINT ( 'NONE',  ( -5.196152422706573404, -3.000000000000002665, -166.2886751345948255 ) ) ;
#4404 = CARTESIAN_POINT ( 'NONE',  ( 6.350852961086080661, -9.614813431917819062E-14, -96.37499999999997158 ) ) ;
#4405 = SURFACE_SIDE_STYLE ('',( #2419 ) ) ;
#4406 = CARTESIAN_POINT ( 'NONE',  ( 0.1659452612680607231, -15.34501306676551202, 8.417236167508884037 ) ) ;
#4407 = ORIENTED_EDGE ( 'NONE', *, *, #30077, .T. ) ;
#4408 = CARTESIAN_POINT ( 'NONE',  ( 11.37500000000007994, 2.220446049250313081E-13, -2.649519052838444910 ) ) ;
#4409 = CARTESIAN_POINT ( 'NONE',  ( 116.8749999999998863, 1.767766952966320915, -1.767766952966320915 ) ) ;
#4410 = CARTESIAN_POINT ( 'NONE',  ( 6.000000000000000888, 1.607695154586715303, -130.5193375672974128 ) ) ;
#4411 = CARTESIAN_POINT ( 'NONE',  ( 107.5627832217621744, 0.7662911109077987781, 1.849990392679772278 ) ) ;
#4412 = LINE ( 'NONE', #11683, #13537 ) ;
#4413 = ORIENTED_EDGE ( 'NONE', *, *, #30050, .F. ) ;
#4414 = CARTESIAN_POINT ( 'NONE',  ( -3.464101615137757051, -5.999999999999979572, -170.0863248654051745 ) ) ;
#4415 = CARTESIAN_POINT ( 'NONE',  ( 105.6247167782375271, 1.849990392679495832, 0.000000000000000000 ) ) ;
#4416 = CARTESIAN_POINT ( 'NONE',  ( 2.775557561562891351E-14, -6.250000000000061284, -85.81698729810783277 ) ) ;
#4417 = EDGE_CURVE ( 'NONE', #283, #29510, #24460, .T. ) ;
#4418 =( GEOMETRIC_REPRESENTATION_CONTEXT ( 3 ) GLOBAL_UNCERTAINTY_ASSIGNED_CONTEXT ( ( #9677 ) ) GLOBAL_UNIT_ASSIGNED_CONTEXT ( ( #14808, #10341, #29047 ) ) REPRESENTATION_CONTEXT ( 'NONE', 'WORKASPACE' ) );
#4419 = CARTESIAN_POINT ( 'NONE',  ( 3.464101615137757051, -5.999999999999979572, -65.41367513459485394 ) ) ;
#4420 = AXIS2_PLACEMENT_3D ( 'NONE', #10080, #6055, #981 ) ;
#4421 = ORIENTED_EDGE ( 'NONE', *, *, #4778, .F. ) ;
#4422 = CARTESIAN_POINT ( 'NONE',  ( 147.8437500000000284, -6.000000000000005329, -2.485281374238555774 ) ) ;
#4423 = VERTEX_POINT ( 'NONE', #961 ) ;
#4424 = CARTESIAN_POINT ( 'NONE',  ( -2.775557561562891351E-14, -5.500000000000115463, -123.7500000000000284 ) ) ;
#4425 = CARTESIAN_POINT ( 'NONE',  ( 21.87500000000008882, -2.649519052838111843, 1.110223024625156540E-13 ) ) ;
#4426 = EDGE_CURVE ( 'NONE', #16190, #6115, #16992, .T. ) ;
#4427 = CARTESIAN_POINT ( 'NONE',  ( 5.412658773652739619, 3.124999999999988898, -129.6830127018922667 ) ) ;
#4428 = ORIENTED_EDGE ( 'NONE', *, *, #3402, .F. ) ;
#4429 = PRESENTATION_STYLE_ASSIGNMENT (( #16156 ) ) ;
#4430 = CARTESIAN_POINT ( 'NONE',  ( 3.608439182435180470, 6.249999999999982236, -170.6919872981078470 ) ) ;
#4431 = CARTESIAN_POINT ( 'NONE',  ( 5.412658773652712085, -3.125000000000086153, -177.0669872981078186 ) ) ;
#4432 = CARTESIAN_POINT ( 'NONE',  ( 160.9999999919967877, -11.61962113023372289, 3.007375573655278966 ) ) ;
#4433 = SURFACE_STYLE_USAGE ( .BOTH. , #5135 ) ;
#4434 = CARTESIAN_POINT ( 'NONE',  ( 12.81250000000004441, 0.8284271247461753029, -2.000000000000091926 ) ) ;
#4435 = CARTESIAN_POINT ( 'NONE',  ( 0.7580070251407292625, -15.51657223718414791, -8.092363357809270852 ) ) ;
#4436 = CIRCLE ( 'NONE', #6246, 0.5000000000000004441 ) ;
#4437 = DIRECTION ( 'NONE',  ( 0.000000000000000000, 0.000000000000000000, 1.000000000000000000 ) ) ;
#4438 = DIRECTION ( 'NONE',  ( 1.000000000000000000, -5.551115123125773458E-17, -1.260129944081490338E-35 ) ) ;
#4439 = CARTESIAN_POINT ( 'NONE',  ( -3.464101615137725076, 5.999999999999979572, -133.0863248654052313 ) ) ;
#4440 = CARTESIAN_POINT ( 'NONE',  ( 3.464101615137757051, -5.999999999999979572, -150.3363248654051176 ) ) ;
#4441 = CARTESIAN_POINT ( 'NONE',  ( 112.2502832217622739, 1.308140751793640533, -1.308140751793640533 ) ) ;
#4442 = CARTESIAN_POINT ( 'NONE',  ( 5.412658773652712085, -3.125000000000086153, -73.56698729810784698 ) ) ;
#4443 = CARTESIAN_POINT ( 'NONE',  ( -5.412658773652684552, -3.125000000000099920, -60.56698729810783277 ) ) ;
#4444 = CARTESIAN_POINT ( 'NONE',  ( -4.763139720814407951, 2.749999999999946709, -49.25000000000001421 ) ) ;
#4445 = CARTESIAN_POINT ( 'NONE',  ( -9.757819552369539906E-16, -10.00000000000000888, -5.000000000000004441 ) ) ;
#4446 = LINE ( 'NONE', #18155, #18692 ) ;
#4447 = CARTESIAN_POINT ( 'NONE',  ( -5.999999999999963585, 1.780251999655701777E-13, -53.91367513459482552 ) ) ;
#4448 = CARTESIAN_POINT ( 'NONE',  ( 3.175426480543072749, -5.500000000000105693, -117.6250000000000284 ) ) ;
#4449 = CARTESIAN_POINT ( 'NONE',  ( 135.2765744903421137, -8.508179439634940167, -8.095374785726331623 ) ) ;
#4450 = DIRECTION ( 'NONE',  ( 0.000000000000000000, 0.000000000000000000, 1.000000000000000000 ) ) ;
#4451 = ORIENTED_EDGE ( 'NONE', *, *, #26909, .T. ) ;
#4452 = CARTESIAN_POINT ( 'NONE',  ( 21.87500000000006040, 1.110223024625156540E-13, 2.649519052838167354 ) ) ;
#4453 = CARTESIAN_POINT ( 'NONE',  ( -5.999999999999963585, 1.780251999655701777E-13, -104.9136751345948255 ) ) ;
#4454 =( BOUNDED_CURVE ( )  B_SPLINE_CURVE ( 2, ( #4869, #9508, #23640, #18894, #16305, #16452, #14300, #28063, #11846 ),
 .UNSPECIFIED., .F., .T. ) 
 B_SPLINE_CURVE_WITH_KNOTS ( ( 3, 2, 2, 2, 3 ),
 ( 0.04722222222222216548, 0.04814814814814816213, 0.05000000000000004441, 0.05185185185185181567, 0.05277777777777781232 ),
 .UNSPECIFIED. ) 
 CURVE ( )  GEOMETRIC_REPRESENTATION_ITEM ( )  RATIONAL_B_SPLINE_CURVE ( ( 0.9330127018922194093, 0.9330127018922154125, 1.000000000000000000, 0.8660254037844388186, 1.000000000000000000, 0.8660254037844388186, 1.000000000000000000, 0.9330127018922154125, 0.9330127018922194093 ) ) 
 REPRESENTATION_ITEM ( '' )  );
#4455 = AXIS2_PLACEMENT_3D ( 'NONE', #4661, #4516, #29855 ) ;
#4456 = ORIENTED_EDGE ( 'NONE', *, *, #1406, .T. ) ;
#4457 = CARTESIAN_POINT ( 'NONE',  ( 109.4997167782374845, 1.308140751793696044, -1.308140751793640533 ) ) ;
#4458 = LINE ( 'NONE', #18775, #2007 ) ;
#4459 = CARTESIAN_POINT ( 'NONE',  ( 112.1872167782374135, -1.849990392679411677, -0.7662911109075883909 ) ) ;
#4460 = CARTESIAN_POINT ( 'NONE',  ( -3.608439182435115633, 6.249999999999965361, -107.4419872981077901 ) ) ;
#4461 = EDGE_CURVE ( 'NONE', #30108, #1220, #18940, .T. ) ;
#4462 = FACE_OUTER_BOUND ( 'NONE', #12535, .T. ) ;
#4463 = EDGE_CURVE ( 'NONE', #17549, #16378, #20073, .T. ) ;
#4464 = CARTESIAN_POINT ( 'NONE',  ( 10.00000000000014744, 0.5735884529305894652, 2.302716324837206230 ) ) ;
#4465 = ORIENTED_EDGE ( 'NONE', *, *, #20957, .F. ) ;
#4466 = ORIENTED_EDGE ( 'NONE', *, *, #6923, .F. ) ;
#4467 = CARTESIAN_POINT ( 'NONE',  ( 6.000000000000000888, -3.330669073875464691E-16, -7.560779664488942560E-35 ) ) ;
#4468 = CARTESIAN_POINT ( 'NONE',  ( 134.8125000000000284, 4.242640687119298093, -4.242640687119298093 ) ) ;
#4469 = AXIS2_PLACEMENT_3D ( 'NONE', #18296, #27610, #6587 ) ;
#4470 = CARTESIAN_POINT ( 'NONE',  ( 3.608439182435180470, 6.249999999999982236, -140.6919872981078470 ) ) ;
#4471 = MECHANICAL_DESIGN_GEOMETRIC_PRESENTATION_REPRESENTATION (  '', ( #29966 ), #21181 ) ;
#4472 = CARTESIAN_POINT ( 'NONE',  ( 14.97617513459490191, -1.035533905932568999, -2.499999999999904521 ) ) ;
#4473 = CARTESIAN_POINT ( 'NONE',  ( 21.50000000000004619, -1.999999999999890754, -1.665334536937734811E-13 ) ) ;
#4474 = CARTESIAN_POINT ( 'NONE',  ( 125.0000000000000568, -55.00000000000000711, 8.000000000000007105 ) ) ;
#4475 = CARTESIAN_POINT ( 'NONE',  ( 3.608439182435180470, 6.249999999999982236, -71.05801270189222407 ) ) ;
#4476 = CARTESIAN_POINT ( 'NONE',  ( 134.9304254777555911, -7.819842479424068848, -8.000000000000007105 ) ) ;
#4477 = CARTESIAN_POINT ( 'NONE',  ( 141.3601497308104058, -3.535533905932725318, -3.535533905932725318 ) ) ;
#4478 = CARTESIAN_POINT ( 'NONE',  ( 0.000000000000000000, 0.000000000000000000, -185.0000000000000000 ) ) ;
#4479 = CARTESIAN_POINT ( 'NONE',  ( 0.000000000000000000, 0.000000000000000000, 0.000000000000000000 ) ) ;
#4480 = CARTESIAN_POINT ( 'NONE',  ( 129.9999999999998010, -90.00000000000001421, -3.000000000000002665 ) ) ;
#4481 = VECTOR ( 'NONE', #29362, 1000.000000000000000 ) ;
#4482 = CARTESIAN_POINT ( 'NONE',  ( 24.67146418439117639, -2.317096007398430579, 0.2759497617555390914 ) ) ;
#4483 =( NAMED_UNIT ( * ) PLANE_ANGLE_UNIT ( ) SI_UNIT ( $, .RADIAN. ) );
#4484 = CARTESIAN_POINT ( 'NONE',  ( 110.2499999999998010, -5.551115123125782702E-14, 2.500000000000168754 ) ) ;
#4485 = CARTESIAN_POINT ( 'NONE',  ( 4.763139720814407951, 2.750000000000002665, -121.7500000000000284 ) ) ;
#4486 = CARTESIAN_POINT ( 'NONE',  ( -5.999999999999963585, -1.487416814333745711E-14, -92.91367513459482552 ) ) ;
#4487 = CARTESIAN_POINT ( 'NONE',  ( -5.412658773652684552, -3.125000000000099920, -145.4330127018922383 ) ) ;
#4488 = CARTESIAN_POINT ( 'NONE',  ( 5.999999999999949374, 1.607695154586804565, -113.0966878364870638 ) ) ;
#4489 = ORIENTED_EDGE ( 'NONE', *, *, #6252, .T. ) ;
#4490 = TOROIDAL_SURFACE ( 'NONE', #3005, 28.99999999999999645, 1.000000000000000000 ) ;
#4491 = CARTESIAN_POINT ( 'NONE',  ( -3.175426480542816066, 5.499999999999865885, -58.37500000000004974 ) ) ;
#4492 = CARTESIAN_POINT ( 'NONE',  ( 3.464101615137852974, 5.999999999999884537, -62.83632486540521711 ) ) ;
#4493 = DIRECTION ( 'NONE',  ( 0.000000000000000000, 0.000000000000000000, 1.000000000000000000 ) ) ;
#4494 = VERTEX_POINT ( 'NONE', #8032 ) ;
#4495 = VECTOR ( 'NONE', #28538, 1000.000000000000000 ) ;
#4496 = CARTESIAN_POINT ( 'NONE',  ( 120.1872167782373992, -1.849990392679441875, -0.7662911109076485650 ) ) ;
#4497 = CARTESIAN_POINT ( 'NONE',  ( 137.9062500000000568, 6.000000000000005329, -2.485281374238556218 ) ) ;
#4498 = CARTESIAN_POINT ( 'NONE',  ( 2.775557561562891351E-14, 6.250000000000033751, -106.0669872981078186 ) ) ;
#4499 = CARTESIAN_POINT ( 'NONE',  ( -15.49999999999999289, -25.00000000000007816, -8.000000000000007105 ) ) ;
#4500 = EDGE_CURVE ( 'NONE', #22104, #21789, #2226, .T. ) ;
#4501 = CARTESIAN_POINT ( 'NONE',  ( 132.1875000000000284, 4.242640687119269671, 4.242640687119298093 ) ) ;
#4502 = DIRECTION ( 'NONE',  ( 1.000000000000000000, -5.551115123125773458E-17, -1.260129944081490338E-35 ) ) ;
#4503 = CIRCLE ( 'NONE', #11409, 17.50000000000000355 ) ;
#4504 = VECTOR ( 'NONE', #16769, 1000.000000000000000 ) ;
#4505 = CARTESIAN_POINT ( 'NONE',  ( -2.775557561562891351E-14, -5.500000000000115463, -138.7500000000000284 ) ) ;
#4506 = ORIENTED_EDGE ( 'NONE', *, *, #2655, .F. ) ;
#4507 = VECTOR ( 'NONE', #18687, 1000.000000000000000 ) ;
#4508 = CARTESIAN_POINT ( 'NONE',  ( 11.62499999999999645, -1.414213562373090038, -1.414213562373090038 ) ) ;
#4509 = EDGE_LOOP ( 'NONE', ( #560, #29654, #25424, #12185 ) ) ;
#4510 = CARTESIAN_POINT ( 'NONE',  ( 3.175426480543072749, -5.500000000000105693, -62.12500000000000711 ) ) ;
#4511 = CARTESIAN_POINT ( 'NONE',  ( 10.00000000000015099, 1.032209696753886519, -2.067976829748041645 ) ) ;
#4512 = CARTESIAN_POINT ( 'NONE',  ( 119.9800011666190755, -0.2475512722491883533, 2.000000000000047073 ) ) ;
#4513 = AXIS2_PLACEMENT_3D ( 'NONE', #26595, #15591, #29195 ) ;
#4514 = CARTESIAN_POINT ( 'NONE',  ( 104.8122167782375129, 0.7662911109077388261, 1.849990392679712103 ) ) ;
#4515 = CARTESIAN_POINT ( 'NONE',  ( -19.49999999999998224, -25.00000000000010658, -7.500000000000007105 ) ) ;
#4516 = DIRECTION ( 'NONE',  ( -7.147005652999508048E-36, 5.642372883946980038E-36, 1.000000000000000000 ) ) ;
#4517 = CARTESIAN_POINT ( 'NONE',  ( 120.0002832217621886, -1.308140751793557266, -1.308140751793529510 ) ) ;
#4518 = CARTESIAN_POINT ( 'NONE',  ( -2.775557561562891351E-14, -5.500000000000115463, -150.7500000000000568 ) ) ;
#4519 = CARTESIAN_POINT ( 'NONE',  ( 140.0000000000000284, -10.00000000000000888, -7.500000000000007105 ) ) ;
#4520 = CARTESIAN_POINT ( 'NONE',  ( 4.763139720814407951, -2.749999999999988454, -140.0000000000000000 ) ) ;
#4521 = CARTESIAN_POINT ( 'NONE',  ( -5.412658773652684552, -3.125000000000099920, -157.4330127018922383 ) ) ;
#4522 = LINE ( 'NONE', #26158, #23454 ) ;
#4523 = EDGE_CURVE ( 'NONE', #407, #10456, #7680, .T. ) ;
#4524 = CARTESIAN_POINT ( 'NONE',  ( 3.175426480543072749, -5.500000000000105693, -75.62500000000001421 ) ) ;
#4525 = CARTESIAN_POINT ( 'NONE',  ( -5.999999999999963585, 1.780251999655701777E-13, -69.83632486540523132 ) ) ;
#4526 = CARTESIAN_POINT ( 'NONE',  ( -3.175426480542816510, -5.500000000000057732, -75.87500000000001421 ) ) ;
#4527 = CARTESIAN_POINT ( 'NONE',  ( 148.0461002691896510, -2.071067811865468400, 4.999999999999989342 ) ) ;
#4528 = LINE ( 'NONE', #11792, #18165 ) ;
#4529 = CARTESIAN_POINT ( 'NONE',  ( 1.000000000000000888, 0.000000000000000000, 0.000000000000000000 ) ) ;
#4530 = CARTESIAN_POINT ( 'NONE',  ( 160.9687500000000568, -2.485281374238585972, 6.000000000000005329 ) ) ;
#4531 = CARTESIAN_POINT ( 'NONE',  ( 5.196152422706629359, 3.000000000000002665, -134.0386751345948255 ) ) ;
#4532 = CARTESIAN_POINT ( 'NONE',  ( 20.43750000000014566, -1.999999999999911626, 0.8284271247462354770 ) ) ;
#4533 = CARTESIAN_POINT ( 'NONE',  ( -6.000000000000000888, 1.067854986875958443E-15, 7.560779664488942560E-35 ) ) ;
#4534 = DIRECTION ( 'NONE',  ( 0.000000000000000000, 0.000000000000000000, 1.000000000000000000 ) ) ;
#4535 = ADVANCED_FACE ( 'NONE', ( #28763 ), #7731, .T. ) ;
#4536 = ORIENTED_EDGE ( 'NONE', *, *, #17911, .F. ) ;
#4537 = CARTESIAN_POINT ( 'NONE',  ( 156.2812500000000284, 2.485281374238585972, 6.000000000000005329 ) ) ;
#4538 = CARTESIAN_POINT ( 'NONE',  ( 0.000000000000000000, -5.999999999999991118, -109.0386751345948113 ) ) ;
#4539 = CARTESIAN_POINT ( 'NONE',  ( 116.0627832217622029, -0.7662911109076785410, -1.849990392679291551 ) ) ;
#4540 = CARTESIAN_POINT ( 'NONE',  ( -5.196152422706601826, 2.999999999999975131, -179.4613248654052313 ) ) ;
#4541 = ORIENTED_EDGE ( 'NONE', *, *, #3918, .T. ) ;
#4542 = ORIENTED_EDGE ( 'NONE', *, *, #14882, .T. ) ;
#4543 =( BOUNDED_CURVE ( )  B_SPLINE_CURVE ( 2, ( #28951, #14860, #16886, #28800, #21322, #17027, #14571, #12282, #12135 ),
 .UNSPECIFIED., .F., .T. ) 
 B_SPLINE_CURVE_WITH_KNOTS ( ( 3, 2, 2, 2, 3 ),
 ( 0.6406250000000000000, 0.6484375000000000000, 0.6562500000000000000, 0.6640625000000000000, 0.6718750000000000000 ),
 .UNSPECIFIED. ) 
 CURVE ( )  GEOMETRIC_REPRESENTATION_ITEM ( )  RATIONAL_B_SPLINE_CURVE ( ( 1.000000000000000000, 0.9238795325112867385, 1.000000000000000000, 0.9238795325112867385, 1.000000000000000000, 0.9238795325112867385, 1.000000000000000000, 0.9238795325112867385, 1.000000000000000000 ) ) 
 REPRESENTATION_ITEM ( '' )  );
#4544 = ORIENTED_EDGE ( 'NONE', *, *, #533, .F. ) ;
#4545 = CARTESIAN_POINT ( 'NONE',  ( -3.175426480542816510, -5.500000000000057732, -86.37500000000005684 ) ) ;
#4546 = CARTESIAN_POINT ( 'NONE',  ( 5.412658773652739619, 3.124999999999988898, -105.6830127018922383 ) ) ;
#4547 =( BOUNDED_CURVE ( )  B_SPLINE_CURVE ( 2, ( #25579, #20992, #30339, #6989, #21737, #14680, #26907, #1114, #3413 ),
 .UNSPECIFIED., .F., .T. ) 
 B_SPLINE_CURVE_WITH_KNOTS ( ( 3, 2, 2, 2, 3 ),
 ( 0.6138888888888888173, 0.6148148148148148140, 0.6166666666666666963, 0.6185185185185184675, 0.6194444444444444642 ),
 .UNSPECIFIED. ) 
 CURVE ( )  GEOMETRIC_REPRESENTATION_ITEM ( )  RATIONAL_B_SPLINE_CURVE ( ( 0.9330127018922194093, 0.9330127018922154125, 1.000000000000000000, 0.8660254037844388186, 1.000000000000000000, 0.8660254037844388186, 1.000000000000000000, 0.9330127018922154125, 0.9330127018922194093 ) ) 
 REPRESENTATION_ITEM ( '' )  );
#4548 = ORIENTED_EDGE ( 'NONE', *, *, #5303, .F. ) ;
#4549 = DIRECTION ( 'NONE',  ( 0.000000000000000000, 0.000000000000000000, -1.000000000000000000 ) ) ;
#4550 = DIRECTION ( 'NONE',  ( 0.000000000000000000, 1.000000000000000000, 0.000000000000000000 ) ) ;
#4551 = CARTESIAN_POINT ( 'NONE',  ( 6.350852961086080661, -9.614813431917819062E-14, -163.8750000000000284 ) ) ;
#4552 = CARTESIAN_POINT ( 'NONE',  ( 4.384309399116693484, -10.08956758734763071, -29.10056064752990679 ) ) ;
#4553 = ORIENTED_EDGE ( 'NONE', *, *, #11147, .T. ) ;
#4554 = CARTESIAN_POINT ( 'NONE',  ( 3.464101615137757051, -5.999999999999979572, -67.83632486540517448 ) ) ;
#4555 = STYLED_ITEM ( 'NONE', ( #4829 ), #22508 ) ;
#4556 = CARTESIAN_POINT ( 'NONE',  ( 3.175426480543072749, 5.499999999999865885, -169.6250000000000000 ) ) ;
#4557 = LINE ( 'NONE', #11196, #20392 ) ;
#4558 = CARTESIAN_POINT ( 'NONE',  ( -3.175426480542816510, -5.500000000000057732, -165.8750000000000568 ) ) ;
#4559 = CARTESIAN_POINT ( 'NONE',  ( 112.1874999999998295, 1.035533905932719101, 2.500000000000205169 ) ) ;
#4560 = ADVANCED_FACE ( 'NONE', ( #12541 ), #3119, .F. ) ;
#4561 = CARTESIAN_POINT ( 'NONE',  ( 3.175426480543072749, -5.500000000000105693, -99.62500000000007105 ) ) ;
#4562 = DIRECTION ( 'NONE',  ( -7.147005652999508048E-36, 5.642372883946980038E-36, 1.000000000000000000 ) ) ;
#4563 = CARTESIAN_POINT ( 'NONE',  ( -6.350852961085760029, -1.281975124255709124E-13, -97.12500000000004263 ) ) ;
#4564 = CARTESIAN_POINT ( 'NONE',  ( 159.2023502691896510, 0.000000000000000000, -5.000000000000004441 ) ) ;
#4565 = CARTESIAN_POINT ( 'NONE',  ( 135.0101475501562049, -7.374327361089822119, 8.398546155689757597 ) ) ;
#4566 = VERTEX_POINT ( 'NONE', #17294 ) ;
#4567 = CARTESIAN_POINT ( 'NONE',  ( 11.87500000000013500, 1.665334536937734811E-13, 2.649519052838278377 ) ) ;
#4568 = CARTESIAN_POINT ( 'NONE',  ( 114.7499999999999147, -5.551115123125782702E-14, -2.499999999999946709 ) ) ;
#4569 = CARTESIAN_POINT ( 'NONE',  ( 12.96132486540529882, 1.110223024625156540E-13, 2.500000000000002220 ) ) ;
#4570 = CARTESIAN_POINT ( 'NONE',  ( 105.1252832217623023, -5.551115123125782702E-14, -1.849990392679523588 ) ) ;
#4571 = ADVANCED_FACE ( 'NONE', ( #6657 ), #20648, .F. ) ;
#4572 = CARTESIAN_POINT ( 'NONE',  ( 23.97617513459492145, -1.035533905932689347, -2.500000000000084821 ) ) ;
#4573 = VERTEX_POINT ( 'NONE', #13606 ) ;
#4574 = FACE_OUTER_BOUND ( 'NONE', #29910, .T. ) ;
#4575 =( NAMED_UNIT ( * ) SI_UNIT ( $, .STERADIAN. ) SOLID_ANGLE_UNIT ( ) );
#4576 = ORIENTED_EDGE ( 'NONE', *, *, #21687, .F. ) ;
#4577 = CARTESIAN_POINT ( 'NONE',  ( 0.000000000000000000, -5.999999999999991118, -141.4613248654052029 ) ) ;
#4578 = CARTESIAN_POINT ( 'NONE',  ( 152.0625000000000568, -4.242640687119298093, 4.242640687119298093 ) ) ;
#4579 = CARTESIAN_POINT ( 'NONE',  ( 0.000000000000000000, 5.499999999999991118, -117.0000000000000000 ) ) ;
#4580 = CARTESIAN_POINT ( 'NONE',  ( 20.87500000000011724, -2.649519052838167354, -5.551115123125782702E-14 ) ) ;
#4581 = ORIENTED_EDGE ( 'NONE', *, *, #11046, .T. ) ;
#4582 = CARTESIAN_POINT ( 'NONE',  ( 7.216878364870455975, -6.409875621278545621E-14, -131.3080127018922667 ) ) ;
#4583 = VERTEX_POINT ( 'NONE', #1890 ) ;
#4584 = CARTESIAN_POINT ( 'NONE',  ( 137.3363248654052029, 0.000000000000000000, -5.500000000000005329 ) ) ;
#4585 = CARTESIAN_POINT ( 'NONE',  ( 7.216878364870455975, -6.409875621278545621E-14, -169.4419872981078470 ) ) ;
#4586 = CARTESIAN_POINT ( 'NONE',  ( 108.9999999999998579, 2.500000000000030198, 1.110223024625156540E-13 ) ) ;
#4587 = CARTESIAN_POINT ( 'NONE',  ( 10.75000000000014921, 1.665334536937734811E-13, -2.000000000000168310 ) ) ;
#4588 = CARTESIAN_POINT ( 'NONE',  ( -0.08172395017747559332, -15.06317155720421930, -7.964553512345503350 ) ) ;
#4589 = CARTESIAN_POINT ( 'NONE',  ( 153.0074251345948255, 2.278174593052074925, -5.499999999999950262 ) ) ;
#4590 = DIRECTION ( 'NONE',  ( 0.000000000000000000, 0.000000000000000000, 1.000000000000000000 ) ) ;
#4591 = CARTESIAN_POINT ( 'NONE',  ( 6.000000000000000888, -1.859271017917181981E-14, -68.16367513459481131 ) ) ;
#4592 = CARTESIAN_POINT ( 'NONE',  ( 109.4377832217621460, 1.849990392679562001, 0.7662911109080692285 ) ) ;
#4593 = CARTESIAN_POINT ( 'NONE',  ( 5.412658773652739619, 3.124999999999988898, -174.6830127018922383 ) ) ;
#4594 = CARTESIAN_POINT ( 'NONE',  ( -0.5000000001309222730, -10.00000000000000888, -4.869076758059778243 ) ) ;
#4595 = EDGE_CURVE ( 'NONE', #24916, #18033, #3184, .T. ) ;
#4596 = CARTESIAN_POINT ( 'NONE',  ( -0.5000000000000004441, -15.50000000000001421, -7.500000000000007105 ) ) ;
#4597 = CARTESIAN_POINT ( 'NONE',  ( -6.350852961085760029, -1.281975124255709124E-13, -121.1250000000000426 ) ) ;
#4598 = CARTESIAN_POINT ( 'NONE',  ( -3.464101615137725076, 5.999999999999979572, -166.0863248654052029 ) ) ;
#4599 = CARTESIAN_POINT ( 'NONE',  ( 114.4136751345946976, 1.414213562373145550, 1.414213562373034527 ) ) ;
#4600 = AXIS2_PLACEMENT_3D ( 'NONE', #15759, #4023, #13442 ) ;
#4601 = EDGE_LOOP ( 'NONE', ( #15848, #25840, #21184, #11667 ) ) ;
#4602 = CARTESIAN_POINT ( 'NONE',  ( 19.68750000000012790, 2.649519052838478661, 1.097466725451439196 ) ) ;
#4603 = CARTESIAN_POINT ( 'NONE',  ( 143.5386751345948255, -5.500000000000005329, 0.000000000000000000 ) ) ;
#4604 = EDGE_CURVE ( 'NONE', #24916, #27766, #29792, .T. ) ;
#4605 = EDGE_CURVE ( 'NONE', #21925, #6123, #29994, .T. ) ;
#4606 = ORIENTED_EDGE ( 'NONE', *, *, #16341, .T. ) ;
#4607 = CARTESIAN_POINT ( 'NONE',  ( 110.6872167782375840, 1.849990392679562001, 0.7662911109078287542 ) ) ;
#4608 = CARTESIAN_POINT ( 'NONE',  ( 118.5238248654050608, 0.8284271247463257382, -1.999999999999911626 ) ) ;
#4609 = CARTESIAN_POINT ( 'NONE',  ( 5.412658773652739619, 3.124999999999988898, -109.3169872981077901 ) ) ;
#4610 = CARTESIAN_POINT ( 'NONE',  ( 19.97617513459498539, -1.035533905932629173, -2.499999999999964473 ) ) ;
#4611 = CARTESIAN_POINT ( 'NONE',  ( -5.999999999999964473, 9.063946212346262433E-15, -174.8363248654052313 ) ) ;
#4612 = ORIENTED_EDGE ( 'NONE', *, *, #2655, .T. ) ;
#4613 = ORIENTED_EDGE ( 'NONE', *, *, #1013, .F. ) ;
#4614 = CARTESIAN_POINT ( 'NONE',  ( 106.2261751345945129, 2.000000000000122125, -0.8284271247460553989 ) ) ;
#4615 = CARTESIAN_POINT ( 'NONE',  ( 133.3125000000000284, 4.242640687119298093, -4.242640687119298093 ) ) ;
#4616 = ORIENTED_EDGE ( 'NONE', *, *, #10478, .T. ) ;
#4617 = CARTESIAN_POINT ( 'NONE',  ( -5.412658773652739619, 3.124999999999975131, -135.8169872981078186 ) ) ;
#4618 = CARTESIAN_POINT ( 'NONE',  ( 12.62500000000005329, 1.110223024625156540E-13, 2.649519052838056332 ) ) ;
#4619 =( LENGTH_UNIT ( ) NAMED_UNIT ( * ) SI_UNIT ( .MILLI., .METRE. ) );
#4620 = CARTESIAN_POINT ( 'NONE',  ( 19.25000000000009948, 1.110223024625156540E-13, 1.999999999999946265 ) ) ;
#4621 = LINE ( 'NONE', #14052, #19136 ) ;
#4622 = CARTESIAN_POINT ( 'NONE',  ( 2.775557561562891351E-14, -6.250000000000061284, -62.68301270189225249 ) ) ;
#4623 = CARTESIAN_POINT ( 'NONE',  ( 144.7351497308104058, 3.535533905932725318, -3.535533905932725318 ) ) ;
#4624 = CARTESIAN_POINT ( 'NONE',  ( 12.66367513459487526, -1.767766952966265404, 1.767766952966431937 ) ) ;
#4625 = CARTESIAN_POINT ( 'NONE',  ( -6.000000000000000888, 1.067854986875958443E-15, 7.560779664488942560E-35 ) ) ;
#4626 = CARTESIAN_POINT ( 'NONE',  ( 24.74512076645466152, -1.864212315884203441, -1.303982556562485851 ) ) ;
#4627 = CYLINDRICAL_SURFACE ( 'NONE', #27269, 2.499999999999999112 ) ;
#4628 = CARTESIAN_POINT ( 'NONE',  ( 108.3749999999998437, -1.767766952966209892, 1.767766952966431937 ) ) ;
#4629 = EDGE_CURVE ( 'NONE', #3499, #2708, #20482, .T. ) ;
#4630 = CARTESIAN_POINT ( 'NONE',  ( -5.196152422706573404, -3.000000000000002665, -95.21132486540517448 ) ) ;
#4631 = ADVANCED_FACE ( 'NONE', ( #3874 ), #15612, .T. ) ;
#4632 =( BOUNDED_CURVE ( )  B_SPLINE_CURVE ( 2, ( #6859, #16285, #13981, #23321, #11671, #17160, #2551, #2695, #28628 ),
 .UNSPECIFIED., .F., .T. ) 
 B_SPLINE_CURVE_WITH_KNOTS ( ( 3, 2, 2, 2, 3 ),
 ( 0.7472222222222222321, 0.7481481481481481177, 0.7500000000000000000, 0.7518518518518518823, 0.7527777777777777679 ),
 .UNSPECIFIED. ) 
 CURVE ( )  GEOMETRIC_REPRESENTATION_ITEM ( )  RATIONAL_B_SPLINE_CURVE ( ( 0.9330127018922194093, 0.9330127018922194093, 1.000000000000000000, 0.8660254037844388186, 1.000000000000000000, 0.8660254037844388186, 1.000000000000000000, 0.9330127018922194093, 0.9330127018922194093 ) ) 
 REPRESENTATION_ITEM ( '' )  );
#4633 = DIRECTION ( 'NONE',  ( 1.000000000000000000, 0.000000000000000000, 0.000000000000000000 ) ) ;
#4634 = CARTESIAN_POINT ( 'NONE',  ( 7.216878364870455975, -6.409875621278545621E-14, -143.3080127018922667 ) ) ;
#4635 = FILL_AREA_STYLE_COLOUR ( '', #24824 ) ;
#4636 = VERTEX_POINT ( 'NONE', #22334 ) ;
#4637 = CARTESIAN_POINT ( 'NONE',  ( 0.000000000000000000, 5.499999999999991118, -57.00000000000004974 ) ) ;
#4638 = CARTESIAN_POINT ( 'NONE',  ( -6.000000000000007105, -1.607695154586655129, -155.2693375672974412 ) ) ;
#4639 = CARTESIAN_POINT ( 'NONE',  ( -5.999999999999963585, -1.487416814333745711E-14, -171.8363248654052313 ) ) ;
#4640 = EDGE_LOOP ( 'NONE', ( #7307, #6228, #8668, #15125 ) ) ;
#4641 = CARTESIAN_POINT ( 'NONE',  ( 106.4374999999997442, -2.499999999999994671, 1.035533905932989551 ) ) ;
#4642 = CARTESIAN_POINT ( 'NONE',  ( 141.0000000000000284, 6.000000000000005329, 0.000000000000000000 ) ) ;
#4643 = CARTESIAN_POINT ( 'NONE',  ( 11.56250000000009059, -1.999999999999851674, -0.8284271247462354770 ) ) ;
#4644 = CARTESIAN_POINT ( 'NONE',  ( 7.216878364870455975, -6.409875621278545621E-14, -106.4419872981078470 ) ) ;
#4645 = AXIS2_PLACEMENT_3D ( 'NONE', #7752, #26483, #21908 ) ;
#4646 = MECHANICAL_DESIGN_GEOMETRIC_PRESENTATION_REPRESENTATION (  '', ( #14023 ), #7105 ) ;
#4647 = LINE ( 'NONE', #25847, #13158 ) ;
#4648 = CARTESIAN_POINT ( 'NONE',  ( 134.0625000000000284, -4.242640687119298093, 4.242640687119298093 ) ) ;
#4649 = CARTESIAN_POINT ( 'NONE',  ( 0.000000000000000000, 0.000000000000000000, 0.000000000000000000 ) ) ;
#4650 = CARTESIAN_POINT ( 'NONE',  ( 3.175426480543072749, 5.499999999999865885, -135.1250000000000000 ) ) ;
#4651 = ORIENTED_EDGE ( 'NONE', *, *, #3057, .F. ) ;
#4652 = ORIENTED_EDGE ( 'NONE', *, *, #5887, .F. ) ;
#4653 = VECTOR ( 'NONE', #6075, 1000.000000000000000 ) ;
#4654 = CARTESIAN_POINT ( 'NONE',  ( -4.763139720814407951, 2.749999999999946709, -67.25000000000002842 ) ) ;
#4655 = LINE ( 'NONE', #30315, #5762 ) ;
#4656 = DIRECTION ( 'NONE',  ( 0.000000000000000000, 0.000000000000000000, -1.000000000000000000 ) ) ;
#4657 = CARTESIAN_POINT ( 'NONE',  ( 114.2113248654050750, -1.999999999999890754, 0.000000000000000000 ) ) ;
#4658 = CARTESIAN_POINT ( 'NONE',  ( 106.8747167782375840, 2.775557561562891351E-14, 1.849990392679745632 ) ) ;
#4659 = CYLINDRICAL_SURFACE ( 'NONE', #312, 6.000000000000000888 ) ;
#4660 = EDGE_CURVE ( 'NONE', #26117, #7780, #13450, .T. ) ;
#4661 = CARTESIAN_POINT ( 'NONE',  ( 0.000000000000000000, 0.000000000000000000, 0.000000000000000000 ) ) ;
#4662 = CARTESIAN_POINT ( 'NONE',  ( 118.6252832217622029, 5.551115123125782702E-14, 1.849990392679634610 ) ) ;
#4663 = EDGE_CURVE ( 'NONE', #26866, #18250, #15991, .T. ) ;
#4664 = CARTESIAN_POINT ( 'NONE',  ( 0.000000000000000000, 5.499999999999991118, -151.5000000000000284 ) ) ;
#4665 = CARTESIAN_POINT ( 'NONE',  ( 140.0758535114726726, -9.341226305241869809, -7.537168216789017272 ) ) ;
#4666 = CARTESIAN_POINT ( 'NONE',  ( -3.175426480542816510, 5.499999999999865885, -137.8750000000000568 ) ) ;
#4667 = CARTESIAN_POINT ( 'NONE',  ( 3.608439182435180470, -6.249999999999997335, -158.5580127018922383 ) ) ;
#4668 = CARTESIAN_POINT ( 'NONE',  ( -4.763139720814407951, -2.750000000000016431, -82.00000000000001421 ) ) ;
#4669 = CARTESIAN_POINT ( 'NONE',  ( 0.000000000000000000, 5.499999999999991118, -67.50000000000000000 ) ) ;
#4670 = CARTESIAN_POINT ( 'NONE',  ( -9.999999999999980460, -60.00000000000001421, 3.000000000000002665 ) ) ;
#4671 = CARTESIAN_POINT ( 'NONE',  ( -4.999999999999886313, -10.00000000000000888, 7.500000000000007105 ) ) ;
#4672 = CARTESIAN_POINT ( 'NONE',  ( -5.999999999999962697, -1.607695154586733954, -175.3466878364870354 ) ) ;
#4673 = CARTESIAN_POINT ( 'NONE',  ( 155.5312500000000284, -2.485281374238556218, -6.000000000000005329 ) ) ;
#4674 = CARTESIAN_POINT ( 'NONE',  ( 21.18750000000019540, 0.8284271247462955401, 2.000000000000031530 ) ) ;
#4675 = AXIS2_PLACEMENT_3D ( 'NONE', #3868, #11289, #13443 ) ;
#4676 = FILL_AREA_STYLE ('',( #7137 ) ) ;
#4677 =( BOUNDED_CURVE ( )  B_SPLINE_CURVE ( 2, ( #7776, #5320, #5172, #19767, #24217, #8071, #17192, #10264, #14729 ),
 .UNSPECIFIED., .F., .F. ) 
 B_SPLINE_CURVE_WITH_KNOTS ( ( 3, 2, 2, 2, 3 ),
 ( 0.5249999999999999112, 0.5259259259259259078, 0.5277777777777777901, 0.5296296296296296724, 0.5305555555555555580 ),
 .UNSPECIFIED. ) 
 CURVE ( )  GEOMETRIC_REPRESENTATION_ITEM ( )  RATIONAL_B_SPLINE_CURVE ( ( 0.9330127018922194093, 0.9330127018922154125, 1.000000000000000000, 0.8660254037844388186, 1.000000000000000000, 0.8660254037844388186, 1.000000000000000000, 0.9330127018922194093, 0.9330127018922194093 ) ) 
 REPRESENTATION_ITEM ( '' )  );
#4678 = FACE_OUTER_BOUND ( 'NONE', #13386, .T. ) ;
#4679 = CARTESIAN_POINT ( 'NONE',  ( 118.8747167782375840, 5.551115123125782702E-14, 1.849990392679523588 ) ) ;
#4680 = DIRECTION ( 'NONE',  ( -7.147005652999508048E-36, 5.642372883946980038E-36, 1.000000000000000000 ) ) ;
#4681 = ORIENTED_EDGE ( 'NONE', *, *, #262, .F. ) ;
#4682 = CARTESIAN_POINT ( 'NONE',  ( 149.9062500000000568, 6.000000000000005329, -2.485281374238555774 ) ) ;
#4683 = CARTESIAN_POINT ( 'NONE',  ( 113.6252832217621460, 1.665334536937734811E-13, 1.849990392679745632 ) ) ;
#4684 = CARTESIAN_POINT ( 'NONE',  ( 11.64882486540532014, 2.500000000000144773, -1.035533905932809473 ) ) ;
#4685 = ORIENTED_EDGE ( 'NONE', *, *, #1779, .T. ) ;
#4686 = ORIENTED_EDGE ( 'NONE', *, *, #15120, .F. ) ;
#4687 = CIRCLE ( 'NONE', #29701, 0.5000000000000004441 ) ;
#4688 = ORIENTED_EDGE ( 'NONE', *, *, #10167, .F. ) ;
#4689 = CARTESIAN_POINT ( 'NONE',  ( 4.763139720814407951, -2.749999999999988454, -92.00000000000002842 ) ) ;
#4690 = CARTESIAN_POINT ( 'NONE',  ( -3.608439182435052128, -6.250000000000110134, -107.8080127018922667 ) ) ;
#4691 = VERTEX_POINT ( 'NONE', #1584 ) ;
#4692 = CARTESIAN_POINT ( 'NONE',  ( 0.8083154347086104474, 10.97740844234572677, -30.95886765600325319 ) ) ;
#4693 = CARTESIAN_POINT ( 'NONE',  ( 157.6726497308104058, -5.000000000000004441, 0.000000000000000000 ) ) ;
#4694 = CARTESIAN_POINT ( 'NONE',  ( -6.350852961085760029, -1.281975124255709124E-13, -166.1249999999999716 ) ) ;
#4695 = CARTESIAN_POINT ( 'NONE',  ( 6.000000000000000888, -1.859271017917181981E-14, -105.6636751345948397 ) ) ;
#4696 = LINE ( 'NONE', #9481, #7813 ) ;
#4697 = CARTESIAN_POINT ( 'NONE',  ( -6.000000000000007105, -1.607695154586655129, -68.26933756729739855 ) ) ;
#4698 = SHAPE_REPRESENTATION_RELATIONSHIP ( 'NONE' , 'NONE' ,  #13689, #15129 ) ;
#4699 = EDGE_CURVE ( 'NONE', #7475, #12687, #10989, .T. ) ;
#4700 = CARTESIAN_POINT ( 'NONE',  ( -3.175426480542816066, -5.500000000000057732, -171.8750000000000284 ) ) ;
#4701 = CYLINDRICAL_SURFACE ( 'NONE', #8619, 6.000000000000000888 ) ;
#4702 = CARTESIAN_POINT ( 'NONE',  ( 0.000000000000000000, 5.499999999999991118, -157.5000000000000284 ) ) ;
#4703 = CARTESIAN_POINT ( 'NONE',  ( 112.9374999999997868, 2.500000000000114575, -1.035533905932448873 ) ) ;
#4704 = CARTESIAN_POINT ( 'NONE',  ( 0.000000000000000000, 5.499999999999991118, -102.0000000000000284 ) ) ;
#4705 = CARTESIAN_POINT ( 'NONE',  ( 5.196152422706629359, -2.999999999999988898, -159.2113248654052313 ) ) ;
#4706 = DIRECTION ( 'NONE',  ( 1.000000000000000000, 0.000000000000000000, 0.000000000000000000 ) ) ;
#4707 = CARTESIAN_POINT ( 'NONE',  ( 4.763139720814407951, -2.749999999999988454, -89.00000000000002842 ) ) ;
#4708 = DIRECTION ( 'NONE',  ( 0.000000000000000000, 0.000000000000000000, -1.000000000000000000 ) ) ;
#4709 = CARTESIAN_POINT ( 'NONE',  ( 160.2336002691896226, -4.999999999999989342, 2.071067811865468400 ) ) ;
#4710 = CARTESIAN_POINT ( 'NONE',  ( 135.0000000000002842, -7.177308154933044193, 8.449997537985554530 ) ) ;
#4711 = VERTEX_POINT ( 'NONE', #25073 ) ;
#4712 = CARTESIAN_POINT ( 'NONE',  ( 12.56250000000004619, 2.649519052838298805, -1.097466725451739622 ) ) ;
#4713 = CARTESIAN_POINT ( 'NONE',  ( 111.9374999999997868, 2.500000000000114575, -1.035533905932508825 ) ) ;
#4714 = CARTESIAN_POINT ( 'NONE',  ( 136.0000000000000284, 0.000000000000000000, -11.00000000000000355 ) ) ;
#4715 = CARTESIAN_POINT ( 'NONE',  ( 104.8752832217621602, -1.849990392679495832, 2.220446049250313081E-13 ) ) ;
#4716 = FACE_OUTER_BOUND ( 'NONE', #1667, .T. ) ;
#4717 =( BOUNDED_CURVE ( )  B_SPLINE_CURVE ( 2, ( #14421, #5136, #23202, #23046, #28491, #1985, #2841, #30240, #24043 ),
 .UNSPECIFIED., .F., .T. ) 
 B_SPLINE_CURVE_WITH_KNOTS ( ( 3, 2, 2, 2, 3 ),
 ( 0.3529411764705882026, 0.3602941176470587648, 0.3676470588235294379, 0.3750000000000000000, 0.3823529411764705621 ),
 .UNSPECIFIED. ) 
 CURVE ( )  GEOMETRIC_REPRESENTATION_ITEM ( )  RATIONAL_B_SPLINE_CURVE ( ( 1.000000000000000000, 0.9238795325112867385, 1.000000000000000000, 0.9238795325112867385, 1.000000000000000000, 0.9238795325112867385, 1.000000000000000000, 0.9238795325112867385, 1.000000000000000000 ) ) 
 REPRESENTATION_ITEM ( '' )  );
#4718 = AXIS2_PLACEMENT_3D ( 'NONE', #23871, #12681, #16986 ) ;
#4719 = ORIENTED_EDGE ( 'NONE', *, *, #21426, .T. ) ;
#4720 = CYLINDRICAL_SURFACE ( 'NONE', #15811, 0.5000000000000004441 ) ;
#4721 = CARTESIAN_POINT ( 'NONE',  ( 105.2497167782374845, -1.308140751793585022, -1.308140751793640533 ) ) ;
#4722 = AXIS2_PLACEMENT_3D ( 'NONE', #9789, #21473, #28795 ) ;
#4723 = ORIENTED_EDGE ( 'NONE', *, *, #8408, .F. ) ;
#4724 = CARTESIAN_POINT ( 'NONE',  ( -40.00000000000000000, -20.00000000000021316, 3.000000000000002665 ) ) ;
#4725 =( BOUNDED_CURVE ( )  B_SPLINE_CURVE ( 2, ( #28572, #16951, #26279, #23987, #14787, #2930, #10018, #19397, #28719 ),
 .UNSPECIFIED., .F., .T. ) 
 B_SPLINE_CURVE_WITH_KNOTS ( ( 3, 2, 2, 2, 3 ),
 ( 0.1764705882352941568, 0.1838235294117647189, 0.1911764705882352811, 0.1985294117647058432, 0.2058823529411765163 ),
 .UNSPECIFIED. ) 
 CURVE ( )  GEOMETRIC_REPRESENTATION_ITEM ( )  RATIONAL_B_SPLINE_CURVE ( ( 1.000000000000000000, 0.9238795325112867385, 1.000000000000000000, 0.9238795325112867385, 1.000000000000000000, 0.9238795325112867385, 1.000000000000000000, 0.9238795325112867385, 1.000000000000000000 ) ) 
 REPRESENTATION_ITEM ( '' )  );
#4726 = EDGE_CURVE ( 'NONE', #26400, #15757, #29841, .T. ) ;
#4727 = CARTESIAN_POINT ( 'NONE',  ( 152.5312500000000000, -2.485281374238555774, -6.000000000000005329 ) ) ;
#4728 = VERTEX_POINT ( 'NONE', #7106 ) ;
#4729 = EDGE_CURVE ( 'NONE', #9839, #11992, #29657, .T. ) ;
#4730 = CARTESIAN_POINT ( 'NONE',  ( -3.175426480542816510, -5.500000000000057732, -111.8750000000000568 ) ) ;
#4731 = CARTESIAN_POINT ( 'NONE',  ( 23.75000000000015987, -1.873492889144845464, 1.873492889144900975 ) ) ;
#4732 = CARTESIAN_POINT ( 'NONE',  ( 5.412658773652712085, -3.125000000000086153, -129.9330127018922383 ) ) ;
#4733 = ORIENTED_EDGE ( 'NONE', *, *, #6608, .T. ) ;
#4734 = CARTESIAN_POINT ( 'NONE',  ( -4.999999999999879208, -71.00000000000002842, 4.000000000000003553 ) ) ;
#4735 = CARTESIAN_POINT ( 'NONE',  ( -3.608439182435052128, -6.250000000000110134, -166.9419872981078470 ) ) ;
#4736 = CARTESIAN_POINT ( 'NONE',  ( 108.4374999999998863, -2.499999999999934719, 1.035533905932929599 ) ) ;
#4737 = SURFACE_SIDE_STYLE ('',( #9813 ) ) ;
#4738 = VECTOR ( 'NONE', #14636, 1000.000000000000000 ) ;
#4739 = ORIENTED_EDGE ( 'NONE', *, *, #17183, .T. ) ;
#4740 = CARTESIAN_POINT ( 'NONE',  ( 0.7548275425895982771, -15.52547035223602734, -8.075280843867185254 ) ) ;
#4741 = EDGE_CURVE ( 'NONE', #8028, #25601, #6332, .T. ) ;
#4742 = CARTESIAN_POINT ( 'NONE',  ( 5.196152422706629359, 3.000000000000002665, -95.96132486540520290 ) ) ;
#4743 = DIRECTION ( 'NONE',  ( 0.000000000000000000, 0.000000000000000000, 1.000000000000000000 ) ) ;
#4744 = CARTESIAN_POINT ( 'NONE',  ( -4.763139720814407951, -2.750000000000016431, -178.0000000000000568 ) ) ;
#4745 = CARTESIAN_POINT ( 'NONE',  ( 106.5002832217622881, 1.308140751793696044, 1.308140751793640533 ) ) ;
#4746 = CARTESIAN_POINT ( 'NONE',  ( 2.775557561562891351E-14, 6.250000000000033751, -174.4330127018922667 ) ) ;
#4747 = CARTESIAN_POINT ( 'NONE',  ( -0.2003331987396576308, -9.399833400630168256, -4.385453238887252247 ) ) ;
#4748 = CYLINDRICAL_SURFACE ( 'NONE', #17264, 2.000000000000012879 ) ;
#4749 = CARTESIAN_POINT ( 'NONE',  ( 160.2059167087800802, -11.22359236516978775, -4.246869790297142622 ) ) ;
#4750 = CARTESIAN_POINT ( 'NONE',  ( 0.000000000000000000, 5.499999999999991118, -121.5000000000000568 ) ) ;
#4751 = CARTESIAN_POINT ( 'NONE',  ( 135.0000000000000284, -7.800712729749759156, -7.983520772873845317 ) ) ;
#4752 = ORIENTED_EDGE ( 'NONE', *, *, #12313, .F. ) ;
#4753 = CARTESIAN_POINT ( 'NONE',  ( 22.06250000000015632, -2.649519052838238409, 1.097466725451559322 ) ) ;
#4754 = LINE ( 'NONE', #16777, #4495 ) ;
#4755 = CARTESIAN_POINT ( 'NONE',  ( 143.3511751345948255, -3.889087296526011706, 3.889087296526011706 ) ) ;
#4756 = CARTESIAN_POINT ( 'NONE',  ( 116.7261751345945981, -1.999999999999911626, 0.8284271247463557142 ) ) ;
#4757 = AXIS2_PLACEMENT_3D ( 'NONE', #3047, #2461, #21663 ) ;
#4758 = VERTEX_POINT ( 'NONE', #18508 ) ;
#4759 = CIRCLE ( 'NONE', #20466, 11.00000000000000355 ) ;
#4760 = CARTESIAN_POINT ( 'NONE',  ( 151.5863248654052313, 0.000000000000000000, 5.500000000000005329 ) ) ;
#4761 = CARTESIAN_POINT ( 'NONE',  ( 17.39882486540526685, -1.035533905932749299, -2.499999999999964473 ) ) ;
#4762 = CARTESIAN_POINT ( 'NONE',  ( 6.000000000000000888, 1.743066579297358182E-13, -95.16367513459482552 ) ) ;
#4763 = CARTESIAN_POINT ( 'NONE',  ( 140.3363248654052029, 0.000000000000000000, -5.500000000000005329 ) ) ;
#4764 = MECHANICAL_DESIGN_GEOMETRIC_PRESENTATION_REPRESENTATION (  '', ( #28299 ), #30267 ) ;
#4765 = ORIENTED_EDGE ( 'NONE', *, *, #19178, .F. ) ;
#4766 = CARTESIAN_POINT ( 'NONE',  ( 3.464101615137852974, 5.999999999999884537, -141.4136751345948255 ) ) ;
#4767 = CARTESIAN_POINT ( 'NONE',  ( 136.5000000000000284, 6.000000000000005329, 0.000000000000000000 ) ) ;
#4768 = EDGE_CURVE ( 'NONE', #8327, #14623, #21106, .T. ) ;
#4769 = ORIENTED_EDGE ( 'NONE', *, *, #3715, .T. ) ;
#4770 = AXIS2_PLACEMENT_3D ( 'NONE', #6350, #22660, #6209 ) ;
#4771 = CARTESIAN_POINT ( 'NONE',  ( 2.775557561562891351E-14, -6.250000000000061284, -142.8169872981078186 ) ) ;
#4772 = CARTESIAN_POINT ( 'NONE',  ( 10.50000000000012079, 1.873492889145123019, 1.873492889144845464 ) ) ;
#4773 = CARTESIAN_POINT ( 'NONE',  ( 0.000000000000000000, 5.999999999999977796, -151.2113248654052313 ) ) ;
#4774 = COLOUR_RGB ( '', 0.72549020, 0.75294118, 0.79215686) ;
#4775 = CARTESIAN_POINT ( 'NONE',  ( 20.12500000000011369, 1.414213562373201061, 1.414213562373034527 ) ) ;
#4776 = CARTESIAN_POINT ( 'NONE',  ( 0.07033120956265798140, -15.06949959929781357, 8.898246228163568361 ) ) ;
#4777 = EDGE_CURVE ( 'NONE', #379, #22958, #27831, .T. ) ;
#4778 = EDGE_CURVE ( 'NONE', #6046, #21961, #16371, .T. ) ;
#4779 = CARTESIAN_POINT ( 'NONE',  ( 146.0476497308104058, 0.000000000000000000, -5.000000000000004441 ) ) ;
#4780 = CARTESIAN_POINT ( 'NONE',  ( 0.000000000000000000, 5.999999999999977796, -102.2886751345948255 ) ) ;
#4781 = CARTESIAN_POINT ( 'NONE',  ( 0.000000000000000000, 0.000000000000000000, 0.000000000000000000 ) ) ;
#4782 = LINE ( 'NONE', #4625, #17835 ) ;
#4783 = CARTESIAN_POINT ( 'NONE',  ( 24.84150635094622572, -1.291286745249641628E-13, -2.158493649053927044 ) ) ;
#4784 = CARTESIAN_POINT ( 'NONE',  ( -5.196152422706601826, 2.999999999999975131, -113.4613248654052171 ) ) ;
#4785 = CARTESIAN_POINT ( 'NONE',  ( 110.9999999999999147, 2.500000000000057732, 0.000000000000000000 ) ) ;
#4786 = CARTESIAN_POINT ( 'NONE',  ( 14.47617513459494099, 1.035533905932809473, 2.500000000000024425 ) ) ;
#4787 = ORIENTED_EDGE ( 'NONE', *, *, #16682, .T. ) ;
#4788 = CARTESIAN_POINT ( 'NONE',  ( 3.175426480543072749, 5.499999999999865885, -54.12500000000003553 ) ) ;
#4789 = DIRECTION ( 'NONE',  ( 1.000000000000000000, -0.000000000000000000, -0.000000000000000000 ) ) ;
#4790 = VERTEX_POINT ( 'NONE', #11460 ) ;
#4791 = CARTESIAN_POINT ( 'NONE',  ( 120.3122167782375413, -0.7662911109077686911, -1.849990392679411677 ) ) ;
#4792 = CARTESIAN_POINT ( 'NONE',  ( 142.7812500000000568, 2.485281374238585972, 6.000000000000005329 ) ) ;
#4793 = CARTESIAN_POINT ( 'NONE',  ( 3.608439182435180470, 6.249999999999982236, -100.1919872981078186 ) ) ;
#4794 = DIRECTION ( 'NONE',  ( -7.147005652999508048E-36, 5.642372883946980038E-36, 1.000000000000000000 ) ) ;
#4795 = AXIS2_PLACEMENT_3D ( 'NONE', #2938, #21705, #12653 ) ;
#4796 = CARTESIAN_POINT ( 'NONE',  ( 133.1250000000000284, 0.000000000000000000, -6.000000000000005329 ) ) ;
#4797 = CARTESIAN_POINT ( 'NONE',  ( 116.3749999999998579, -1.767766952966209892, 1.767766952966542959 ) ) ;
#4798 = ADVANCED_FACE ( 'NONE', ( #21250 ), #16525, .T. ) ;
#4799 = CARTESIAN_POINT ( 'NONE',  ( 4.763139720814407951, -2.749999999999988454, -134.0000000000000000 ) ) ;
#4800 = ORIENTED_EDGE ( 'NONE', *, *, #18705, .T. ) ;
#4801 = VECTOR ( 'NONE', #2571, 1000.000000000000000 ) ;
#4802 = EDGE_LOOP ( 'NONE', ( #28213, #7708, #15503, #19545 ) ) ;
#4803 =( LENGTH_UNIT ( ) NAMED_UNIT ( * ) SI_UNIT ( .MILLI., .METRE. ) );
#4804 = CARTESIAN_POINT ( 'NONE',  ( -3.175426480542816510, -5.500000000000057732, -68.37500000000002842 ) ) ;
#4805 = CARTESIAN_POINT ( 'NONE',  ( 140.2574251345947687, -2.278174593051702335, 5.500000000000323297 ) ) ;
#4806 = CARTESIAN_POINT ( 'NONE',  ( -5.196152422706601826, 2.999999999999975131, -66.03867513459482552 ) ) ;
#4807 = EDGE_CURVE ( 'NONE', #27377, #27416, #12654, .T. ) ;
#4808 = CARTESIAN_POINT ( 'NONE',  ( 5.412658773652712085, -3.125000000000086153, -81.93301270189223828 ) ) ;
#4809 =( BOUNDED_CURVE ( )  B_SPLINE_CURVE ( 2, ( #12414, #26480, #14276, #2993, #12267, #28495, #23617, #21306, #7750 ),
 .UNSPECIFIED., .F., .T. ) 
 B_SPLINE_CURVE_WITH_KNOTS ( ( 3, 2, 2, 2, 3 ),
 ( 0.8527777777777778567, 0.8537037037037037424, 0.8555555555555556246, 0.8574074074074073959, 0.8583333333333332815 ),
 .UNSPECIFIED. ) 
 CURVE ( )  GEOMETRIC_REPRESENTATION_ITEM ( )  RATIONAL_B_SPLINE_CURVE ( ( 0.9330127018922194093, 0.9330127018922234061, 1.000000000000000000, 0.8660254037844388186, 1.000000000000000000, 0.8660254037844388186, 1.000000000000000000, 0.9330127018922234061, 0.9330127018922194093 ) ) 
 REPRESENTATION_ITEM ( '' )  );
#4810 = CARTESIAN_POINT ( 'NONE',  ( 119.8363248654050039, 1.414213562373201061, 1.414213562373367594 ) ) ;
#4811 = CARTESIAN_POINT ( 'NONE',  ( 105.5622167782374419, 1.849990392679591977, -0.7662911109075883909 ) ) ;
#4812 = CARTESIAN_POINT ( 'NONE',  ( 140.5126539824821634, -11.05214782318283184, 4.674845224361170004 ) ) ;
#4813 = CARTESIAN_POINT ( 'NONE',  ( 6.000000000000000888, 1.743066579297358182E-13, -61.58632486540521001 ) ) ;
#4814 = CARTESIAN_POINT ( 'NONE',  ( 120.1877832217620750, 0.7662911109077987781, -1.849990392679532247 ) ) ;
#4815 = CONTEXT_DEPENDENT_SHAPE_REPRESENTATION ( #29468, #16095 ) ;
#4816 = CARTESIAN_POINT ( 'NONE',  ( 4.763139720814407951, 2.750000000000002665, -148.7500000000000568 ) ) ;
#4817 = DIRECTION ( 'NONE',  ( 1.000000000000000000, 5.551115123125765446E-17, 2.220446049250314560E-16 ) ) ;
#4818 = CARTESIAN_POINT ( 'NONE',  ( 2.775557561562891351E-14, -6.250000000000061284, -160.1830127018922667 ) ) ;
#4819 =( NAMED_UNIT ( * ) PLANE_ANGLE_UNIT ( ) SI_UNIT ( $, .RADIAN. ) );
#4820 = DIRECTION ( 'NONE',  ( -7.147005652999508048E-36, 5.642372883946980038E-36, 1.000000000000000000 ) ) ;
#4821 = CARTESIAN_POINT ( 'NONE',  ( 13.27382486540526862, -2.499999999999904521, -1.035533905932749299 ) ) ;
#4822 = CARTESIAN_POINT ( 'NONE',  ( 4.763139720814407951, -2.749999999999988454, -62.00000000000000000 ) ) ;
#4823 = CARTESIAN_POINT ( 'NONE',  ( 115.7886751345947118, -1.999999999999974021, 0.000000000000000000 ) ) ;
#4824 = CARTESIAN_POINT ( 'NONE',  ( 143.3586002691896226, 2.071067811865468400, 4.999999999999989342 ) ) ;
#4825 = DIRECTION ( 'NONE',  ( -7.147005652999508048E-36, 5.642372883946980038E-36, 1.000000000000000000 ) ) ;
#4826 = CARTESIAN_POINT ( 'NONE',  ( 155.3437500000000284, -6.000000000000005329, -2.485281374238556218 ) ) ;
#4827 = SURFACE_SIDE_STYLE ('',( #2241 ) ) ;
#4828 = CARTESIAN_POINT ( 'NONE',  ( 17.00000000000015277, 2.000000000000112799, 0.000000000000000000 ) ) ;
#4829 = PRESENTATION_STYLE_ASSIGNMENT (( #12095 ) ) ;
#4830 = CARTESIAN_POINT ( 'NONE',  ( 119.9136751345946266, -1.414213562373228816, -1.414213562373034527 ) ) ;
#4831 = CARTESIAN_POINT ( 'NONE',  ( 117.3747167782375271, 0.000000000000000000, -1.849990392679301543 ) ) ;
#4832 = DIRECTION ( 'NONE',  ( 0.000000000000000000, 0.000000000000000000, -1.000000000000000000 ) ) ;
#4833 = ORIENTED_EDGE ( 'NONE', *, *, #17918, .F. ) ;
#4834 = CARTESIAN_POINT ( 'NONE',  ( 152.3437500000000568, -6.000000000000005329, -2.485281374238555774 ) ) ;
#4835 = CARTESIAN_POINT ( 'NONE',  ( 115.4377832217621744, 1.849990392679591977, 0.7662911109078888172 ) ) ;
#4836 = EDGE_CURVE ( 'NONE', #29837, #14973, #4647, .T. ) ;
#4837 = CARTESIAN_POINT ( 'NONE',  ( 140.0255071013316410, -11.51275355066580453, 4.738782956804194590 ) ) ;
#4838 = VERTEX_POINT ( 'NONE', #4499 ) ;
#4839 = EDGE_CURVE ( 'NONE', #27076, #23117, #13922, .T. ) ;
#4840 = CARTESIAN_POINT ( 'NONE',  ( 21.18750000000019540, 0.8284271247462955401, 2.000000000000031530 ) ) ;
#4841 = ORIENTED_EDGE ( 'NONE', *, *, #2677, .T. ) ;
#4842 = CARTESIAN_POINT ( 'NONE',  ( 6.350852961086080661, -9.614813431917819062E-14, -85.87500000000005684 ) ) ;
#4843 = EDGE_LOOP ( 'NONE', ( #16138, #22753, #11096, #1313 ) ) ;
#4844 = CARTESIAN_POINT ( 'NONE',  ( 155.8913997308104342, -2.071067811865468400, 4.999999999999989342 ) ) ;
#4845 = CARTESIAN_POINT ( 'NONE',  ( 159.5550748654052313, -5.500000000000012434, -2.278174593052012309 ) ) ;
#4846 = CARTESIAN_POINT ( 'NONE',  ( 136.0000000000000284, -8.798545334315202027, 8.160000000000007248 ) ) ;
#4847 = CARTESIAN_POINT ( 'NONE',  ( -6.350852961085760029, -1.281975124255709124E-13, -175.1250000000000284 ) ) ;
#4848 = CARTESIAN_POINT ( 'NONE',  ( -2.000000000000000000, 3.559516622919861969E-16, -200.0000000000000000 ) ) ;
#4849 = CARTESIAN_POINT ( 'NONE',  ( -4.763139720814407951, -2.750000000000016431, -151.0000000000000284 ) ) ;
#4850 = CARTESIAN_POINT ( 'NONE',  ( 113.8124999999998437, 1.035533905932749299, -2.499999999999904521 ) ) ;
#4851 =( BOUNDED_CURVE ( )  B_SPLINE_CURVE ( 2, ( #20667, #8990, #10861, #27244, #8366, #3590, #1758, #15791, #15476 ),
 .UNSPECIFIED., .F., .F. ) 
 B_SPLINE_CURVE_WITH_KNOTS ( ( 3, 2, 2, 2, 3 ),
 ( 0.1625000000000006162, 0.1687500000000003997, 0.1750000000000001554, 0.1812499999999999112, 0.1874999999999996947 ),
 .UNSPECIFIED. ) 
 CURVE ( )  GEOMETRIC_REPRESENTATION_ITEM ( )  RATIONAL_B_SPLINE_CURVE ( ( 0.9999999999999925615, 0.9238795325112941770, 1.000000000000000000, 0.9238795325112867385, 1.000000000000000000, 0.9238795325112867385, 1.000000000000000000, 0.9238795325112904022, 0.9999999999999963363 ) ) 
 REPRESENTATION_ITEM ( '' )  );
#4852 = AXIS2_PLACEMENT_3D ( 'NONE', #279, #2295, #11699 ) ;
#4853 = CARTESIAN_POINT ( 'NONE',  ( -2.775557561562891351E-14, -5.500000000000115463, -102.7500000000000142 ) ) ;
#4854 = CARTESIAN_POINT ( 'NONE',  ( 21.21132486540527751, -2.499999999999891198, -2.220446049250313081E-13 ) ) ;
#4855 = DIRECTION ( 'NONE',  ( 7.147005652999508048E-36, -5.642372883946980038E-36, -1.000000000000000000 ) ) ;
#4857 = CARTESIAN_POINT ( 'NONE',  ( -4.763139720814407951, -2.750000000000016431, -91.00000000000002842 ) ) ;
#4856 = CARTESIAN_POINT ( 'NONE',  ( -2.775557561562891351E-14, -5.500000000000115463, -155.2500000000000000 ) ) ;
#4858 = CARTESIAN_POINT ( 'NONE',  ( 0.000000000000000000, -9.500000000000008882, -5.000000000000004441 ) ) ;
#4859 = VERTEX_POINT ( 'NONE', #2497 ) ;
#4860 = CARTESIAN_POINT ( 'NONE',  ( 24.93750000000011013, 2.000000000000151879, -0.8284271247462354770 ) ) ;
#4861 = CARTESIAN_POINT ( 'NONE',  ( 111.8124999999997584, 1.035533905932779275, -2.499999999999964473 ) ) ;
#4862 = CARTESIAN_POINT ( 'NONE',  ( -5.196152422706601826, 2.999999999999975131, -126.0386751345948824 ) ) ;
#4863 = CARTESIAN_POINT ( 'NONE',  ( 105.9377832217620323, -1.849990392679441875, -0.7662911109074682647 ) ) ;
#4864 = DIRECTION ( 'NONE',  ( -1.000000000000000000, -1.665334536937736783E-16, -2.220446049250315546E-16 ) ) ;
#4865 = VERTEX_POINT ( 'NONE', #30304 ) ;
#4866 = CARTESIAN_POINT ( 'NONE',  ( 15.33632486540528816, -1.767766952966265404, -1.767766952966487448 ) ) ;
#4867 = CARTESIAN_POINT ( 'NONE',  ( -1.000000000000000888, 9.000000000000007105, -5.000000000000004441 ) ) ;
#4868 = ORIENTED_EDGE ( 'NONE', *, *, #28138, .F. ) ;
#4869 = CARTESIAN_POINT ( 'NONE',  ( 6.000000000000000888, 1.743066579297358182E-13, -52.58632486540518869 ) ) ;
#4870 = EDGE_CURVE ( 'NONE', #13568, #21900, #23464, .T. ) ;
#4871 = CARTESIAN_POINT ( 'NONE',  ( 153.1875000000000284, 4.242640687119269671, 4.242640687119298093 ) ) ;
#4872 = ORIENTED_EDGE ( 'NONE', *, *, #570, .T. ) ;
#4873 = CARTESIAN_POINT ( 'NONE',  ( -6.350852961085760029, -1.281975124255709124E-13, -115.1250000000000000 ) ) ;
#4874 = CARTESIAN_POINT ( 'NONE',  ( 21.50000000000010303, 1.873492889145067508, 1.873492889144734441 ) ) ;
#4875 = CARTESIAN_POINT ( 'NONE',  ( -3.608439182435052128, -6.250000000000110134, -130.3080127018922383 ) ) ;
#4876 = VERTEX_POINT ( 'NONE', #25694 ) ;
#4877 = FACE_OUTER_BOUND ( 'NONE', #1315, .T. ) ;
#4878 = CARTESIAN_POINT ( 'NONE',  ( -5.412658773652684552, -3.125000000000099920, -167.0669872981078186 ) ) ;
#4879 = CARTESIAN_POINT ( 'NONE',  ( 107.8749999999999858, 1.767766952966431937, -1.767766952966209892 ) ) ;
#4880 = FACE_OUTER_BOUND ( 'NONE', #7545, .T. ) ;
#4881 = VECTOR ( 'NONE', #11006, 1000.000000000000000 ) ;
#4882 = LINE ( 'NONE', #25792, #14374 ) ;
#4883 =( NAMED_UNIT ( * ) SI_UNIT ( $, .STERADIAN. ) SOLID_ANGLE_UNIT ( ) );
#4884 = CARTESIAN_POINT ( 'NONE',  ( -2.775557561562891351E-14, -5.500000000000115463, -177.7500000000000284 ) ) ;
#4885 = CARTESIAN_POINT ( 'NONE',  ( 108.8127832217621176, -1.849990392679501827, 0.7662911109078287542 ) ) ;
#4886 = CARTESIAN_POINT ( 'NONE',  ( 6.000000000000000888, 1.743066579297358182E-13, -111.0863248654051887 ) ) ;
#4887 = CARTESIAN_POINT ( 'NONE',  ( 7.216878364870455975, -6.409875621278545621E-14, -180.8080127018922099 ) ) ;
#4888 = CYLINDRICAL_SURFACE ( 'NONE', #1331, 0.5000000000000004441 ) ;
#4889 = CARTESIAN_POINT ( 'NONE',  ( 6.000000000000000888, 1.743066579297358182E-13, -53.16367513459481131 ) ) ;
#4890 =( BOUNDED_CURVE ( )  B_SPLINE_CURVE ( 2, ( #14281, #10092, #21311, #2416, #19315, #9939, #28195, #24051, #19462 ),
 .UNSPECIFIED., .F., .T. ) 
 B_SPLINE_CURVE_WITH_KNOTS ( ( 3, 2, 2, 2, 3 ),
 ( 0.6176470588235294379, 0.6250000000000000000, 0.6323529411764705621, 0.6397058823529411242, 0.6470588235294116863 ),
 .UNSPECIFIED. ) 
 CURVE ( )  GEOMETRIC_REPRESENTATION_ITEM ( )  RATIONAL_B_SPLINE_CURVE ( ( 1.000000000000000000, 0.9238795325112867385, 1.000000000000000000, 0.9238795325112867385, 1.000000000000000000, 0.9238795325112867385, 1.000000000000000000, 0.9238795325112867385, 1.000000000000000000 ) ) 
 REPRESENTATION_ITEM ( '' )  );
#4891 = CARTESIAN_POINT ( 'NONE',  ( -4.763139720814407951, 2.749999999999946709, -113.7500000000000142 ) ) ;
#4892 = CARTESIAN_POINT ( 'NONE',  ( 135.0000000000000284, -7.345688489539636379, -8.346135564586871780 ) ) ;
#4893 = CARTESIAN_POINT ( 'NONE',  ( -5.196152422706601826, 2.999999999999975131, -145.5386751345948539 ) ) ;
#4894 = VERTEX_POINT ( 'NONE', #23413 ) ;
#4895 = EDGE_CURVE ( 'NONE', #26645, #14008, #4357, .T. ) ;
#4896 = DIRECTION ( 'NONE',  ( -7.147005652999508048E-36, 5.642372883946980038E-36, 1.000000000000000000 ) ) ;
#4897 = AXIS2_PLACEMENT_3D ( 'NONE', #1680, #15552, #13248 ) ;
#4898 = LINE ( 'NONE', #23667, #11160 ) ;
#4899 = CARTESIAN_POINT ( 'NONE',  ( 116.6636751345947829, -1.414213562373090038, 1.414213562373256572 ) ) ;
#4900 = MECHANICAL_DESIGN_GEOMETRIC_PRESENTATION_REPRESENTATION (  '', ( #10316 ), #16277 ) ;
#4901 = EDGE_LOOP ( 'NONE', ( #19359, #27673, #23972, #12053 ) ) ;
#4902 = FACE_OUTER_BOUND ( 'NONE', #2580, .T. ) ;
#4903 = CARTESIAN_POINT ( 'NONE',  ( 17.22617513459484329, 2.500000000000144773, -1.035533905932689347 ) ) ;
#4904 = CARTESIAN_POINT ( 'NONE',  ( 5.196152422706629359, -2.999999999999988898, -176.2886751345948539 ) ) ;
#4905 = CARTESIAN_POINT ( 'NONE',  ( 6.000000000000052403, -1.607695154586662678, -95.23066243270257303 ) ) ;
#4906 = ADVANCED_FACE ( 'NONE', ( #929 ), #3284, .T. ) ;
#4907 = LINE ( 'NONE', #7229, #7393 ) ;
#4908 = EDGE_LOOP ( 'NONE', ( #15687, #13085, #7514, #17307 ) ) ;
#4909 = ORIENTED_EDGE ( 'NONE', *, *, #19252, .F. ) ;
#4910 = CARTESIAN_POINT ( 'NONE',  ( 106.2886751345948255, 2.000000000000029310, 1.110223024625156540E-13 ) ) ;
#4911 = CARTESIAN_POINT ( 'NONE',  ( 134.5312500000000568, -2.485281374238555774, -6.000000000000005329 ) ) ;
#4912 = ORIENTED_EDGE ( 'NONE', *, *, #23390, .F. ) ;
#4913 = CARTESIAN_POINT ( 'NONE',  ( -5.412658773652684552, -3.125000000000099920, -141.5669872981077901 ) ) ;
#4914 = SURFACE_STYLE_FILL_AREA ( #14199 ) ;
#4915 = PRESENTATION_LAYER_ASSIGNMENT (  '', '', ( #25508 ) ) ;
#4916 = CARTESIAN_POINT ( 'NONE',  ( 18.37500000000008527, -1.414213562373090038, 1.414213562372867994 ) ) ;
#4917 = CARTESIAN_POINT ( 'NONE',  ( 117.6636751345947545, -1.414213562373034527, 1.414213562373367594 ) ) ;
#4918 = CARTESIAN_POINT ( 'NONE',  ( 137.7038997308103774, 2.071067811865468400, 4.999999999999989342 ) ) ;
#4919 = CARTESIAN_POINT ( 'NONE',  ( -3.464101615137725076, 5.999999999999979572, -102.1636751345948255 ) ) ;
#4920 = CARTESIAN_POINT ( 'NONE',  ( -5.999999999999962697, 3.323446944526963260E-14, -161.3363248654052597 ) ) ;
#4921 = CARTESIAN_POINT ( 'NONE',  ( -5.999999999999919176, 1.607695154586804565, -146.4033121635129930 ) ) ;
#4922 = AXIS2_PLACEMENT_3D ( 'NONE', #25645, #6294, #1841 ) ;
#4923 = CARTESIAN_POINT ( 'NONE',  ( -0.07769256095284393648, -15.23231281889969679, 7.500000000000007105 ) ) ;
#4924 = FACE_OUTER_BOUND ( 'NONE', #6201, .T. ) ;
#4925 = CARTESIAN_POINT ( 'NONE',  ( 110.5624999999998295, -2.499999999999994671, -1.035533905932568999 ) ) ;
#4926 = CARTESIAN_POINT ( 'NONE',  ( 3.464101615137757051, -5.999999999999979572, -142.8363248654052029 ) ) ;
#4927 = FILL_AREA_STYLE ('',( #18798 ) ) ;
#4928 = FILL_AREA_STYLE ('',( #4635 ) ) ;
#4929 = ORIENTED_EDGE ( 'NONE', *, *, #21716, .T. ) ;
#4930 = EDGE_CURVE ( 'NONE', #6568, #15139, #1091, .T. ) ;
#4931 = CARTESIAN_POINT ( 'NONE',  ( 0.000000000000000000, -5.999999999999991118, -106.9613248654052171 ) ) ;
#4932 = CARTESIAN_POINT ( 'NONE',  ( 0.000000000000000000, 5.999999999999977796, -52.78867513459483973 ) ) ;
#4933 = DIRECTION ( 'NONE',  ( -1.000000000000000000, -1.665334536937731113E-16, 1.526556658859586792E-16 ) ) ;
#4934 = CARTESIAN_POINT ( 'NONE',  ( 0.000000000000000000, -5.999999999999991118, -178.9613248654052313 ) ) ;
#4935 = VERTEX_POINT ( 'NONE', #24140 ) ;
#4936 = CARTESIAN_POINT ( 'NONE',  ( 116.8747167782375556, 0.000000000000000000, 1.849990392679523588 ) ) ;
#4937 = CARTESIAN_POINT ( 'NONE',  ( 142.1250000000000284, 0.000000000000000000, -6.000000000000005329 ) ) ;
#4938 = CARTESIAN_POINT ( 'NONE',  ( -3.608439182435115633, 6.249999999999965361, -105.9419872981078470 ) ) ;
#4939 = CARTESIAN_POINT ( 'NONE',  ( 138.8363248654052029, 0.000000000000000000, -5.500000000000005329 ) ) ;
#4940 = EDGE_CURVE ( 'NONE', #11050, #20611, #28306, .T. ) ;
#4941 = VECTOR ( 'NONE', #4855, 1000.000000000000000 ) ;
#4942 = CARTESIAN_POINT ( 'NONE',  ( 160.0163997308104342, 4.999999999999989342, 2.071067811865468400 ) ) ;
#4943 = CARTESIAN_POINT ( 'NONE',  ( 116.2499999999998437, 5.551115123125782702E-14, 2.500000000000168754 ) ) ;
#4944 = CARTESIAN_POINT ( 'NONE',  ( 6.350852961086080661, -9.614813431917819062E-14, -127.8749999999999858 ) ) ;
#4945 = ORIENTED_EDGE ( 'NONE', *, *, #7767, .T. ) ;
#4946 = CARTESIAN_POINT ( 'NONE',  ( 115.3988248654050182, -0.8284271247460852639, -1.999999999999791278 ) ) ;
#4947 = CARTESIAN_POINT ( 'NONE',  ( 4.763139720814407951, -2.749999999999988454, -66.50000000000000000 ) ) ;
#4948 = CARTESIAN_POINT ( 'NONE',  ( 6.000000000000052403, -1.607695154586662678, -81.15331216351296462 ) ) ;
#4949 = CARTESIAN_POINT ( 'NONE',  ( 109.2886751345947971, 2.000000000000057288, 1.110223024625156540E-13 ) ) ;
#4950 = CARTESIAN_POINT ( 'NONE',  ( 7.216878364870455975, -6.409875621278545621E-14, -81.80801270189226670 ) ) ;
#4951 = CARTESIAN_POINT ( 'NONE',  ( 6.000000000000000888, 7.762456499804234384E-14, -140.1636751345948255 ) ) ;
#4952 = CARTESIAN_POINT ( 'NONE',  ( 107.4372167782373850, 0.7662911109078287542, -1.849990392679351725 ) ) ;
#4953 = CARTESIAN_POINT ( 'NONE',  ( -5.999999999999963585, -2.788906526875773208E-15, -176.3363248654052029 ) ) ;
#4954 = COLOUR_RGB ( '', 0.09019608, 0.27058824, 0.51372549) ;
#4955 = CARTESIAN_POINT ( 'NONE',  ( -5.999999999999963585, 1.780251999655701777E-13, -94.41367513459482552 ) ) ;
#4956 = CARTESIAN_POINT ( 'NONE',  ( 113.6877832217621460, -0.7662911109077987781, 1.849990392679591977 ) ) ;
#4957 = CARTESIAN_POINT ( 'NONE',  ( -4.763139720814407951, -2.750000000000016431, -137.5000000000000000 ) ) ;
#4958 = CARTESIAN_POINT ( 'NONE',  ( 139.9157253400916829, -9.546725596017704873, 7.785029603303435408 ) ) ;
#4959 = CIRCLE ( 'NONE', #8913, 11.00000000000001599 ) ;
#4960 = CARTESIAN_POINT ( 'NONE',  ( 3.608439182435180470, -6.249999999999997335, -152.5580127018922099 ) ) ;
#4961 = DIRECTION ( 'NONE',  ( -6.938893903907222067E-15, 1.000000000000000000, 0.000000000000000000 ) ) ;
#4962 = CARTESIAN_POINT ( 'NONE',  ( 105.7113248654051461, 2.000000000000057288, 0.000000000000000000 ) ) ;
#4963 = ADVANCED_FACE ( 'NONE', ( #7845 ), #5237, .T. ) ;
#4964 = CARTESIAN_POINT ( 'NONE',  ( -3.175426480542816066, 5.499999999999865885, -79.37500000000002842 ) ) ;
#4965 = CARTESIAN_POINT ( 'NONE',  ( -5.196152422706601826, 2.999999999999975131, -114.0386751345948113 ) ) ;
#4966 = CARTESIAN_POINT ( 'NONE',  ( -2.775557561562891351E-14, -5.500000000000115463, -66.75000000000002842 ) ) ;
#4967 = CARTESIAN_POINT ( 'NONE',  ( 5.999999999999999112, 2.951592740943527306E-14, -155.1636751345948539 ) ) ;
#4968 = CARTESIAN_POINT ( 'NONE',  ( -3.464101615137757051, -5.999999999999979572, -148.1636751345947971 ) ) ;
#4969 = CARTESIAN_POINT ( 'NONE',  ( 160.3125000000000284, 4.242640687119298093, -4.242640687119298093 ) ) ;
#4970 = LINE ( 'NONE', #3259, #20236 ) ;
#4971 = CARTESIAN_POINT ( 'NONE',  ( 18.18750000000005684, 0.8284271247463557142, 1.999999999999971800 ) ) ;
#4972 = CARTESIAN_POINT ( 'NONE',  ( 0.000000000000000000, -5.999999999999991118, -49.96132486540522422 ) ) ;
#4973 = CARTESIAN_POINT ( 'NONE',  ( 115.8747167782375840, 0.000000000000000000, 1.849990392679523588 ) ) ;
#4974 = EDGE_CURVE ( 'NONE', #22535, #18178, #5514, .T. ) ;
#4975 = ORIENTED_EDGE ( 'NONE', *, *, #23661, .T. ) ;
#4976 = CARTESIAN_POINT ( 'NONE',  ( 151.6875000000000284, 4.242640687119269671, 4.242640687119298093 ) ) ;
#4977 = CARTESIAN_POINT ( 'NONE',  ( 119.1636751345946834, 1.414213562373145550, -1.414213562373145550 ) ) ;
#4978 = CARTESIAN_POINT ( 'NONE',  ( 115.0627832217623592, -0.7662911109076785410, -1.849990392679171425 ) ) ;
#4979 = AXIS2_PLACEMENT_3D ( 'NONE', #739, #14737, #16761 ) ;
#4980 = CARTESIAN_POINT ( 'NONE',  ( 140.5000000000000284, -10.00000000000000888, -7.500000000000007105 ) ) ;
#4981 =( BOUNDED_CURVE ( )  B_SPLINE_CURVE ( 2, ( #20451, #29810, #8788, #12187, #21373, #12032, #16492, #4614, #4910 ),
 .UNSPECIFIED., .F., .T. ) 
 B_SPLINE_CURVE_WITH_KNOTS ( ( 3, 2, 2, 2, 3 ),
 ( 0.05882352941176471894, 0.06617647058823528106, 0.07352941176470584317, 0.08088235294117651630, 0.08823529411764707842 ),
 .UNSPECIFIED. ) 
 CURVE ( )  GEOMETRIC_REPRESENTATION_ITEM ( )  RATIONAL_B_SPLINE_CURVE ( ( 1.000000000000000000, 0.9238795325112867385, 1.000000000000000000, 0.9238795325112867385, 1.000000000000000000, 0.9238795325112867385, 1.000000000000000000, 0.9238795325112867385, 1.000000000000000000 ) ) 
 REPRESENTATION_ITEM ( '' )  );
#4982 = CARTESIAN_POINT ( 'NONE',  ( 19.43750000000012790, -1.999999999999851674, 0.8284271247462354770 ) ) ;
#4983 = ORIENTED_EDGE ( 'NONE', *, *, #28715, .F. ) ;
#4984 = CARTESIAN_POINT ( 'NONE',  ( 3.608439182435180470, 6.249999999999982236, -152.6919872981078186 ) ) ;
#4985 = ORIENTED_EDGE ( 'NONE', *, *, #4286, .T. ) ;
#4986 = CARTESIAN_POINT ( 'NONE',  ( -4.763139720814407951, -2.750000000000016431, -88.00000000000002842 ) ) ;
#4987 = DIRECTION ( 'NONE',  ( -6.938893903907221278E-15, 1.000000000000000000, 0.000000000000000000 ) ) ;
#4988 = CARTESIAN_POINT ( 'NONE',  ( 153.7351497308104342, 3.535533905932725318, -3.535533905932725318 ) ) ;
#4989 = AXIS2_PLACEMENT_3D ( 'NONE', #29065, #3116, #2669 ) ;
#4990 = FACE_OUTER_BOUND ( 'NONE', #6258, .T. ) ;
#4991 = CARTESIAN_POINT ( 'NONE',  ( 1.960615434941584301, -10.82557180451506085, -19.32589338774632282 ) ) ;
#4992 = DIRECTION ( 'NONE',  ( -0.000000000000000000, 1.000000000000000000, -1.224646799147353207E-16 ) ) ;
#4993 = CARTESIAN_POINT ( 'NONE',  ( 3.175426480543072749, 5.499999999999865885, -166.6250000000000000 ) ) ;
#4994 = CARTESIAN_POINT ( 'NONE',  ( -5.999999999999919176, 1.607695154586804565, -57.90331216351300014 ) ) ;
#4995 = CARTESIAN_POINT ( 'NONE',  ( -4.763139720814407951, 2.749999999999946709, -152.7500000000000568 ) ) ;
#4996 = CARTESIAN_POINT ( 'NONE',  ( 112.1249999999998437, 1.767766952966293159, 1.767766952966431937 ) ) ;
#4997 = EDGE_CURVE ( 'NONE', #19034, #2328, #21363, .T. ) ;
#4998 = CARTESIAN_POINT ( 'NONE',  ( 3.175426480543072749, 5.499999999999865885, -103.6250000000000142 ) ) ;
#4999 = CARTESIAN_POINT ( 'NONE',  ( 6.000000000000000888, 1.743066579297358182E-13, -60.08632486540520290 ) ) ;
#5000 = EDGE_CURVE ( 'NONE', #11352, #25418, #8678, .T. ) ;
#5001 = CARTESIAN_POINT ( 'NONE',  ( 6.350852961086080661, -9.614813431917819062E-14, -85.87500000000005684 ) ) ;
#5002 = CARTESIAN_POINT ( 'NONE',  ( 109.5863248654051603, 1.414213562373201061, -1.414213562373145550 ) ) ;
#5003 = CARTESIAN_POINT ( 'NONE',  ( 9.625000000000106581, 2.649519052838444910, 0.000000000000000000 ) ) ;
#5004 = AXIS2_PLACEMENT_3D ( 'NONE', #3702, #27203, #10343 ) ;
#5005 = UNCERTAINTY_MEASURE_WITH_UNIT (LENGTH_MEASURE( 1.000000000000000082E-05 ), #1107, 'distance_accuracy_value', 'NONE');
#5006 = CARTESIAN_POINT ( 'NONE',  ( 113.5624999999997158, -2.499999999999964473, -1.035533905932689347 ) ) ;
#5007 = DIRECTION ( 'NONE',  ( -1.000000000000000000, -1.665334536937731113E-16, 1.526556658859586792E-16 ) ) ;
#5008 = CARTESIAN_POINT ( 'NONE',  ( 106.0627832217622455, -0.7662911109077388261, -1.849990392679351725 ) ) ;
#5009 = CARTESIAN_POINT ( 'NONE',  ( -5.196152422706601826, 2.999999999999975131, -78.03867513459483973 ) ) ;
#5010 = ORIENTED_EDGE ( 'NONE', *, *, #13796, .F. ) ;
#5011 = CARTESIAN_POINT ( 'NONE',  ( 0.000000000000000000, 10.49588505988223375, 0.000000000000000000 ) ) ;
#5012 = DIRECTION ( 'NONE',  ( -7.147005652999508048E-36, 5.642372883946980038E-36, 1.000000000000000000 ) ) ;
#5013 = CARTESIAN_POINT ( 'NONE',  ( 107.4997167782375982, 1.308140751793723799, -1.308140751793640533 ) ) ;
#5014 = ORIENTED_EDGE ( 'NONE', *, *, #9803, .F. ) ;
#5015 = EDGE_LOOP ( 'NONE', ( #8507, #27747, #5826, #6157 ) ) ;
#5016 = CARTESIAN_POINT ( 'NONE',  ( 0.000000000000000000, 5.499999999999991118, -113.9999999999999858 ) ) ;
#5017 = CARTESIAN_POINT ( 'NONE',  ( 17.50000000000012790, 1.873492889145011997, 1.873492889144734441 ) ) ;
#5018 = CARTESIAN_POINT ( 'NONE',  ( 2.775557561562891351E-14, -6.250000000000061284, -121.1830127018922383 ) ) ;
#5019 = UNCERTAINTY_MEASURE_WITH_UNIT (LENGTH_MEASURE( 1.000000000000000082E-05 ), #28319, 'distance_accuracy_value', 'NONE');
#5020 = ORIENTED_EDGE ( 'NONE', *, *, #14294, .T. ) ;
#5021 = CARTESIAN_POINT ( 'NONE',  ( 158.5238248654052313, 3.889087296526011706, -3.889087296526011706 ) ) ;
#5022 = CARTESIAN_POINT ( 'NONE',  ( 5.412658773652739619, 3.124999999999988898, -164.8169872981077901 ) ) ;
#5023 = CARTESIAN_POINT ( 'NONE',  ( 106.4374999999997442, -2.499999999999994671, 1.035533905932989551 ) ) ;
#5024 = CARTESIAN_POINT ( 'NONE',  ( 132.9226497308104058, 5.000000000000004441, 0.000000000000000000 ) ) ;
#5025 = ORIENTED_EDGE ( 'NONE', *, *, #262, .T. ) ;
#5026 = CARTESIAN_POINT ( 'NONE',  ( -4.509628467067655855, 10.03401783428613925, -21.03762154299059262 ) ) ;
#5027 = DIRECTION ( 'NONE',  ( -1.000000000000000000, 0.000000000000000000, 0.000000000000000000 ) ) ;
#5028 = CARTESIAN_POINT ( 'NONE',  ( -5.999999999999956479, -1.607695154586745057, -150.7693375672974412 ) ) ;
#5029 = CARTESIAN_POINT ( 'NONE',  ( 106.1877832217621318, 0.7662911109077987781, -1.849990392679351725 ) ) ;
#5030 = FACE_OUTER_BOUND ( 'NONE', #26849, .T. ) ;
#5031 = CARTESIAN_POINT ( 'NONE',  ( -5.412658773652739619, 3.124999999999975131, -180.1830127018922383 ) ) ;
#5032 = CARTESIAN_POINT ( 'NONE',  ( 0.000000000000000000, 5.999999999999977796, -76.21132486540521711 ) ) ;
#5033 = CARTESIAN_POINT ( 'NONE',  ( -5.999999999999963585, -1.487416814333745711E-14, -101.9136751345948397 ) ) ;
#5034 = CARTESIAN_POINT ( 'NONE',  ( -3.175426480542816066, -5.500000000000057732, -126.8749999999999858 ) ) ;
#5035 = CARTESIAN_POINT ( 'NONE',  ( 160.9323586472526699, -11.54909004507883452, -3.261009256920451627 ) ) ;
#5036 = UNCERTAINTY_MEASURE_WITH_UNIT (LENGTH_MEASURE( 1.000000000000000082E-05 ), #25270, 'distance_accuracy_value', 'NONE');
#5037 = ADVANCED_FACE ( 'NONE', ( #20154 ), #18122, .F. ) ;
#5038 = CARTESIAN_POINT ( 'NONE',  ( 3.175426480543072749, 5.499999999999865885, -111.1249999999999716 ) ) ;
#5039 = LINE ( 'NONE', #7060, #23990 ) ;
#5040 = CARTESIAN_POINT ( 'NONE',  ( -3.464101615137725076, 5.999999999999979572, -100.6636751345948113 ) ) ;
#5041 = ORIENTED_EDGE ( 'NONE', *, *, #15196, .F. ) ;
#5042 = DIRECTION ( 'NONE',  ( -7.147005652999508048E-36, 5.642372883946980038E-36, 1.000000000000000000 ) ) ;
#5043 = DIRECTION ( 'NONE',  ( 1.000000000000000000, 1.734723475976843579E-16, -0.000000000000000000 ) ) ;
#5044 = CARTESIAN_POINT ( 'NONE',  ( -5.999999999999962697, 3.323446944526963260E-14, -155.3363248654052313 ) ) ;
#5045 = AXIS2_PLACEMENT_3D ( 'NONE', #5602, #17937, #22528 ) ;
#5046 = ORIENTED_EDGE ( 'NONE', *, *, #22479, .T. ) ;
#5047 = CARTESIAN_POINT ( 'NONE',  ( 5.196152422706629359, -2.999999999999988898, -126.2113248654052029 ) ) ;
#5048 = LINE ( 'NONE', #2608, #19976 ) ;
#5049 = CARTESIAN_POINT ( 'NONE',  ( 110.3122167782374419, -0.7662911109077388261, -1.849990392679411677 ) ) ;
#5050 = CARTESIAN_POINT ( 'NONE',  ( 162.0000000000000284, 0.000000000000000000, 0.000000000000000000 ) ) ;
#5051 = VERTEX_POINT ( 'NONE', #8467 ) ;
#5052 = CARTESIAN_POINT ( 'NONE',  ( 157.1324251345948539, -5.500000000000012434, -2.278174593052012309 ) ) ;
#5053 = EDGE_LOOP ( 'NONE', ( #26689, #12890, #18667, #27412 ) ) ;
#5054 = ORIENTED_EDGE ( 'NONE', *, *, #3778, .T. ) ;
#5055 = CARTESIAN_POINT ( 'NONE',  ( 138.0000000000000284, 6.000000000000005329, 0.000000000000000000 ) ) ;
#5056 = CARTESIAN_POINT ( 'NONE',  ( 11.06250000000006928, 2.000000000000091926, 0.8284271247461753029 ) ) ;
#5057 = EDGE_LOOP ( 'NONE', ( #20908, #7809, #11425, #17225 ) ) ;
#5058 = CARTESIAN_POINT ( 'NONE',  ( 5.412658773652712085, -3.125000000000086153, -139.5669872981077901 ) ) ;
#5059 = CARTESIAN_POINT ( 'NONE',  ( 24.46132486540536632, 1.665334536937734811E-13, -2.500000000000002220 ) ) ;
#5060 = CARTESIAN_POINT ( 'NONE',  ( 10.31249999999998934, 2.649519052838478661, -1.097466725451679892 ) ) ;
#5061 = EDGE_CURVE ( 'NONE', #20652, #22535, #14798, .T. ) ;
#5062 = CYLINDRICAL_SURFACE ( 'NONE', #7389, 6.000000000000000888 ) ;
#5063 = EDGE_LOOP ( 'NONE', ( #5862, #29537, #1055, #3465 ) ) ;
#5064 = CARTESIAN_POINT ( 'NONE',  ( 19.50000000000009948, -1.999999999999835243, 0.000000000000000000 ) ) ;
#5065 = FACE_OUTER_BOUND ( 'NONE', #6997, .T. ) ;
#5066 = DIRECTION ( 'NONE',  ( 1.000000000000000000, 0.000000000000000000, 0.000000000000000000 ) ) ;
#5067 =( BOUNDED_CURVE ( )  B_SPLINE_CURVE ( 2, ( #28499, #7465, #21617, #16876, #26196, #10247, #22523, #27099, #29400 ),
 .UNSPECIFIED., .F., .T. ) 
 B_SPLINE_CURVE_WITH_KNOTS ( ( 3, 2, 2, 2, 3 ),
 ( 0.8906250000000000000, 0.8984375000000000000, 0.9062500000000000000, 0.9140625000000000000, 0.9194088329325865727 ),
 .UNSPECIFIED. ) 
 CURVE ( )  GEOMETRIC_REPRESENTATION_ITEM ( )  RATIONAL_B_SPLINE_CURVE ( ( 1.000000000000000000, 0.9238795325112867385, 1.000000000000000000, 0.9238795325112867385, 1.000000000000000000, 0.9238795325112867385, 1.000000000000000000, 0.9479084336411144340, 0.9671125746062680939 ) ) 
 REPRESENTATION_ITEM ( '' )  );
#5068 = CARTESIAN_POINT ( 'NONE',  ( -1.000000000000000888, -9.000000000000007105, 4.000000000000003553 ) ) ;
#5069 = CARTESIAN_POINT ( 'NONE',  ( 135.7351497308104058, 3.535533905932725318, -3.535533905932725318 ) ) ;
#5070 = DIRECTION ( 'NONE',  ( -7.147005652999508048E-36, 5.642372883946980038E-36, 1.000000000000000000 ) ) ;
#5071 =( NAMED_UNIT ( * ) PLANE_ANGLE_UNIT ( ) SI_UNIT ( $, .RADIAN. ) );
#5072 = CARTESIAN_POINT ( 'NONE',  ( 3.464101615137852974, 5.999999999999884537, -60.41367513459482552 ) ) ;
#5073 = CARTESIAN_POINT ( 'NONE',  ( -5.999999999999971578, 1.607695154586715303, -113.4033121635130072 ) ) ;
#5074 = CARTESIAN_POINT ( 'NONE',  ( 105.1874999999998437, 1.035533905932749299, 2.500000000000265121 ) ) ;
#5075 = EDGE_CURVE ( 'NONE', #19519, #28690, #24359, .T. ) ;
#5076 = EDGE_LOOP ( 'NONE', ( #27362, #17209, #7964, #7510 ) ) ;
#5077 = CARTESIAN_POINT ( 'NONE',  ( 4.763139720814407951, -2.749999999999988454, -48.49999999999998579 ) ) ;
#5078 = CARTESIAN_POINT ( 'NONE',  ( -4.999999999999990230, -24.99999999999999289, 5.000000000000004441 ) ) ;
#5079 = CARTESIAN_POINT ( 'NONE',  ( 0.000000000000000000, 0.000000000000000000, 0.000000000000000000 ) ) ;
#5080 = CARTESIAN_POINT ( 'NONE',  ( -5.999999999999962697, 3.323446944526963260E-14, -152.3363248654052313 ) ) ;
#5081 = EDGE_LOOP ( 'NONE', ( #25310, #17800, #17660, #8345 ) ) ;
#5082 = CARTESIAN_POINT ( 'NONE',  ( 115.8747167782375840, 0.000000000000000000, 1.849990392679523588 ) ) ;
#5083 = CARTESIAN_POINT ( 'NONE',  ( 3.608439182435180470, -6.249999999999997335, -106.6919872981078612 ) ) ;
#5084 = CARTESIAN_POINT ( 'NONE',  ( -5.196152422706601826, 2.999999999999975131, -172.5386751345947971 ) ) ;
#5085 = CARTESIAN_POINT ( 'NONE',  ( 133.3125000000000284, 4.242640687119298093, -4.242640687119298093 ) ) ;
#5086 = CARTESIAN_POINT ( 'NONE',  ( 118.6249999999998010, -1.767766952966431937, -1.767766952966209892 ) ) ;
#5087 = CARTESIAN_POINT ( 'NONE',  ( -3.175426480542816510, 5.499999999999865885, -130.3750000000000284 ) ) ;
#5088 = EDGE_CURVE ( 'NONE', #25453, #4865, #16960, .T. ) ;
#5089 = EDGE_LOOP ( 'NONE', ( #16116, #2289, #8621, #29497 ) ) ;
#5090 = B_SPLINE_CURVE_WITH_KNOTS ( 'NONE', 3,
 ( #26641, #15004, #7219, #10397 ),
 .UNSPECIFIED., .F., .F.,
 ( 4, 4 ),
 ( 0.000000000000000000, 0.0007771587456802753549 ),
 .UNSPECIFIED. ) ;
#5091 = CARTESIAN_POINT ( 'NONE',  ( -5.999999999999919176, 1.607695154586804565, -95.98066243270261566 ) ) ;
#5092 = EDGE_CURVE ( 'NONE', #13146, #6031, #27490, .T. ) ;
#5093 = CARTESIAN_POINT ( 'NONE',  ( -3.175426480542816510, -5.500000000000057732, -54.87500000000003553 ) ) ;
#5094 = CARTESIAN_POINT ( 'NONE',  ( 124.9999999999999432, -70.00000000000000000, 5.000000000000004441 ) ) ;
#5095 = CARTESIAN_POINT ( 'NONE',  ( 119.9999999999998721, -0.4876318259425804769, -1.939643060543838615 ) ) ;
#5096 = CARTESIAN_POINT ( 'NONE',  ( 5.412658773652739619, 3.124999999999988898, -81.68301270189226670 ) ) ;
#5097 = PRODUCT_DEFINITION_CONTEXT ( 'detailed design', #7328, 'design' ) ;
#5098 = LINE ( 'NONE', #14810, #86 ) ;
#5099 = CARTESIAN_POINT ( 'NONE',  ( -3.464101615137725076, 5.999999999999979572, -149.5863248654051176 ) ) ;
#5100 = CARTESIAN_POINT ( 'NONE',  ( 105.4372167782375413, 0.7662911109078888172, -1.849990392679291551 ) ) ;
#5101 = CARTESIAN_POINT ( 'NONE',  ( 3.464101615137757051, -5.999999999999979572, -175.8363248654052029 ) ) ;
#5102 = CARTESIAN_POINT ( 'NONE',  ( -5.999999999999963585, 1.780251999655701777E-13, -60.83632486540522422 ) ) ;
#5103 = CARTESIAN_POINT ( 'NONE',  ( 114.6877832217621318, -0.7662911109077987781, 1.849990392679591977 ) ) ;
#5104 = EDGE_CURVE ( 'NONE', #124, #18584, #19108, .T. ) ;
#5105 = CONTEXT_DEPENDENT_SHAPE_REPRESENTATION ( #11072, #25348 ) ;
#5106 = ADVANCED_FACE ( 'NONE', ( #4462 ), #14335, .T. ) ;
#5107 = CARTESIAN_POINT ( 'NONE',  ( -3.175426480542816066, 5.499999999999865885, -140.8750000000000568 ) ) ;
#5108 = CARTESIAN_POINT ( 'NONE',  ( 139.9892236744308889, -9.817200068377076150, 7.619547926460280785 ) ) ;
#5109 = CARTESIAN_POINT ( 'NONE',  ( 3.608439182435180470, 6.249999999999982236, -150.5580127018922667 ) ) ;
#5110 = CARTESIAN_POINT ( 'NONE',  ( 146.6175748654052313, 5.500000000000012434, -2.278174593052012309 ) ) ;
#5111 = CARTESIAN_POINT ( 'NONE',  ( 6.350852961086080661, -9.614813431917819062E-14, -70.87500000000004263 ) ) ;
#5112 = CARTESIAN_POINT ( 'NONE',  ( 145.5863248654052313, 0.000000000000000000, 5.500000000000005329 ) ) ;
#5113 = CARTESIAN_POINT ( 'NONE',  ( -3.175426480542816510, -5.500000000000057732, -65.37500000000001421 ) ) ;
#5114 = CARTESIAN_POINT ( 'NONE',  ( -5.196152422706601826, 2.999999999999975131, -53.46132486540522422 ) ) ;
#5115 = CARTESIAN_POINT ( 'NONE',  ( 144.6711002691896226, 4.999999999999989342, 2.071067811865468400 ) ) ;
#5116 = CARTESIAN_POINT ( 'NONE',  ( 108.2886751345946834, 2.000000000000057288, 2.220446049250313081E-13 ) ) ;
#5117 = CARTESIAN_POINT ( 'NONE',  ( 154.1250000000000284, 0.000000000000000000, -6.000000000000005329 ) ) ;
#5118 = CARTESIAN_POINT ( 'NONE',  ( 6.000000000000000888, 1.743066579297358182E-13, -98.16367513459481131 ) ) ;
#5119 = ORIENTED_EDGE ( 'NONE', *, *, #10938, .F. ) ;
#5120 = CARTESIAN_POINT ( 'NONE',  ( 149.8125000000000568, 4.242640687119298093, -4.242640687119298093 ) ) ;
#5121 = CARTESIAN_POINT ( 'NONE',  ( 112.6252832217622597, 1.665334536937734811E-13, 1.849990392679745632 ) ) ;
#5122 = VECTOR ( 'NONE', #14563, 1000.000000000000000 ) ;
#5123 = UNCERTAINTY_MEASURE_WITH_UNIT (LENGTH_MEASURE( 1.000000000000000082E-05 ), #21918, 'distance_accuracy_value', 'NONE');
#5124 = CARTESIAN_POINT ( 'NONE',  ( 104.7623688579944741, 1.279647136099528737, 1.365257574501548721 ) ) ;
#5125 = CARTESIAN_POINT ( 'NONE',  ( 7.216878364870455975, -6.409875621278545621E-14, -46.44198729810782567 ) ) ;
#5126 = CARTESIAN_POINT ( 'NONE',  ( 19.93750000000015277, 2.000000000000091926, -0.8284271247462354770 ) ) ;
#5127 = CARTESIAN_POINT ( 'NONE',  ( 7.216878364870455975, -6.409875621278545621E-14, -152.9419872981078186 ) ) ;
#5128 = ORIENTED_EDGE ( 'NONE', *, *, #17146, .T. ) ;
#5129 = ADVANCED_FACE ( 'NONE', ( #23525 ), #11883, .T. ) ;
#5130 = CARTESIAN_POINT ( 'NONE',  ( -4.763139720814407951, 2.749999999999946709, -82.25000000000004263 ) ) ;
#5131 =( GEOMETRIC_REPRESENTATION_CONTEXT ( 3 ) GLOBAL_UNCERTAINTY_ASSIGNED_CONTEXT ( ( #1314 ) ) GLOBAL_UNIT_ASSIGNED_CONTEXT ( ( #17406, #14508, #2786 ) ) REPRESENTATION_CONTEXT ( 'NONE', 'WORKASPACE' ) );
#5132 = CARTESIAN_POINT ( 'NONE',  ( -3.608439182435115633, 6.249999999999965361, -99.30801270189222407 ) ) ;
#5133 = ORIENTED_EDGE ( 'NONE', *, *, #12364, .F. ) ;
#5134 = AXIS2_PLACEMENT_3D ( 'NONE', #25665, #30118, #18476 ) ;
#5135 = SURFACE_SIDE_STYLE ('',( #16863 ) ) ;
#5136 = CARTESIAN_POINT ( 'NONE',  ( 110.8511751345946692, -1.999999999999911626, -0.8284271247459952248 ) ) ;
#5137 = DIRECTION ( 'NONE',  ( 1.000000000000000000, -5.551115123125773458E-17, -1.260129944081490338E-35 ) ) ;
#5138 = PLANE ( 'NONE',  #19141 ) ;
#5139 = DIRECTION ( 'NONE',  ( 1.000000000000000000, 1.067522139062651904E-16, -0.000000000000000000 ) ) ;
#5140 = EDGE_CURVE ( 'NONE', #8549, #7308, #23235, .T. ) ;
#5141 = EDGE_CURVE ( 'NONE', #6464, #6046, #26332, .T. ) ;
#5142 = CARTESIAN_POINT ( 'NONE',  ( 3.175426480543072749, -5.500000000000105693, -165.6250000000000000 ) ) ;
#5143 = CARTESIAN_POINT ( 'NONE',  ( 6.000000000000052403, -1.607695154586662678, -60.15331216351297883 ) ) ;
#5144 = CARTESIAN_POINT ( 'NONE',  ( -3.175426480542816510, 5.499999999999865885, -157.3750000000000000 ) ) ;
#5145 = CARTESIAN_POINT ( 'NONE',  ( 113.7499999999997584, 0.000000000000000000, -2.500000000000057732 ) ) ;
#5146 = AXIS2_PLACEMENT_3D ( 'NONE', #12244, #24427, #15248 ) ;
#5147 = CARTESIAN_POINT ( 'NONE',  ( -2.775557561562891351E-14, -5.500000000000115463, -92.25000000000000000 ) ) ;
#5148 = DIRECTION ( 'NONE',  ( -2.498001805406611091E-16, 8.049116928532385904E-16, -1.000000000000000000 ) ) ;
#5149 =( BOUNDED_CURVE ( )  B_SPLINE_CURVE ( 2, ( #17326, #19905, #26642, #3299, #15007, #24346, #10400, #19752, #15163 ),
 .UNSPECIFIED., .F., .F. ) 
 B_SPLINE_CURVE_WITH_KNOTS ( ( 3, 2, 2, 2, 3 ),
 ( 0.6083333333333333925, 0.6092592592592592782, 0.6111111111111111605, 0.6129629629629629317, 0.6138888888888889284 ),
 .UNSPECIFIED. ) 
 CURVE ( )  GEOMETRIC_REPRESENTATION_ITEM ( )  RATIONAL_B_SPLINE_CURVE ( ( 0.9330127018922194093, 0.9330127018922234061, 1.000000000000000000, 0.8660254037844388186, 1.000000000000000000, 0.8660254037844388186, 1.000000000000000000, 0.9330127018922154125, 0.9330127018922194093 ) ) 
 REPRESENTATION_ITEM ( '' )  );
#5150 = CARTESIAN_POINT ( 'NONE',  ( 6.350852961086080661, -9.614813431917819062E-14, -91.87500000000001421 ) ) ;
#5151 = CARTESIAN_POINT ( 'NONE',  ( 154.9836002691896510, 4.999999999999989342, -2.071067811865468400 ) ) ;
#5152 = CARTESIAN_POINT ( 'NONE',  ( 109.4613248654051745, 0.000000000000000000, -2.000000000000001776 ) ) ;
#5153 = CARTESIAN_POINT ( 'NONE',  ( 23.81250000000003553, 0.8284271247463557142, -2.000000000000151879 ) ) ;
#5154 = CARTESIAN_POINT ( 'NONE',  ( 113.7499999999997584, 0.000000000000000000, -2.500000000000057732 ) ) ;
#5155 = DIRECTION ( 'NONE',  ( 1.000000000000000000, -3.469446951953694061E-16, -0.000000000000000000 ) ) ;
#5156 = CARTESIAN_POINT ( 'NONE',  ( 6.000000000000000888, 1.743066579297358182E-13, -73.58632486540520290 ) ) ;
#5157 = DIRECTION ( 'NONE',  ( 0.000000000000000000, 0.8907235428302470170, 0.4545454545454539197 ) ) ;
#5158 =( BOUNDED_CURVE ( )  B_SPLINE_CURVE ( 2, ( #1352, #10764, #20109, #29453, #17832, #1503, #6267, #5305, #404 ),
 .UNSPECIFIED., .F., .T. ) 
 B_SPLINE_CURVE_WITH_KNOTS ( ( 3, 2, 2, 2, 3 ),
 ( 0.3874999999999999001, 0.3937500000000000999, 0.4000000000000003553, 0.4062500000000006106, 0.4125000000000008105 ),
 .UNSPECIFIED. ) 
 CURVE ( )  GEOMETRIC_REPRESENTATION_ITEM ( )  RATIONAL_B_SPLINE_CURVE ( ( 1.000000000000001332, 0.9238795325112854062, 1.000000000000000000, 0.9238795325112867385, 1.000000000000000000, 0.9238795325112867385, 1.000000000000000000, 0.9238795325112766355, 1.000000000000010214 ) ) 
 REPRESENTATION_ITEM ( '' )  );
#5159 = ORIENTED_EDGE ( 'NONE', *, *, #20144, .F. ) ;
#5160 = AXIS2_PLACEMENT_3D ( 'NONE', #17672, #19800, #5959 ) ;
#5161 = DIRECTION ( 'NONE',  ( 1.000000000000000000, -5.551115123125773458E-17, -1.260129944081490338E-35 ) ) ;
#5162 = CARTESIAN_POINT ( 'NONE',  ( 119.3127832217621034, 1.849990392679501827, -0.7662911109077087390 ) ) ;
#5163 = ORIENTED_EDGE ( 'NONE', *, *, #12036, .T. ) ;
#5164 = VERTEX_POINT ( 'NONE', #9229 ) ;
#5165 = EDGE_LOOP ( 'NONE', ( #20714, #9221, #6377, #25340 ) ) ;
#5166 = VECTOR ( 'NONE', #3445, 1000.000000000000000 ) ;
#5167 = ADVANCED_FACE ( 'NONE', ( #18620, #6915 ), #27942, .T. ) ;
#5168 = CARTESIAN_POINT ( 'NONE',  ( -4.763139720814407951, -2.750000000000016431, -108.9999999999999858 ) ) ;
#5169 = CARTESIAN_POINT ( 'NONE',  ( 19.43750000000013145, 2.649519052838358757, 1.097466725451499370 ) ) ;
#5170 = CARTESIAN_POINT ( 'NONE',  ( 2.775557561562891351E-14, -6.250000000000061284, -125.6830127018922525 ) ) ;
#5171 = ORIENTED_EDGE ( 'NONE', *, *, #5691, .F. ) ;
#5172 = CARTESIAN_POINT ( 'NONE',  ( -5.196152422706573404, -3.000000000000002665, -110.7886751345948397 ) ) ;
#5173 = CARTESIAN_POINT ( 'NONE',  ( -3.608439182435115633, 6.249999999999965361, -162.9419872981077901 ) ) ;
#5174 = CARTESIAN_POINT ( 'NONE',  ( 109.9999999999999432, 2.500000000000030198, 0.000000000000000000 ) ) ;
#5175 = CARTESIAN_POINT ( 'NONE',  ( 133.5788997308104058, -4.999999999999989342, 2.071067811865468400 ) ) ;
#5176 = CARTESIAN_POINT ( 'NONE',  ( 3.608439182435180470, -6.249999999999997335, -61.05801270189223828 ) ) ;
#5177 = ORIENTED_EDGE ( 'NONE', *, *, #26758, .F. ) ;
#5178 = CARTESIAN_POINT ( 'NONE',  ( 5.196152422706629359, 3.000000000000002665, -167.9613248654052029 ) ) ;
#5179 = ADVANCED_FACE ( 'NONE', ( #7660 ), #26363, .T. ) ;
#5180 = CARTESIAN_POINT ( 'NONE',  ( -0.7970850910874407447, 10.97816267869983875, -19.03975521967168660 ) ) ;
#5181 = DIRECTION ( 'NONE',  ( 1.000000000000000000, 0.000000000000000000, 0.000000000000000000 ) ) ;
#5182 = CARTESIAN_POINT ( 'NONE',  ( -3.175426480542816510, 5.499999999999865885, -175.3750000000000568 ) ) ;
#5183 = CARTESIAN_POINT ( 'NONE',  ( 108.9377832217621886, -1.849990392679411677, -0.7662911109076485650 ) ) ;
#5184 = MECHANICAL_DESIGN_GEOMETRIC_PRESENTATION_REPRESENTATION (  '', ( #12109 ), #6187 ) ;
#5185 = CARTESIAN_POINT ( 'NONE',  ( -3.464101615137725076, 5.999999999999979572, -100.0863248654052029 ) ) ;
#5186 = CARTESIAN_POINT ( 'NONE',  ( 2.775557561562891351E-14, 6.250000000000033751, -180.4330127018922667 ) ) ;
#5187 = CARTESIAN_POINT ( 'NONE',  ( 119.4761751345946834, 0.8284271247463257382, 2.000000000000212275 ) ) ;
#5188 = DIRECTION ( 'NONE',  ( 0.000000000000000000, 0.000000000000000000, 1.000000000000000000 ) ) ;
#5189 = CARTESIAN_POINT ( 'NONE',  ( 4.763139720814407951, -2.749999999999988454, -126.5000000000000568 ) ) ;
#5190 = CARTESIAN_POINT ( 'NONE',  ( 135.0000000000000568, -7.170799408905232042, 8.464366752364069768 ) ) ;
#5191 = CARTESIAN_POINT ( 'NONE',  ( 4.763139720814407951, 2.750000000000002665, -109.7500000000000142 ) ) ;
#5192 =( NAMED_UNIT ( * ) PLANE_ANGLE_UNIT ( ) SI_UNIT ( $, .RADIAN. ) );
#5193 = CARTESIAN_POINT ( 'NONE',  ( 16.14882486540525619, -2.499999999999904521, 1.035533905932749299 ) ) ;
#5194 = CARTESIAN_POINT ( 'NONE',  ( 148.5074251345948539, 2.278174593052012309, -5.500000000000012434 ) ) ;
#5195 = VERTEX_POINT ( 'NONE', #12473 ) ;
#5196 = AXIS2_PLACEMENT_3D ( 'NONE', #2001, #18314, #4450 ) ;
#5197 = CARTESIAN_POINT ( 'NONE',  ( -19.49999999999998224, -54.99999999999992184, 8.000000000000007105 ) ) ;
#5198 = CARTESIAN_POINT ( 'NONE',  ( -5.999999999999963585, -1.487416814333745711E-14, -137.3363248654052313 ) ) ;
#5199 = ORIENTED_EDGE ( 'NONE', *, *, #6999, .F. ) ;
#5200 = CARTESIAN_POINT ( 'NONE',  ( -3.464101615137757051, -5.999999999999979572, -126.5863248654051887 ) ) ;
#5201 = CARTESIAN_POINT ( 'NONE',  ( 3.175426480543072749, 5.499999999999865885, -177.1250000000000284 ) ) ;
#5202 = EDGE_LOOP ( 'NONE', ( #5010, #27511, #10723, #12735 ) ) ;
#5203 = DIRECTION ( 'NONE',  ( 1.000000000000000000, -5.551115123125773458E-17, -1.260129944081490338E-35 ) ) ;
#5204 = ORIENTED_EDGE ( 'NONE', *, *, #30306, .F. ) ;
#5205 = ORIENTED_EDGE ( 'NONE', *, *, #29025, .T. ) ;
#5206 = CARTESIAN_POINT ( 'NONE',  ( 132.0000000000000284, 6.000000000000005329, 0.000000000000000000 ) ) ;
#5207 = CARTESIAN_POINT ( 'NONE',  ( 133.1398502691896510, -3.535533905932752852, 3.535533905932725318 ) ) ;
#5208 = ADVANCED_FACE ( 'NONE', ( #9693 ), #28994, .T. ) ;
#5209 = EDGE_CURVE ( 'NONE', #1357, #18127, #10298, .T. ) ;
#5210 = EDGE_LOOP ( 'NONE', ( #11504, #24612, #26838, #16787 ) ) ;
#5211 = CARTESIAN_POINT ( 'NONE',  ( -3.608439182435052128, -6.250000000000110134, -127.9419872981078186 ) ) ;
#5212 = CARTESIAN_POINT ( 'NONE',  ( 24.27382486540532369, -2.499999999999904521, -1.035533905932809473 ) ) ;
#5213 = CARTESIAN_POINT ( 'NONE',  ( 12.25000000000009415, 1.873492889145123019, -1.873492889144956486 ) ) ;
#5214 = CARTESIAN_POINT ( 'NONE',  ( -5.999999999999963585, -1.487416814333745711E-14, -128.9136751345948539 ) ) ;
#5215 = ORIENTED_EDGE ( 'NONE', *, *, #3431, .T. ) ;
#5216 = CARTESIAN_POINT ( 'NONE',  ( 20.68750000000011369, -0.8284271247459952248, -1.999999999999971800 ) ) ;
#5217 = DIRECTION ( 'NONE',  ( -7.147005652999508048E-36, 5.642372883946980038E-36, 1.000000000000000000 ) ) ;
#5218 = DIRECTION ( 'NONE',  ( -0.7071067811865455743, -1.324765512014429388E-16, 0.7071067811865495711 ) ) ;
#5219 = CARTESIAN_POINT ( 'NONE',  ( 137.4226497308104058, 5.000000000000004441, 0.000000000000000000 ) ) ;
#5220 = CARTESIAN_POINT ( 'NONE',  ( 6.000000000000000888, 1.743066579297358182E-13, -99.08632486540518869 ) ) ;
#5221 = CARTESIAN_POINT ( 'NONE',  ( -4.999999999999879208, -14.50000000000001243, -8.000000000000007105 ) ) ;
#5222 = CARTESIAN_POINT ( 'NONE',  ( 2.081668171172167281E-16, 3.582034040661430693E-16, -2.499999999999999112 ) ) ;
#5223 = CARTESIAN_POINT ( 'NONE',  ( 108.7738248654050182, 2.000000000000031530, 0.8284271247463557142 ) ) ;
#5224 = CARTESIAN_POINT ( 'NONE',  ( 104.4999999999998863, -2.499999999999919176, 0.000000000000000000 ) ) ;
#5225 = CARTESIAN_POINT ( 'NONE',  ( -3.464101615137757051, -5.999999999999979572, -143.0863248654052029 ) ) ;
#5226 = CARTESIAN_POINT ( 'NONE',  ( -3.175426480542816510, 5.499999999999865885, -140.8750000000000568 ) ) ;
#5227 = AXIS2_PLACEMENT_3D ( 'NONE', #7110, #9887, #19261 ) ;
#5228 = EDGE_LOOP ( 'NONE', ( #18941, #4407, #23790, #4382 ) ) ;
#5229 = CARTESIAN_POINT ( 'NONE',  ( -3.175426480542816066, 5.499999999999865885, -50.87500000000001421 ) ) ;
#5230 = CARTESIAN_POINT ( 'NONE',  ( 0.000000000000000000, -5.999999999999991118, -133.0386751345948824 ) ) ;
#5231 = CARTESIAN_POINT ( 'NONE',  ( 3.464101615137757051, -5.999999999999979572, -99.91367513459481131 ) ) ;
#5232 = ORIENTED_EDGE ( 'NONE', *, *, #25362, .T. ) ;
#5233 = CARTESIAN_POINT ( 'NONE',  ( 117.3122167782375840, -0.7662911109077388261, -1.849990392679351725 ) ) ;
#5234 = CARTESIAN_POINT ( 'NONE',  ( -6.000000000000000888, 1.067854986875958443E-15, 7.560779664488942560E-35 ) ) ;
#5235 = CARTESIAN_POINT ( 'NONE',  ( 11.68750000000000000, -0.8284271247461753029, -1.999999999999971800 ) ) ;
#5236 = CARTESIAN_POINT ( 'NONE',  ( 2.775557561562891351E-14, 6.250000000000033751, -92.56698729810780435 ) ) ;
#5237 = CYLINDRICAL_SURFACE ( 'NONE', #4795, 6.000000000000000888 ) ;
#5238 = CARTESIAN_POINT ( 'NONE',  ( 11.33632486540525619, -1.767766952966209892, -1.767766952966598470 ) ) ;
#5239 = CARTESIAN_POINT ( 'NONE',  ( 119.4374999999997868, -2.499999999999994671, 1.035533905932809473 ) ) ;
#5240 = VECTOR ( 'NONE', #5506, 1000.000000000000000 ) ;
#5241 = CARTESIAN_POINT ( 'NONE',  ( 140.2902754521815325, -11.64513772609109132, 4.288736938852949265 ) ) ;
#5242 = AXIS2_PLACEMENT_3D ( 'NONE', #20334, #12996, #17747 ) ;
#5243 = AXIS2_PLACEMENT_3D ( 'NONE', #9721, #19100, #477 ) ;
#5244 = CARTESIAN_POINT ( 'NONE',  ( -2.775557561562891351E-14, -5.500000000000115463, -128.2500000000000284 ) ) ;
#5245 =( BOUNDED_CURVE ( )  B_SPLINE_CURVE ( 2, ( #28421, #7537, #2193, #18648, #27966, #6942, #9563, #16361, #16659 ),
 .UNSPECIFIED., .F., .T. ) 
 B_SPLINE_CURVE_WITH_KNOTS ( ( 3, 2, 2, 2, 3 ),
 ( 0.5882352941176470784, 0.5955882352941176405, 0.6029411764705882026, 0.6102941176470588758, 0.6176470588235294379 ),
 .UNSPECIFIED. ) 
 CURVE ( )  GEOMETRIC_REPRESENTATION_ITEM ( )  RATIONAL_B_SPLINE_CURVE ( ( 1.000000000000000000, 0.9238795325112867385, 1.000000000000000000, 0.9238795325112867385, 1.000000000000000000, 0.9238795325112867385, 1.000000000000000000, 0.9238795325112867385, 1.000000000000000000 ) ) 
 REPRESENTATION_ITEM ( '' )  );
#5246 = EDGE_CURVE ( 'NONE', #5319, #13146, #14622, .T. ) ;
#5247 = ORIENTED_EDGE ( 'NONE', *, *, #21909, .F. ) ;
#5248 = CARTESIAN_POINT ( 'NONE',  ( 115.2113248654050750, -1.999999999999918510, 1.110223024625156540E-13 ) ) ;
#5249 = CARTESIAN_POINT ( 'NONE',  ( -4.763139720814407951, 2.749999999999946709, -59.75000000000002842 ) ) ;
#5250 = CYLINDRICAL_SURFACE ( 'NONE', #14128, 6.000000000000000888 ) ;
#5251 = CARTESIAN_POINT ( 'NONE',  ( 109.0386751345947118, 0.000000000000000000, -2.000000000000001776 ) ) ;
#5252 = CARTESIAN_POINT ( 'NONE',  ( 2.775557561562891351E-14, 10.99999999999998224, -31.00000000000002842 ) ) ;
#5253 = CARTESIAN_POINT ( 'NONE',  ( 3.608439182435180470, -6.249999999999997335, -82.05801270189219565 ) ) ;
#5254 = DIRECTION ( 'NONE',  ( -6.938893903907222067E-15, 1.000000000000000000, 0.000000000000000000 ) ) ;
#5255 = LINE ( 'NONE', #14663, #12851 ) ;
#5256 = CARTESIAN_POINT ( 'NONE',  ( 160.0000000000000284, -59.99999999999980105, -3.000000000000002665 ) ) ;
#5257 = CARTESIAN_POINT ( 'NONE',  ( 141.0000000000000284, -12.00000000000001066, -4.000000000000003553 ) ) ;
#5258 = DIRECTION ( 'NONE',  ( 0.000000000000000000, 0.000000000000000000, -1.000000000000000000 ) ) ;
#5259 = CARTESIAN_POINT ( 'NONE',  ( 113.3752832217622881, 1.849990392679523588, 0.000000000000000000 ) ) ;
#5260 = CARTESIAN_POINT ( 'NONE',  ( -6.350852961085760029, -1.281975124255709124E-13, -143.6250000000000000 ) ) ;
#5261 = CARTESIAN_POINT ( 'NONE',  ( -1.000000000000000888, 9.000000000000007105, 3.000000000000002665 ) ) ;
#5262 = CARTESIAN_POINT ( 'NONE',  ( 0.000000000000000000, -5.999999999999991118, -70.96132486540524553 ) ) ;
#5263 = CARTESIAN_POINT ( 'NONE',  ( 6.000000000000000888, -1.859271017917181981E-14, -72.66367513459483973 ) ) ;
#5264 = CARTESIAN_POINT ( 'NONE',  ( 4.763139720814407951, -2.749999999999988454, -71.00000000000001421 ) ) ;
#5265 = PRESENTATION_LAYER_ASSIGNMENT (  '', '', ( #29812 ) ) ;
#5266 = CARTESIAN_POINT ( 'NONE',  ( 144.8363248654052029, 0.000000000000000000, -5.500000000000005329 ) ) ;
#5267 = CARTESIAN_POINT ( 'NONE',  ( 6.350852961086080661, -9.614813431917819062E-14, -66.37500000000004263 ) ) ;
#5268 = SURFACE_STYLE_FILL_AREA ( #28758 ) ;
#5269 = CARTESIAN_POINT ( 'NONE',  ( 150.5625000000000568, -4.242640687119298093, 4.242640687119298093 ) ) ;
#5270 = CARTESIAN_POINT ( 'NONE',  ( 135.0000000000000284, -8.851546142247588733, -7.500000000000097700 ) ) ;
#5271 = EDGE_CURVE ( 'NONE', #15734, #30347, #3950, .T. ) ;
#5272 = CARTESIAN_POINT ( 'NONE',  ( 0.000000000000000000, -5.999999999999991118, -104.5386751345948113 ) ) ;
#5273 = CARTESIAN_POINT ( 'NONE',  ( 114.9997167782375698, -1.308140751793612777, 1.308140751793862577 ) ) ;
#5274 = FACE_OUTER_BOUND ( 'NONE', #22874, .T. ) ;
#5275 = ORIENTED_EDGE ( 'NONE', *, *, #9213, .T. ) ;
#5276 = CARTESIAN_POINT ( 'NONE',  ( 148.0312500000000284, -2.485281374238555774, -6.000000000000005329 ) ) ;
#5277 = AXIS2_PLACEMENT_3D ( 'NONE', #28209, #7185, #21030 ) ;
#5278 = CARTESIAN_POINT ( 'NONE',  ( -5.196152422706573404, -3.000000000000002665, -102.7113248654052455 ) ) ;
#5279 = EDGE_CURVE ( 'NONE', #18627, #20260, #16968, .T. ) ;
#5280 = CARTESIAN_POINT ( 'NONE',  ( 2.775557561562891351E-14, -6.250000000000061284, -46.81698729810779014 ) ) ;
#5281 = CARTESIAN_POINT ( 'NONE',  ( 22.18750000000018119, 0.8284271247464157772, 1.999999999999971800 ) ) ;
#5282 = VERTEX_POINT ( 'NONE', #20268 ) ;
#5283 = ORIENTED_EDGE ( 'NONE', *, *, #22117, .T. ) ;
#5284 = CARTESIAN_POINT ( 'NONE',  ( 0.000000000000000000, 5.499999999999991118, -84.00000000000001421 ) ) ;
#5285 = CARTESIAN_POINT ( 'NONE',  ( 120.0000000000000568, 1.621546429797428024, 1.617766924401469186 ) ) ;
#5286 = CARTESIAN_POINT ( 'NONE',  ( 6.000000000000000888, -1.859271017917181981E-14, -54.66367513459481842 ) ) ;
#5287 = CYLINDRICAL_SURFACE ( 'NONE', #27320, 6.000000000000000888 ) ;
#5288 = CARTESIAN_POINT ( 'NONE',  ( 140.0252556714799823, -11.51262782845654620, 4.739386388448187937 ) ) ;
#5289 = CARTESIAN_POINT ( 'NONE',  ( -3.175426480542816066, -5.500000000000057732, -161.3750000000000284 ) ) ;
#5290 = CARTESIAN_POINT ( 'NONE',  ( 160.6011751345948255, 3.889087296526011706, -3.889087296526011706 ) ) ;
#5291 = CARTESIAN_POINT ( 'NONE',  ( -4.763139720814407951, 2.749999999999946709, -158.7500000000000568 ) ) ;
#5292 = CARTESIAN_POINT ( 'NONE',  ( 117.2261751345945697, 2.000000000000061728, -0.8284271247459952248 ) ) ;
#5293 = CARTESIAN_POINT ( 'NONE',  ( -4.763139720814407951, 2.749999999999946709, -94.25000000000000000 ) ) ;
#5294 = CARTESIAN_POINT ( 'NONE',  ( 142.0238248654052029, 3.889087296526011706, -3.889087296526011706 ) ) ;
#5295 = DIRECTION ( 'NONE',  ( 1.000000000000000000, 0.000000000000000000, -0.000000000000000000 ) ) ;
#5296 = CARTESIAN_POINT ( 'NONE',  ( -4.763139720814407951, 2.749999999999946709, -91.25000000000005684 ) ) ;
#5297 = CYLINDRICAL_SURFACE ( 'NONE', #576, 2.499999999999999112 ) ;
#5298 = CARTESIAN_POINT ( 'NONE',  ( 155.8273502691896510, -5.000000000000004441, 0.000000000000000000 ) ) ;
#5299 = CARTESIAN_POINT ( 'NONE',  ( 3.464101615137852974, 5.999999999999884537, -64.91367513459485394 ) ) ;
#5300 = CARTESIAN_POINT ( 'NONE',  ( 5.196152422706629359, -2.999999999999988898, -135.7886751345947971 ) ) ;
#5301 = CARTESIAN_POINT ( 'NONE',  ( 22.81250000000002132, 0.8284271247461753029, -2.000000000000091926 ) ) ;
#5302 = CARTESIAN_POINT ( 'NONE',  ( 109.9374999999996874, 2.500000000000114575, -1.035533905932448873 ) ) ;
#5303 = EDGE_CURVE ( 'NONE', #13381, #8715, #13292, .T. ) ;
#5304 = CARTESIAN_POINT ( 'NONE',  ( 0.000000000000000000, 5.999999999999977796, -126.2886751345948539 ) ) ;
#5305 = CARTESIAN_POINT ( 'NONE',  ( 149.4300748654051745, 2.278174593051780050, -5.500000000000244249 ) ) ;
#5306 = DIRECTION ( 'NONE',  ( 1.000000000000000000, -5.551115123125773458E-17, -1.260129944081490338E-35 ) ) ;
#5307 = ORIENTED_EDGE ( 'NONE', *, *, #25279, .F. ) ;
#5308 = CYLINDRICAL_SURFACE ( 'NONE', #16302, 6.000000000000000888 ) ;
#5309 = CARTESIAN_POINT ( 'NONE',  ( 104.9997167782376692, -1.308140751793585022, 1.308140751793640533 ) ) ;
#5310 = EDGE_LOOP ( 'NONE', ( #3915, #25629, #24549, #13091 ) ) ;
#5311 = EDGE_CURVE ( 'NONE', #651, #1699, #27943, .T. ) ;
#5312 = EDGE_CURVE ( 'NONE', #25253, #29814, #22573, .T. ) ;
#5313 = VERTEX_POINT ( 'NONE', #20403 ) ;
#5314 = CARTESIAN_POINT ( 'NONE',  ( 147.0937500000000284, 6.000000000000005329, 2.485281374238585972 ) ) ;
#5315 = ORIENTED_EDGE ( 'NONE', *, *, #26063, .T. ) ;
#5316 = CARTESIAN_POINT ( 'NONE',  ( -4.763139720814407951, -2.750000000000016431, -104.5000000000000426 ) ) ;
#5317 = CARTESIAN_POINT ( 'NONE',  ( 18.06250000000005684, -1.097466725451379244, -2.649519052838419153 ) ) ;
#5318 = CARTESIAN_POINT ( 'NONE',  ( 2.775557561562891351E-14, -6.250000000000061284, -119.6830127018922383 ) ) ;
#5319 = VERTEX_POINT ( 'NONE', #8575 ) ;
#5320 = CARTESIAN_POINT ( 'NONE',  ( -6.000000000000007105, -1.607695154586655129, -110.8466878364870354 ) ) ;
#5321 = CARTESIAN_POINT ( 'NONE',  ( 5.412658773652712085, -3.125000000000086153, -157.5669872981078186 ) ) ;
#5322 = CARTESIAN_POINT ( 'NONE',  ( 132.4538997308104342, -2.071067811865468400, -4.999999999999989342 ) ) ;
#5323 = CARTESIAN_POINT ( 'NONE',  ( -7.216878364870328078, 0.000000000000000000, -61.55801270189223828 ) ) ;
#5324 = VERTEX_POINT ( 'NONE', #24996 ) ;
#5325 =( BOUNDED_CURVE ( )  B_SPLINE_CURVE ( 2, ( #7692, #5832, #15247, #636, #24579, #5231, #3528, #12958, #17252 ),
 .UNSPECIFIED., .F., .F. ) 
 B_SPLINE_CURVE_WITH_KNOTS ( ( 3, 2, 2, 2, 3 ),
 ( 0.6027777777777777457, 0.6037037037037037424, 0.6055555555555555136, 0.6074074074074073959, 0.6083333333333333925 ),
 .UNSPECIFIED. ) 
 CURVE ( )  GEOMETRIC_REPRESENTATION_ITEM ( )  RATIONAL_B_SPLINE_CURVE ( ( 0.9330127018922194093, 0.9330127018922154125, 1.000000000000000000, 0.8660254037844388186, 1.000000000000000000, 0.8660254037844388186, 1.000000000000000000, 0.9330127018922154125, 0.9330127018922194093 ) ) 
 REPRESENTATION_ITEM ( '' )  );
#5326 = CARTESIAN_POINT ( 'NONE',  ( 158.6324251345948824, -5.500000000000012434, -2.278174593052012309 ) ) ;
#5327 = CARTESIAN_POINT ( 'NONE',  ( -3.464101615137725076, 5.999999999999979572, -137.5863248654051745 ) ) ;
#5328 = CYLINDRICAL_SURFACE ( 'NONE', #28775, 6.000000000000000888 ) ;
#5329 = CARTESIAN_POINT ( 'NONE',  ( 120.4374999999997442, -2.499999999999964473, 1.035533905932989551 ) ) ;
#5330 = CARTESIAN_POINT ( 'NONE',  ( -0.08337014915864793263, -15.22335576789224199, 7.695802404352960480 ) ) ;
#5331 = CARTESIAN_POINT ( 'NONE',  ( 7.216878364870455975, -6.409875621278545621E-14, -168.8080127018922099 ) ) ;
#5332 = CARTESIAN_POINT ( 'NONE',  ( 113.2886751345947118, 1.999999999999946265, 1.110223024625156540E-13 ) ) ;
#5333 = CARTESIAN_POINT ( 'NONE',  ( 23.62500000000000711, -1.414213562372923505, -1.414213562373145550 ) ) ;
#5334 = CARTESIAN_POINT ( 'NONE',  ( 0.000000000000000000, 5.499999999999991118, -117.0000000000000000 ) ) ;
#5335 = LINE ( 'NONE', #5485, #3091 ) ;
#5336 = CARTESIAN_POINT ( 'NONE',  ( -3.175426480542816510, -5.500000000000057732, -116.3750000000000142 ) ) ;
#5337 =( BOUNDED_CURVE ( )  B_SPLINE_CURVE ( 2, ( #25876, #18694, #4830, #2386, #27867 ),
 .UNSPECIFIED., .F., .T. ) 
 B_SPLINE_CURVE_WITH_KNOTS ( ( 3, 2, 3 ),
 ( 0.8823529411764705621, 0.8897058823529411242, 0.8947377251129212672 ),
 .UNSPECIFIED. ) 
 CURVE ( )  GEOMETRIC_REPRESENTATION_ITEM ( )  RATIONAL_B_SPLINE_CURVE ( ( 1.000000000000000000, 0.9238795325112867385, 1.000000000000000000, 0.9479084336421641499, 0.9671125746054942685 ) ) 
 REPRESENTATION_ITEM ( '' )  );
#5338 = FILL_AREA_STYLE ('',( #10752 ) ) ;
#5339 = CARTESIAN_POINT ( 'NONE',  ( 0.000000000000000000, 0.000000000000000000, 0.000000000000000000 ) ) ;
#5340 = CARTESIAN_POINT ( 'NONE',  ( 6.000000000000000888, 1.743066579297358182E-13, -112.5863248654052029 ) ) ;
#5341 = ORIENTED_EDGE ( 'NONE', *, *, #19889, .F. ) ;
#5342 = CARTESIAN_POINT ( 'NONE',  ( 17.31250000000010303, -1.097466725451439196, -2.649519052838358757 ) ) ;
#5343 = CYLINDRICAL_SURFACE ( 'NONE', #2053, 12.00000000000000178 ) ;
#5344 = EDGE_CURVE ( 'NONE', #13277, #21900, #29302, .T. ) ;
#5345 = CARTESIAN_POINT ( 'NONE',  ( -3.464101615137725076, 5.999999999999979572, -109.0863248654051745 ) ) ;
#5346 = ORIENTED_EDGE ( 'NONE', *, *, #28734, .F. ) ;
#5347 = CARTESIAN_POINT ( 'NONE',  ( 15.00000000000000000, 0.000000000000000000, 0.000000000000000000 ) ) ;
#5348 = CARTESIAN_POINT ( 'NONE',  ( 0.000000000000000000, 5.499999999999991118, -178.5000000000000000 ) ) ;
#5349 = AXIS2_PLACEMENT_3D ( 'NONE', #1363, #10772, #20121 ) ;
#5350 = ORIENTED_EDGE ( 'NONE', *, *, #15454, .T. ) ;
#5351 = EDGE_CURVE ( 'NONE', #18174, #11659, #3808, .T. ) ;
#5352 = CARTESIAN_POINT ( 'NONE',  ( 0.000000000000000000, 0.000000000000000000, 0.000000000000000000 ) ) ;
#5353 = CIRCLE ( 'NONE', #22550, 1.000000000000000000 ) ;
#5354 = VERTEX_POINT ( 'NONE', #25145 ) ;
#5355 = ORIENTED_EDGE ( 'NONE', *, *, #18630, .T. ) ;
#5356 = CARTESIAN_POINT ( 'NONE',  ( 133.0312500000000568, -2.485281374238555774, -6.000000000000005329 ) ) ;
#5357 = CARTESIAN_POINT ( 'NONE',  ( 134.1711002691896510, 4.999999999999989342, 2.071067811865468400 ) ) ;
#5358 = ORIENTED_EDGE ( 'NONE', *, *, #2216, .T. ) ;
#5359 = CARTESIAN_POINT ( 'NONE',  ( 3.608439182435180470, -6.249999999999997335, -135.1919872981078470 ) ) ;
#5360 = CARTESIAN_POINT ( 'NONE',  ( -5.196152422706601826, 2.999999999999975131, -130.5386751345948255 ) ) ;
#5361 = CARTESIAN_POINT ( 'NONE',  ( 3.464101615137757051, -5.999999999999979572, -116.4136751345948255 ) ) ;
#5362 = B_SPLINE_CURVE_WITH_KNOTS ( 'NONE', 3,
 ( #3599, #17785, #29095, #3297, #8054, #12723, #22061, #24494, #5748, #1302 ),
 .UNSPECIFIED., .F., .F.,
 ( 4, 2, 2, 2, 4 ),
 ( 0.000000000000000000, 0.0005886548318705546240, 0.0008829822478058313396, 0.001030145955773469806, 0.001177309663741108164 ),
 .UNSPECIFIED. ) ;
#5363 = EDGE_LOOP ( 'NONE', ( #27193, #19442, #20201, #1947 ) ) ;
#5364 = CARTESIAN_POINT ( 'NONE',  ( 15.31250000000006928, -0.8284271247461753029, 1.999999999999911626 ) ) ;
#5365 = CARTESIAN_POINT ( 'NONE',  ( 1.000000004113038354, -16.31584838240407720, -6.338213517867180791 ) ) ;
#5366 = B_SPLINE_CURVE_WITH_KNOTS ( 'NONE', 3,
 ( #25247, #27549, #13484, #8250, #1044, #10285, #17366, #3338, #11167, #12918 ),
 .UNSPECIFIED., .F., .F.,
 ( 4, 2, 2, 2, 4 ),
 ( 0.000000000000000000, 0.0002749695263473663160, 0.0005499390526947326319, 0.001099878105389496489, 0.002199756210779025070 ),
 .UNSPECIFIED. ) ;
#5367 = CARTESIAN_POINT ( 'NONE',  ( 137.0476497308104058, 0.000000000000000000, -5.000000000000004441 ) ) ;
#5368 = DIRECTION ( 'NONE',  ( -1.000000000000000000, -0.000000000000000000, -0.000000000000000000 ) ) ;
#5369 = DIRECTION ( 'NONE',  ( -1.000000000000000000, -1.665334536937731113E-16, 1.526556658859586792E-16 ) ) ;
#5370 = DIRECTION ( 'NONE',  ( 1.000000000000000000, -5.551115123125773458E-17, -1.260129944081490338E-35 ) ) ;
#5371 = CARTESIAN_POINT ( 'NONE',  ( 6.000000000000000888, 1.743066579297358182E-13, -69.08632486540523132 ) ) ;
#5372 = CARTESIAN_POINT ( 'NONE',  ( 105.8124999999999574, 1.035533905932839227, -2.499999999999724221 ) ) ;
#5373 = CIRCLE ( 'NONE', #29420, 5.999999999999998224 ) ;
#5374 = CARTESIAN_POINT ( 'NONE',  ( 4.763139720814407951, -2.749999999999988454, -137.0000000000000000 ) ) ;
#5375 = FACE_OUTER_BOUND ( 'NONE', #12474, .T. ) ;
#5376 = EDGE_LOOP ( 'NONE', ( #11207, #21820, #19522, #21892 ) ) ;
#5377 =( BOUNDED_CURVE ( )  B_SPLINE_CURVE ( 2, ( #27017, #22592, #18146, #8278, #8760, #17538, #20284, #3821, #29632 ),
 .UNSPECIFIED., .F., .F. ) 
 B_SPLINE_CURVE_WITH_KNOTS ( ( 3, 2, 2, 2, 3 ),
 ( 0.07499999999999999722, 0.07592592592592592449, 0.07777777777777777901, 0.07962962962962963354, 0.08055555555555556080 ),
 .UNSPECIFIED. ) 
 CURVE ( )  GEOMETRIC_REPRESENTATION_ITEM ( )  RATIONAL_B_SPLINE_CURVE ( ( 0.9330127018922194093, 0.9330127018922194093, 1.000000000000000000, 0.8660254037844388186, 1.000000000000000000, 0.8660254037844388186, 1.000000000000000000, 0.9330127018922194093, 0.9330127018922194093 ) ) 
 REPRESENTATION_ITEM ( '' )  );
#5378 = EDGE_CURVE ( 'NONE', #2984, #9337, #13230, .T. ) ;
#5379 = LINE ( 'NONE', #788, #6729 ) ;
#5380 = CARTESIAN_POINT ( 'NONE',  ( 6.000000000000000888, -1.859271017917181981E-14, -88.58632486540523132 ) ) ;
#5381 = DIRECTION ( 'NONE',  ( -7.147005652999508048E-36, 5.642372883946980038E-36, 1.000000000000000000 ) ) ;
#5382 = EDGE_CURVE ( 'NONE', #14866, #25911, #18074, .T. ) ;
#5383 = CARTESIAN_POINT ( 'NONE',  ( -3.464101615137757051, -5.999999999999979572, -164.0863248654052029 ) ) ;
#5384 = VERTEX_POINT ( 'NONE', #15535 ) ;
#5385 = CARTESIAN_POINT ( 'NONE',  ( 117.1872167782373708, -1.849990392679441875, -0.7662911109077087390 ) ) ;
#5386 = CARTESIAN_POINT ( 'NONE',  ( 118.4761751345946692, 0.8284271247463257382, 2.000000000000151879 ) ) ;
#5387 = CARTESIAN_POINT ( 'NONE',  ( 3.608439182435180470, -6.249999999999997335, -96.19198729810781856 ) ) ;
#5388 =( BOUNDED_CURVE ( )  B_SPLINE_CURVE ( 2, ( #30146, #16070, #29989, #4336, #22638, #10830, #11127, #3718, #1883 ),
 .UNSPECIFIED., .F., .T. ) 
 B_SPLINE_CURVE_WITH_KNOTS ( ( 3, 2, 2, 2, 3 ),
 ( 0.1750000000000000444, 0.1759259259259259300, 0.1777777777777778123, 0.1796296296296295836, 0.1805555555555554692 ),
 .UNSPECIFIED. ) 
 CURVE ( )  GEOMETRIC_REPRESENTATION_ITEM ( )  RATIONAL_B_SPLINE_CURVE ( ( 0.9330127018922194093, 0.9330127018922234061, 1.000000000000000000, 0.8660254037844388186, 1.000000000000000000, 0.8660254037844388186, 1.000000000000000000, 0.9330127018922234061, 0.9330127018922194093 ) ) 
 REPRESENTATION_ITEM ( '' )  );
#5389 = CARTESIAN_POINT ( 'NONE',  ( 135.0000000000000284, 5.961779907188299532, -0.5849724307333836748 ) ) ;
#5390 = CARTESIAN_POINT ( 'NONE',  ( 157.4136751345948539, 0.000000000000000000, -5.500000000000005329 ) ) ;
#5391 = CARTESIAN_POINT ( 'NONE',  ( 116.4374999999997726, -2.499999999999934719, 1.035533905932929599 ) ) ;
#5392 = CARTESIAN_POINT ( 'NONE',  ( 140.4088296780374492, -11.40882967803873171, 4.170790813163523403 ) ) ;
#5393 = STYLED_ITEM ( 'NONE', ( #21823 ), #27297 ) ;
#5394 = CARTESIAN_POINT ( 'NONE',  ( 0.000000000000000000, 5.499999999999991118, -130.5000000000000000 ) ) ;
#5395 = VERTEX_POINT ( 'NONE', #13084 ) ;
#5396 = ORIENTED_EDGE ( 'NONE', *, *, #19432, .T. ) ;
#5397 = CARTESIAN_POINT ( 'NONE',  ( 161.0000000000000284, -11.67610212985248452, 2.769230769230773603 ) ) ;
#5398 = CARTESIAN_POINT ( 'NONE',  ( 6.350852961086080661, -9.614813431917819062E-14, -55.87500000000003553 ) ) ;
#5399 = DIRECTION ( 'NONE',  ( 1.000000000000000000, -5.551115123125774074E-17, 7.147005652999508048E-36 ) ) ;
#5400 = CARTESIAN_POINT ( 'NONE',  ( -3.464101615137757051, -5.999999999999979572, -59.66367513459482552 ) ) ;
#5401 = CARTESIAN_POINT ( 'NONE',  ( -5.412658773652684552, -3.125000000000099920, -82.43301270189223828 ) ) ;
#5402 = CARTESIAN_POINT ( 'NONE',  ( 0.000000000000000000, 5.999999999999977796, -149.7113248654052313 ) ) ;
#5403 = CARTESIAN_POINT ( 'NONE',  ( 5.196152422706629359, -2.999999999999988898, -168.2113248654052313 ) ) ;
#5404 = CARTESIAN_POINT ( 'NONE',  ( 116.1252832217622881, -5.551115123125782702E-14, -1.849990392679412565 ) ) ;
#5405 = CARTESIAN_POINT ( 'NONE',  ( -2.775557561562891351E-14, -5.500000000000115463, -143.2500000000000000 ) ) ;
#5406 = CARTESIAN_POINT ( 'NONE',  ( 140.4784473477112670, -9.424512066737543492, 7.429532019273854537 ) ) ;
#5407 = CARTESIAN_POINT ( 'NONE',  ( 5.412658773652712085, -3.125000000000086153, -152.4330127018922383 ) ) ;
#5408 = CARTESIAN_POINT ( 'NONE',  ( -6.000000000000000888, 1.067854986875958443E-15, 7.560779664488942560E-35 ) ) ;
#5409 = AXIS2_PLACEMENT_3D ( 'NONE', #16009, #4987, #9775 ) ;
#5410 = CARTESIAN_POINT ( 'NONE',  ( -3.175426480542816066, -5.500000000000057732, -68.37500000000002842 ) ) ;
#5411 = CARTESIAN_POINT ( 'NONE',  ( 145.3988248654052313, 3.889087296526011706, 3.889087296526011706 ) ) ;
#5412 = CARTESIAN_POINT ( 'NONE',  ( -2.775557561562891351E-14, -5.500000000000115463, -59.25000000000002842 ) ) ;
#5413 = EDGE_CURVE ( 'NONE', #13346, #20809, #5158, .T. ) ;
#5414 =( NAMED_UNIT ( * ) PLANE_ANGLE_UNIT ( ) SI_UNIT ( $, .RADIAN. ) );
#5415 = ORIENTED_EDGE ( 'NONE', *, *, #15316, .T. ) ;
#5416 = CARTESIAN_POINT ( 'NONE',  ( 144.4836002691896795, 4.999999999999989342, -2.071067811865468400 ) ) ;
#5417 = CARTESIAN_POINT ( 'NONE',  ( 152.2500000000000284, -6.000000000000005329, 0.000000000000000000 ) ) ;
#5418 = CARTESIAN_POINT ( 'NONE',  ( 18.53867513459497829, 1.665334536937734811E-13, 2.499999999999946709 ) ) ;
#5419 = CARTESIAN_POINT ( 'NONE',  ( 14.50000000000012434, -1.999999999999779732, -5.551115123125782702E-14 ) ) ;
#5420 = CARTESIAN_POINT ( 'NONE',  ( 6.000000000000000888, 1.743066579297358182E-13, -57.66367513459481842 ) ) ;
#5421 = CARTESIAN_POINT ( 'NONE',  ( 5.999999999999949374, 1.607695154586804565, -82.51933756729744118 ) ) ;
#5422 =( BOUNDED_CURVE ( )  B_SPLINE_CURVE ( 2, ( #20106, #13081, #17829, #1047, #29450, #24399, #26683, #3643, #10596 ),
 .UNSPECIFIED., .F., .T. ) 
 B_SPLINE_CURVE_WITH_KNOTS ( ( 3, 2, 2, 2, 3 ),
 ( 0.1416666666666667185, 0.1425925925925926041, 0.1444444444444444864, 0.1462962962962962576, 0.1472222222222221433 ),
 .UNSPECIFIED. ) 
 CURVE ( )  GEOMETRIC_REPRESENTATION_ITEM ( )  RATIONAL_B_SPLINE_CURVE ( ( 0.9330127018922194093, 0.9330127018922234061, 1.000000000000000000, 0.8660254037844388186, 1.000000000000000000, 0.8660254037844388186, 1.000000000000000000, 0.9330127018922234061, 0.9330127018922194093 ) ) 
 REPRESENTATION_ITEM ( '' )  );
#5423 = ORIENTED_EDGE ( 'NONE', *, *, #9428, .F. ) ;
#5424 = CARTESIAN_POINT ( 'NONE',  ( 144.2812500000000284, 2.485281374238585972, 6.000000000000005329 ) ) ;
#5425 = CARTESIAN_POINT ( 'NONE',  ( -5.999999999999963585, 1.780251999655701777E-13, -102.8363248654052313 ) ) ;
#5426 = CARTESIAN_POINT ( 'NONE',  ( 3.175426480543072749, -5.500000000000105693, -176.1250000000000284 ) ) ;
#5427 = CARTESIAN_POINT ( 'NONE',  ( 20.06250000000006750, 2.000000000000151879, 0.8284271247461753029 ) ) ;
#5428 = ORIENTED_EDGE ( 'NONE', *, *, #24962, .T. ) ;
#5429 = CARTESIAN_POINT ( 'NONE',  ( -2.775557561562891351E-14, -5.500000000000115463, -80.25000000000004263 ) ) ;
#5430 = AXIS2_PLACEMENT_3D ( 'NONE', #17576, #29670, #22932 ) ;
#5431 = AXIS2_PLACEMENT_3D ( 'NONE', #5347, #23964, #18926 ) ;
#5432 = CARTESIAN_POINT ( 'NONE',  ( 5.196152422706629359, -2.999999999999988898, -127.7113248654052597 ) ) ;
#5433 = EDGE_CURVE ( 'NONE', #5997, #18475, #26952, .T. ) ;
#5434 = CARTESIAN_POINT ( 'NONE',  ( 6.000000000000000000, 2.951592740943527306E-14, -162.6636751345948824 ) ) ;
#5435 = CARTESIAN_POINT ( 'NONE',  ( 5.792970643772029860, -9.351264793308468271, -23.42496030963405218 ) ) ;
#5436 = CARTESIAN_POINT ( 'NONE',  ( 116.0000000000000142, 0.000000000000000000, 0.000000000000000000 ) ) ;
#5437 = CARTESIAN_POINT ( 'NONE',  ( 140.1363996827915059, -11.13639968279144910, 4.472640761300569423 ) ) ;
#5438 = CARTESIAN_POINT ( 'NONE',  ( -4.763139720814407951, 2.749999999999946709, -160.2500000000000000 ) ) ;
#5439 = CARTESIAN_POINT ( 'NONE',  ( -19.99999999999998224, -54.99999999999990763, -7.500000000000007105 ) ) ;
#5440 = CARTESIAN_POINT ( 'NONE',  ( -6.350852961085760029, -1.281975124255709124E-13, -143.6250000000000000 ) ) ;
#5441 = CARTESIAN_POINT ( 'NONE',  ( 135.0000000000000000, 5.732128757725034163, 1.428824620004477630 ) ) ;
#5442 = CARTESIAN_POINT ( 'NONE',  ( -3.175426480542816066, -5.500000000000057732, -98.37500000000000000 ) ) ;
#5443 = DIRECTION ( 'NONE',  ( -1.000000000000000000, 3.469446951953694061E-16, 0.000000000000000000 ) ) ;
#5444 = CARTESIAN_POINT ( 'NONE',  ( 4.763139720814407951, 2.750000000000002665, -81.25000000000004263 ) ) ;
#5445 = EDGE_CURVE ( 'NONE', #10146, #13609, #12684, .T. ) ;
#5446 = CARTESIAN_POINT ( 'NONE',  ( 14.46132486540527218, 5.551115123125782702E-14, -2.500000000000057732 ) ) ;
#5447 = CARTESIAN_POINT ( 'NONE',  ( -5.999999999999982236, -1.607695154586700426, -136.3466878364870070 ) ) ;
#5448 = CARTESIAN_POINT ( 'NONE',  ( 24.18750000000015277, 0.8284271247463557142, 2.000000000000031530 ) ) ;
#5449 = CARTESIAN_POINT ( 'NONE',  ( 108.9374999999997442, 2.500000000000114575, -1.035533905932508825 ) ) ;
#5450 = CARTESIAN_POINT ( 'NONE',  ( -5.999999999999944933, 1.607695154586759934, -125.9806624327026157 ) ) ;
#5451 = AXIS2_PLACEMENT_3D ( 'NONE', #16014, #25164, #28230 ) ;
#5452 = CYLINDRICAL_SURFACE ( 'NONE', #26850, 5.500000000000000000 ) ;
#5453 = CARTESIAN_POINT ( 'NONE',  ( -2.081668171172168020E-16, -5.204170427930420051E-17, 2.499999999999999112 ) ) ;
#5454 = EDGE_LOOP ( 'NONE', ( #20110, #13772 ) ) ;
#5455 = CARTESIAN_POINT ( 'NONE',  ( 161.2500000000000284, -6.000000000000005329, 0.000000000000000000 ) ) ;
#5456 = FACE_OUTER_BOUND ( 'NONE', #17221, .T. ) ;
#5457 = CARTESIAN_POINT ( 'NONE',  ( 110.2261751345946124, 2.000000000000122125, -0.8284271247459350507 ) ) ;
#5458 = CARTESIAN_POINT ( 'NONE',  ( 120.8752832217622029, -1.849990392679523588, 0.000000000000000000 ) ) ;
#5459 = ORIENTED_EDGE ( 'NONE', *, *, #18431, .F. ) ;
#5460 = ORIENTED_EDGE ( 'NONE', *, *, #14977, .F. ) ;
#5461 =( BOUNDED_CURVE ( )  B_SPLINE_CURVE ( 2, ( #29779, #6743, #1983, #21451, #26185, #11546, #28489, #23043, #382 ),
 .UNSPECIFIED., .F., .F. ) 
 B_SPLINE_CURVE_WITH_KNOTS ( ( 3, 2, 2, 2, 3 ),
 ( 0.2527777777777777679, 0.2537037037037037090, 0.2555555555555555358, 0.2574074074074074181, 0.2583333333333333037 ),
 .UNSPECIFIED. ) 
 CURVE ( )  GEOMETRIC_REPRESENTATION_ITEM ( )  RATIONAL_B_SPLINE_CURVE ( ( 0.9330127018922194093, 0.9330127018922194093, 1.000000000000000000, 0.8660254037844388186, 1.000000000000000000, 0.8660254037844388186, 1.000000000000000000, 0.9330127018922214077, 0.9330127018922194093 ) ) 
 REPRESENTATION_ITEM ( '' )  );
#5462 = CARTESIAN_POINT ( 'NONE',  ( 3.175426480543072749, 5.499999999999865885, -103.6250000000000142 ) ) ;
#5463 = CARTESIAN_POINT ( 'NONE',  ( 18.62500000000008527, 5.551115123125782702E-14, 2.649519052838333888 ) ) ;
#5464 = CARTESIAN_POINT ( 'NONE',  ( 7.216878364870455975, -6.409875621278545621E-14, -125.3080127018922099 ) ) ;
#5465 = EDGE_LOOP ( 'NONE', ( #11801, #2141, #25296, #16813 ) ) ;
#5466 = CARTESIAN_POINT ( 'NONE',  ( 114.1488248654049187, -1.999999999999941602, 0.8284271247462955401 ) ) ;
#5467 = CARTESIAN_POINT ( 'NONE',  ( -3.608439182435052128, -6.250000000000110134, -163.9419872981077901 ) ) ;
#5468 = CARTESIAN_POINT ( 'NONE',  ( 104.9999999999998579, 2.500000000000002220, 0.000000000000000000 ) ) ;
#5469 = CIRCLE ( 'NONE', #25605, 0.9999999999999993339 ) ;
#5470 = CARTESIAN_POINT ( 'NONE',  ( 6.000000000000000888, -1.859271017917181981E-14, -63.66367513459483973 ) ) ;
#5471 = EDGE_CURVE ( 'NONE', #7029, #9852, #28313, .T. ) ;
#5472 = VECTOR ( 'NONE', #29121, 1000.000000000000000 ) ;
#5473 = CARTESIAN_POINT ( 'NONE',  ( -3.608439182435052128, -6.250000000000110134, -61.30801270189223828 ) ) ;
#5474 = ORIENTED_EDGE ( 'NONE', *, *, #5000, .F. ) ;
#5475 = CARTESIAN_POINT ( 'NONE',  ( 6.000000000000000888, -1.859271017917181981E-14, -100.5863248654052171 ) ) ;
#5476 = CARTESIAN_POINT ( 'NONE',  ( -5.920437777358313447, 9.270953676058804049, -24.00610273346770640 ) ) ;
#5477 = SURFACE_STYLE_USAGE ( .BOTH. , #10122 ) ;
#5478 = CARTESIAN_POINT ( 'NONE',  ( -4.763139720814407951, 2.749999999999946709, -169.2500000000000000 ) ) ;
#5479 = CARTESIAN_POINT ( 'NONE',  ( 119.9999999999999289, 2.500000000000057732, 1.110223024625156540E-13 ) ) ;
#5480 = CARTESIAN_POINT ( 'NONE',  ( 152.7113248654052313, 5.500000000000005329, 0.000000000000000000 ) ) ;
#5481 = CARTESIAN_POINT ( 'NONE',  ( 3.608439182435180470, 6.249999999999982236, -168.5580127018922383 ) ) ;
#5482 = CARTESIAN_POINT ( 'NONE',  ( 140.5000000000000284, -11.45643923738959202, -5.000000000000004441 ) ) ;
#5483 = CARTESIAN_POINT ( 'NONE',  ( 24.93750000000011369, 2.000000000000151879, -0.8284271247462354770 ) ) ;
#5484 = CARTESIAN_POINT ( 'NONE',  ( -2.775557561562891351E-14, -5.500000000000115463, -119.2500000000000284 ) ) ;
#5485 = CARTESIAN_POINT ( 'NONE',  ( 0.000000000000000000, -10.00000000000000888, -8.500000000000007105 ) ) ;
#5486 = EDGE_CURVE ( 'NONE', #9495, #7022, #15103, .T. ) ;
#5487 = CARTESIAN_POINT ( 'NONE',  ( -2.775557561562891351E-14, -5.500000000000115463, -116.2500000000000142 ) ) ;
#5488 = CARTESIAN_POINT ( 'NONE',  ( 0.000000000000000000, 5.999999999999977796, -142.7886751345948255 ) ) ;
#5489 = CARTESIAN_POINT ( 'NONE',  ( 6.000000000000000888, -1.859271017917181981E-14, -84.08632486540520290 ) ) ;
#5490 = ORIENTED_EDGE ( 'NONE', *, *, #10200, .T. ) ;
#5491 = CARTESIAN_POINT ( 'NONE',  ( 120.6249999999998295, -1.767766952966376426, -1.767766952966320915 ) ) ;
#5492 = CARTESIAN_POINT ( 'NONE',  ( -5.196152422706601826, 2.999999999999975131, -168.0386751345947971 ) ) ;
#5493 = ORIENTED_EDGE ( 'NONE', *, *, #22387, .F. ) ;
#5494 = CARTESIAN_POINT ( 'NONE',  ( -5.999999999999956479, -1.607695154586745057, -127.3466878364870354 ) ) ;
#5495 = CARTESIAN_POINT ( 'NONE',  ( 2.775557561562891351E-14, 6.250000000000033751, -83.56698729810784698 ) ) ;
#5496 = VERTEX_POINT ( 'NONE', #7913 ) ;
#5497 = CARTESIAN_POINT ( 'NONE',  ( 24.65759742343044536, 1.434127907288146542, -1.856221326699502905 ) ) ;
#5498 = EDGE_LOOP ( 'NONE', ( #29944, #24628, #9666, #28397 ) ) ;
#5499 = CARTESIAN_POINT ( 'NONE',  ( 159.7500000000000284, -6.000000000000005329, 0.000000000000000000 ) ) ;
#5500 =( BOUNDED_CURVE ( )  B_SPLINE_CURVE ( 2, ( #29128, #17356, #1173, #3629, #10278, #29436, #8240, #24526, #22245 ),
 .UNSPECIFIED., .F., .T. ) 
 B_SPLINE_CURVE_WITH_KNOTS ( ( 3, 2, 2, 2, 3 ),
 ( 0.9861111111111111605, 0.9870370370370370461, 0.9888888888888889284, 0.9907407407407406996, 0.9916666666666665853 ),
 .UNSPECIFIED. ) 
 CURVE ( )  GEOMETRIC_REPRESENTATION_ITEM ( )  RATIONAL_B_SPLINE_CURVE ( ( 0.9330127018922194093, 0.9330127018922234061, 1.000000000000000000, 0.8660254037844388186, 1.000000000000000000, 0.8660254037844388186, 1.000000000000000000, 0.9330127018922234061, 0.9330127018922194093 ) ) 
 REPRESENTATION_ITEM ( '' )  );
#5501 =( GEOMETRIC_REPRESENTATION_CONTEXT ( 3 ) GLOBAL_UNCERTAINTY_ASSIGNED_CONTEXT ( ( #16829 ) ) GLOBAL_UNIT_ASSIGNED_CONTEXT ( ( #13979, #19019, #25602 ) ) REPRESENTATION_CONTEXT ( 'NONE', 'WORKASPACE' ) );
#5502 = ORIENTED_EDGE ( 'NONE', *, *, #24632, .F. ) ;
#5503 = CARTESIAN_POINT ( 'NONE',  ( -0.5000000000000004441, -14.50000000000001243, -7.500000000000007105 ) ) ;
#5504 = CARTESIAN_POINT ( 'NONE',  ( -5.412658773652684552, -3.125000000000099920, -131.0669872981078470 ) ) ;
#5505 = CARTESIAN_POINT ( 'NONE',  ( 0.000000000000000000, -5.999999999999991118, -135.4613248654051745 ) ) ;
#5506 = DIRECTION ( 'NONE',  ( 1.000000000000000000, -3.469446951953694061E-16, 0.000000000000000000 ) ) ;
#5507 = CARTESIAN_POINT ( 'NONE',  ( 19.27382486540524553, -2.499999999999964473, -1.035533905932749299 ) ) ;
#5508 = EDGE_CURVE ( 'NONE', #9582, #11212, #21625, .T. ) ;
#5509 = ORIENTED_EDGE ( 'NONE', *, *, #10809, .T. ) ;
#5510 = CARTESIAN_POINT ( 'NONE',  ( 16.87500000000000000, 1.414213562373256572, -1.414213562373145550 ) ) ;
#5511 = DIRECTION ( 'NONE',  ( -7.147005652999508048E-36, 5.642372883946980038E-36, 1.000000000000000000 ) ) ;
#5512 = CARTESIAN_POINT ( 'NONE',  ( 149.9136751345948539, 0.000000000000000000, -5.500000000000005329 ) ) ;
#5513 = FACE_OUTER_BOUND ( 'NONE', #14492, .T. ) ;
#5514 =( BOUNDED_CURVE ( )  B_SPLINE_CURVE ( 2, ( #12807, #10486, #26582, #19404, #19836, #26139, #5084, #2789, #17107 ),
 .UNSPECIFIED., .F., .T. ) 
 B_SPLINE_CURVE_WITH_KNOTS ( ( 3, 2, 2, 2, 3 ),
 ( 0.06388888888888888395, 0.06481481481481481122, 0.06666666666666666574, 0.06851851851851852027, 0.06944444444444444753 ),
 .UNSPECIFIED. ) 
 CURVE ( )  GEOMETRIC_REPRESENTATION_ITEM ( )  RATIONAL_B_SPLINE_CURVE ( ( 0.9330127018922194093, 0.9330127018922194093, 1.000000000000000000, 0.8660254037844388186, 1.000000000000000000, 0.8660254037844388186, 1.000000000000000000, 0.9330127018922194093, 0.9330127018922194093 ) ) 
 REPRESENTATION_ITEM ( '' )  );
#5515 = CARTESIAN_POINT ( 'NONE',  ( 139.1101497308104342, 3.535533905932725318, 3.535533905932725318 ) ) ;
#5516 = CARTESIAN_POINT ( 'NONE',  ( -4.999999999999990230, -24.99999999999999289, 7.500000000000007105 ) ) ;
#5517 = DIRECTION ( 'NONE',  ( 1.000000000000000000, 0.000000000000000000, 0.000000000000000000 ) ) ;
#5518 = FACE_OUTER_BOUND ( 'NONE', #7341, .T. ) ;
#5519 = CARTESIAN_POINT ( 'NONE',  ( 108.1249999999999574, 1.767766952966293159, 1.767766952966431937 ) ) ;
#5520 = CARTESIAN_POINT ( 'NONE',  ( 107.2738248654051176, -1.999999999999941602, -0.8284271247460553989 ) ) ;
#5521 = EDGE_CURVE ( 'NONE', #17667, #11814, #19527, .T. ) ;
#5522 = CARTESIAN_POINT ( 'NONE',  ( -3.175426480542816510, -5.500000000000057732, -138.8750000000000568 ) ) ;
#5523 = TOROIDAL_SURFACE ( 'NONE', #18815, 14.49999999999999822, 0.5000000000000000000 ) ;
#5524 = EDGE_CURVE ( 'NONE', #23417, #226, #5966, .T. ) ;
#5525 = CARTESIAN_POINT ( 'NONE',  ( 153.9449251345948539, -5.500000000000012434, 2.278174593052012309 ) ) ;
#5526 = ORIENTED_EDGE ( 'NONE', *, *, #12260, .F. ) ;
#5527 = CARTESIAN_POINT ( 'NONE',  ( 6.055081547227420202, 6.938893903907228378E-16, -12.50000000000003375 ) ) ;
#5528 = CARTESIAN_POINT ( 'NONE',  ( 4.763139720814407951, 2.750000000000002665, -46.75000000000001421 ) ) ;
#5529 = LINE ( 'NONE', #8294, #43 ) ;
#5530 = LINE ( 'NONE', #923, #17862 ) ;
#5531 = VERTEX_POINT ( 'NONE', #17026 ) ;
#5532 = CARTESIAN_POINT ( 'NONE',  ( 116.8122167782373992, 0.7662911109079189043, 1.849990392679652151 ) ) ;
#5533 = CARTESIAN_POINT ( 'NONE',  ( 136.9687500000000284, -2.485281374238585972, 6.000000000000005329 ) ) ;
#5534 = CARTESIAN_POINT ( 'NONE',  ( 10.93750000000009948, 2.000000000000091926, -0.8284271247462354770 ) ) ;
#5535 = CARTESIAN_POINT ( 'NONE',  ( 2.775557561562891351E-14, 6.250000000000033751, -95.56698729810780435 ) ) ;
#5536 = CARTESIAN_POINT ( 'NONE',  ( -3.464101615137757051, -5.999999999999979572, -50.66367513459485394 ) ) ;
#5537 = CARTESIAN_POINT ( 'NONE',  ( 104.9999999999999716, -0.4876318259226519736, 1.939643060552054266 ) ) ;
#5538 = CARTESIAN_POINT ( 'NONE',  ( 114.3124999999997726, -1.035533905932719101, 2.500000000000205169 ) ) ;
#5539 = CARTESIAN_POINT ( 'NONE',  ( 6.000000000000000888, -1.859271017917181981E-14, -146.1636751345948255 ) ) ;
#5540 = ORIENTED_EDGE ( 'NONE', *, *, #642, .F. ) ;
#5541 = FACE_OUTER_BOUND ( 'NONE', #5801, .T. ) ;
#5542 = VECTOR ( 'NONE', #5996, 1000.000000000000000 ) ;
#5543 = EDGE_LOOP ( 'NONE', ( #2541, #26500, #2838, #7618 ) ) ;
#5544 = CARTESIAN_POINT ( 'NONE',  ( 124.9999999999999432, -69.50000000000000000, -8.000000000000007105 ) ) ;
#5545 = CARTESIAN_POINT ( 'NONE',  ( 3.175426480543072749, 5.499999999999865885, -58.62499999999998579 ) ) ;
#5546 = ADVANCED_FACE ( 'NONE', ( #9793 ), #5452, .F. ) ;
#5547 = LINE ( 'NONE', #13130, #7321 ) ;
#5548 = CARTESIAN_POINT ( 'NONE',  ( 4.520452470708214321, 10.03252783106553103, -21.03609891486515338 ) ) ;
#5549 = CARTESIAN_POINT ( 'NONE',  ( 2.775557561562891351E-14, 6.250000000000033751, -72.43301270189222407 ) ) ;
#5550 = CARTESIAN_POINT ( 'NONE',  ( 116.5863248654051461, 1.414213562373201061, -1.414213562373145550 ) ) ;
#5551 = CARTESIAN_POINT ( 'NONE',  ( 156.9226497308104058, 5.000000000000004441, 0.000000000000000000 ) ) ;
#5552 = CARTESIAN_POINT ( 'NONE',  ( 6.000000000000001776, 5.345404176511898156E-15, -174.0863248654052313 ) ) ;
#5553 = CARTESIAN_POINT ( 'NONE',  ( 19.99999999999998934, -3.608224830031758756E-16, 6.500000000000016875 ) ) ;
#5554 = CARTESIAN_POINT ( 'NONE',  ( 134.9999999999952536, -7.159935056834823008, 8.454462315789898597 ) ) ;
#5555 = EDGE_CURVE ( 'NONE', #15347, #23700, #25107, .T. ) ;
#5556 = CARTESIAN_POINT ( 'NONE',  ( 4.763139720814407951, 2.750000000000002665, -142.7500000000000568 ) ) ;
#5557 = CARTESIAN_POINT ( 'NONE',  ( -3.464101615137725076, 5.999999999999979572, -68.58632486540524553 ) ) ;
#5558 = CARTESIAN_POINT ( 'NONE',  ( -5.412658773652739619, 3.124999999999975131, -151.6830127018922099 ) ) ;
#5559 = CARTESIAN_POINT ( 'NONE',  ( 5.999999999999949374, 1.607695154586804565, -102.0193375672974128 ) ) ;
#5560 = CARTESIAN_POINT ( 'NONE',  ( -3.464101615137725076, 5.999999999999979572, -51.16367513459485394 ) ) ;
#5561 = CARTESIAN_POINT ( 'NONE',  ( 3.175426480543072749, 5.499999999999865885, -73.62500000000007105 ) ) ;
#5562 = CARTESIAN_POINT ( 'NONE',  ( -3.175426480542816510, 5.499999999999865885, -53.87500000000003553 ) ) ;
#5563 =( LENGTH_UNIT ( ) NAMED_UNIT ( * ) SI_UNIT ( .MILLI., .METRE. ) );
#5564 = ORIENTED_EDGE ( 'NONE', *, *, #17253, .F. ) ;
#5565 = CARTESIAN_POINT ( 'NONE',  ( 138.6711002691896510, 4.999999999999989342, 2.071067811865468400 ) ) ;
#5566 = CARTESIAN_POINT ( 'NONE',  ( 151.5000000000000284, 6.000000000000005329, 0.000000000000000000 ) ) ;
#5567 = CARTESIAN_POINT ( 'NONE',  ( -5.196152422706601826, 2.999999999999975131, -133.5386751345948255 ) ) ;
#5568 = DIRECTION ( 'NONE',  ( -1.000000000000000000, -1.665334536937736783E-16, -2.220446049250315546E-16 ) ) ;
#5569 = ORIENTED_EDGE ( 'NONE', *, *, #28138, .T. ) ;
#5570 = CARTESIAN_POINT ( 'NONE',  ( 141.6562500000000284, -6.000000000000005329, 2.485281374238555774 ) ) ;
#5571 = CARTESIAN_POINT ( 'NONE',  ( 142.5863248654052313, 0.000000000000000000, 5.500000000000005329 ) ) ;
#5572 = DIRECTION ( 'NONE',  ( 1.000000000000000000, 0.000000000000000000, -0.000000000000000000 ) ) ;
#5573 = CARTESIAN_POINT ( 'NONE',  ( 5.412658773652712085, -3.125000000000086153, -46.56698729810781856 ) ) ;
#5574 = CARTESIAN_POINT ( 'NONE',  ( 18.31249999999999645, -0.8284271247460553989, 2.000000000000031530 ) ) ;
#5575 = CARTESIAN_POINT ( 'NONE',  ( -3.608439182435115633, 6.249999999999965361, -149.4419872981077901 ) ) ;
#5576 = ORIENTED_EDGE ( 'NONE', *, *, #21518, .F. ) ;
#5577 = CARTESIAN_POINT ( 'NONE',  ( -3.175426480542816510, 5.499999999999865885, -77.87500000000001421 ) ) ;
#5578 = ADVANCED_FACE ( 'NONE', ( #27404 ), #8852, .T. ) ;
#5579 = CARTESIAN_POINT ( 'NONE',  ( 13.81250000000000000, -2.649519052838178457, 1.097466725451499370 ) ) ;
#5580 = EDGE_CURVE ( 'NONE', #9387, #24844, #6225, .T. ) ;
#5581 = CARTESIAN_POINT ( 'NONE',  ( 2.775557561562891351E-14, 6.250000000000033751, -93.43301270189225249 ) ) ;
#5582 = CARTESIAN_POINT ( 'NONE',  ( 119.9999999999999574, 2.481996037641524655, 0.1722232477803059547 ) ) ;
#5583 = FILL_AREA_STYLE_COLOUR ( '', #28917 ) ;
#5584 = CARTESIAN_POINT ( 'NONE',  ( 0.7970850910875092454, -10.97816267869983342, -19.03975521967169016 ) ) ;
#5585 = FACE_BOUND ( 'NONE', #196, .T. ) ;
#5586 = DIRECTION ( 'NONE',  ( -8.326672684688674053E-17, -2.081668171172168513E-17, 1.000000000000000000 ) ) ;
#5587 = CIRCLE ( 'NONE', #17413, 14.99999999999998579 ) ;
#5588 = CARTESIAN_POINT ( 'NONE',  ( -4.763139720814407951, -2.750000000000016431, -163.0000000000000284 ) ) ;
#5589 = CARTESIAN_POINT ( 'NONE',  ( 144.8363248654052029, 0.000000000000000000, -5.500000000000005329 ) ) ;
#5590 = CARTESIAN_POINT ( 'NONE',  ( -3.175426480542816510, -5.500000000000057732, -146.3750000000000284 ) ) ;
#5591 = CARTESIAN_POINT ( 'NONE',  ( 19.96132486540530593, 5.551115123125782702E-14, 2.500000000000002220 ) ) ;
#5592 = CARTESIAN_POINT ( 'NONE',  ( 149.1488248654052029, -3.889087296526011706, -3.889087296526011706 ) ) ;
#5593 = CARTESIAN_POINT ( 'NONE',  ( -6.350852961085760029, -1.281975124255709124E-13, -94.12500000000001421 ) ) ;
#5594 = CARTESIAN_POINT ( 'NONE',  ( -3.464101615137725076, 5.999999999999979572, -125.5863248654051887 ) ) ;
#5595 = CARTESIAN_POINT ( 'NONE',  ( -5.196152422706573404, -3.000000000000002665, -131.2113248654052029 ) ) ;
#5596 = CARTESIAN_POINT ( 'NONE',  ( 0.000000000000000000, 5.499999999999991118, -79.50000000000001421 ) ) ;
#5597 =( BOUNDED_CURVE ( )  B_SPLINE_CURVE ( 2, ( #20760, #25489, #23522, #18771, #28540, #28245, #4899, #4756, #25807 ),
 .UNSPECIFIED., .F., .T. ) 
 B_SPLINE_CURVE_WITH_KNOTS ( ( 3, 2, 2, 2, 3 ),
 ( 0.6764705882352941568, 0.6838235294117647189, 0.6911764705882352811, 0.6985294117647058432, 0.7058823529411764053 ),
 .UNSPECIFIED. ) 
 CURVE ( )  GEOMETRIC_REPRESENTATION_ITEM ( )  RATIONAL_B_SPLINE_CURVE ( ( 1.000000000000000000, 0.9238795325112867385, 1.000000000000000000, 0.9238795325112867385, 1.000000000000000000, 0.9238795325112867385, 1.000000000000000000, 0.9238795325112867385, 1.000000000000000000 ) ) 
 REPRESENTATION_ITEM ( '' )  );
#5598 = CARTESIAN_POINT ( 'NONE',  ( 153.0148502691896510, -3.535533905932725318, -3.535533905932725318 ) ) ;
#5599 = CARTESIAN_POINT ( 'NONE',  ( 5.196152422706629359, 3.000000000000002665, -65.03867513459482552 ) ) ;
#5600 = CARTESIAN_POINT ( 'NONE',  ( 0.000000000000000000, 0.000000000000000000, -44.99152654425658682 ) ) ;
#5601 = CARTESIAN_POINT ( 'NONE',  ( 22.12500000000006040, 1.414213562373145550, 1.414213562373201061 ) ) ;
#5602 = CARTESIAN_POINT ( 'NONE',  ( 0.000000000000000000, 0.000000000000000000, 0.000000000000000000 ) ) ;
#5603 = CARTESIAN_POINT ( 'NONE',  ( 5.196152422706629359, 3.000000000000002665, -78.53867513459483973 ) ) ;
#5604 = ORIENTED_EDGE ( 'NONE', *, *, #5140, .F. ) ;
#5605 = CARTESIAN_POINT ( 'NONE',  ( 159.3750000000000568, 0.000000000000000000, 6.000000000000005329 ) ) ;
#5606 = DIRECTION ( 'NONE',  ( 5.551115123125785167E-17, -1.000000000000000000, -8.881784197001256268E-16 ) ) ;
#5607 = CARTESIAN_POINT ( 'NONE',  ( 145.9761751345948255, 3.889087296526011706, 3.889087296526011706 ) ) ;
#5608 = CARTESIAN_POINT ( 'NONE',  ( 120.5627832217621460, 0.7662911109078287542, 1.849990392679652151 ) ) ;
#5609 = CARTESIAN_POINT ( 'NONE',  ( 24.92558298569622366, 1.541947152209776295, -1.394316296550170531 ) ) ;
#5610 = ORIENTED_EDGE ( 'NONE', *, *, #14882, .F. ) ;
#5611 = ORIENTED_EDGE ( 'NONE', *, *, #17707, .T. ) ;
#5612 = CARTESIAN_POINT ( 'NONE',  ( 3.175426480543072749, -5.500000000000105693, -104.1250000000000142 ) ) ;
#5613 = CARTESIAN_POINT ( 'NONE',  ( 17.81250000000009592, -2.649519052838178457, 1.097466725451559322 ) ) ;
#5614 = EDGE_CURVE ( 'NONE', #20028, #13346, #28130, .T. ) ;
#5615 = CARTESIAN_POINT ( 'NONE',  ( 3.608439182435180470, 6.249999999999982236, -114.5580127018922241 ) ) ;
#5616 = VERTEX_POINT ( 'NONE', #13336 ) ;
#5617 = DIRECTION ( 'NONE',  ( -1.000000000000000000, -1.665334536937731113E-16, 1.526556658859586792E-16 ) ) ;
#5618 = CARTESIAN_POINT ( 'NONE',  ( 3.608439182435180470, 6.249999999999982236, -161.6919872981078470 ) ) ;
#5619 = CARTESIAN_POINT ( 'NONE',  ( 106.0624999999998295, 2.500000000000114575, 1.035533905933049725 ) ) ;
#5620 = VECTOR ( 'NONE', #15943, 1000.000000000000227 ) ;
#5621 = CARTESIAN_POINT ( 'NONE',  ( -5.412658773652684552, -3.125000000000099920, -59.93301270189221697 ) ) ;
#5622 = EDGE_LOOP ( 'NONE', ( #21711, #25592, #14757, #7921 ) ) ;
#5623 = CARTESIAN_POINT ( 'NONE',  ( 0.000000000000000000, -14.14213562373095634, -8.500000000000007105 ) ) ;
#5624 = CARTESIAN_POINT ( 'NONE',  ( 22.72617513459488592, -2.499999999999964473, 1.035533905932749299 ) ) ;
#5625 = CARTESIAN_POINT ( 'NONE',  ( -5.608370619328715279, 9.463293048187475520, -22.85879529262371079 ) ) ;
#5626 = CARTESIAN_POINT ( 'NONE',  ( -1.110223024625164676E-16, 2.000000000000012879, 2.021286199229734960E-15 ) ) ;
#5627 = CARTESIAN_POINT ( 'NONE',  ( 0.000000000000000000, 5.499999999999991118, -172.5000000000000000 ) ) ;
#5628 = CARTESIAN_POINT ( 'NONE',  ( 119.7499999999998721, 1.110223024625156540E-13, -2.499999999999946709 ) ) ;
#5629 = CARTESIAN_POINT ( 'NONE',  ( -0.04562205425674009662, -14.50000000000001243, 8.291335958003937634 ) ) ;
#5630 = CARTESIAN_POINT ( 'NONE',  ( 2.775557561562891351E-14, 6.250000000000033751, -165.4330127018922667 ) ) ;
#5631 = CARTESIAN_POINT ( 'NONE',  ( 154.8675748654052313, -5.500000000000012434, 2.278174593052012309 ) ) ;
#5632 = CARTESIAN_POINT ( 'NONE',  ( 23.50000000000010303, -1.999999999999779732, -5.551115123125782702E-14 ) ) ;
#5633 = VECTOR ( 'NONE', #11216, 1000.000000000000000 ) ;
#5634 = CARTESIAN_POINT ( 'NONE',  ( 3.175426480543072749, -5.500000000000105693, -113.1249999999999858 ) ) ;
#5635 = CARTESIAN_POINT ( 'NONE',  ( 135.6334262937400013, -8.691027319329242218, 8.179640144927386558 ) ) ;
#5636 = CARTESIAN_POINT ( 'NONE',  ( 3.175426480543072749, 5.499999999999865885, -103.6250000000000142 ) ) ;
#5637 = CARTESIAN_POINT ( 'NONE',  ( -1.000000000000000888, 10.00000000000000888, -4.000000000000003553 ) ) ;
#5638 = AXIS2_PLACEMENT_3D ( 'NONE', #16043, #22617, #15424 ) ;
#5639 = CYLINDRICAL_SURFACE ( 'NONE', #22033, 6.000000000000000888 ) ;
#5640 = CARTESIAN_POINT ( 'NONE',  ( 148.7886751345948255, 5.500000000000005329, 0.000000000000000000 ) ) ;
#5641 = ORIENTED_EDGE ( 'NONE', *, *, #10974, .T. ) ;
#5642 = CARTESIAN_POINT ( 'NONE',  ( 14.37500000000008171, 1.665334536937734811E-13, -2.649519052838444910 ) ) ;
#5643 = CARTESIAN_POINT ( 'NONE',  ( 119.8749999999998863, 1.767766952966320915, -1.767766952966320915 ) ) ;
#5644 = CARTESIAN_POINT ( 'NONE',  ( 6.000000000000052403, -1.607695154586662678, -71.23066243270258724 ) ) ;
#5645 = EDGE_LOOP ( 'NONE', ( #15543, #29532, #5350 ) ) ;
#5646 = MECHANICAL_DESIGN_GEOMETRIC_PRESENTATION_REPRESENTATION (  '', ( #21389 ), #3696 ) ;
#5647 = EDGE_CURVE ( 'NONE', #4838, #11174, #15800, .T. ) ;
#5648 = CARTESIAN_POINT ( 'NONE',  ( 3.608439182435180470, -6.249999999999997335, -85.69198729810781856 ) ) ;
#5649 =( BOUNDED_CURVE ( )  B_SPLINE_CURVE ( 2, ( #27160, #17841, #10925, #25007, #11388, #20575, #29925, #13387, #6422 ),
 .UNSPECIFIED., .F., .F. ) 
 B_SPLINE_CURVE_WITH_KNOTS ( ( 3, 2, 2, 2, 3 ),
 ( 0.1527777777777777901, 0.1537037037037037035, 0.1555555555555555580, 0.1574074074074074125, 0.1583333333333333259 ),
 .UNSPECIFIED. ) 
 CURVE ( )  GEOMETRIC_REPRESENTATION_ITEM ( )  RATIONAL_B_SPLINE_CURVE ( ( 0.9330127018922194093, 0.9330127018922204085, 1.000000000000000000, 0.8660254037844388186, 1.000000000000000000, 0.8660254037844388186, 1.000000000000000000, 0.9330127018922205195, 0.9330127018922196314 ) ) 
 REPRESENTATION_ITEM ( '' )  );
#5650 = PRESENTATION_STYLE_ASSIGNMENT (( #3193 ) ) ;
#5651 = EDGE_LOOP ( 'NONE', ( #3875, #16494, #24039, #26726 ) ) ;
#5652 = ORIENTED_EDGE ( 'NONE', *, *, #23751, .F. ) ;
#5653 = CARTESIAN_POINT ( 'NONE',  ( 161.3437500000000568, -6.000000000000005329, -2.485281374238555774 ) ) ;
#5654 = EDGE_CURVE ( 'NONE', #5729, #4566, #8533, .T. ) ;
#5655 = ORIENTED_EDGE ( 'NONE', *, *, #17078, .F. ) ;
#5656 = CIRCLE ( 'NONE', #13573, 9.999999999999980460 ) ;
#5657 = CARTESIAN_POINT ( 'NONE',  ( 7.216878364870455975, -6.409875621278545621E-14, -134.9419872981077901 ) ) ;
#5658 = DIRECTION ( 'NONE',  ( 1.000000000000000000, -0.000000000000000000, -0.000000000000000000 ) ) ;
#5659 = CARTESIAN_POINT ( 'NONE',  ( 6.000000000000000888, 1.607695154586715303, -84.01933756729741276 ) ) ;
#5660 = FACE_OUTER_BOUND ( 'NONE', #2354, .T. ) ;
#5661 = CARTESIAN_POINT ( 'NONE',  ( 14.75000000000009592, 2.220446049250313081E-13, -2.000000000000057288 ) ) ;
#5662 = CARTESIAN_POINT ( 'NONE',  ( 111.2113248654051176, -1.999999999999946265, 0.000000000000000000 ) ) ;
#5663 = DIRECTION ( 'NONE',  ( 1.000000000000000000, -5.551115123125773458E-17, -1.260129944081490338E-35 ) ) ;
#5664 = CARTESIAN_POINT ( 'NONE',  ( 134.8913997308104342, -2.071067811865468400, 4.999999999999989342 ) ) ;
#5665 = CARTESIAN_POINT ( 'NONE',  ( 12.08632486540531303, -1.767766952966209892, 1.767766952966431937 ) ) ;
#5666 = CARTESIAN_POINT ( 'NONE',  ( 0.000000000000000000, 2.678141147339105664E-16, 4.000000000000000000 ) ) ;
#5667 = CARTESIAN_POINT ( 'NONE',  ( -7.216878364870328078, 0.000000000000000000, -66.69198729810779014 ) ) ;
#5668 = VECTOR ( 'NONE', #666, 1000.000000000000000 ) ;
#5669 = CARTESIAN_POINT ( 'NONE',  ( -3.608439182435052128, -6.250000000000110134, -52.94198729810779014 ) ) ;
#5670 = CARTESIAN_POINT ( 'NONE',  ( 119.9999999999997584, 2.338294422933281602, -0.6637900606688733607 ) ) ;
#5671 = CARTESIAN_POINT ( 'NONE',  ( -5.999999999999963585, -1.487416814333745711E-14, -127.4136751345948113 ) ) ;
#5672 = CARTESIAN_POINT ( 'NONE',  ( -2.775557561562891351E-14, -5.500000000000115463, -128.2500000000000284 ) ) ;
#5673 = DIRECTION ( 'NONE',  ( 1.000000000000000000, -5.551115123125773458E-17, -1.260129944081490338E-35 ) ) ;
#5674 = EDGE_LOOP ( 'NONE', ( #20692, #26403, #27338, #8502 ) ) ;
#5675 = FACE_OUTER_BOUND ( 'NONE', #9471, .T. ) ;
#5676 = CARTESIAN_POINT ( 'NONE',  ( -5.999999999999866773, 1.607695154586893826, -119.4033121635130215 ) ) ;
#5677 = CARTESIAN_POINT ( 'NONE',  ( -39.99999999999998579, -59.99999999999980105, 3.000000000000002665 ) ) ;
#5678 = LINE ( 'NONE', #9754, #22340 ) ;
#5679 = ORIENTED_EDGE ( 'NONE', *, *, #384, .F. ) ;
#5680 = CARTESIAN_POINT ( 'NONE',  ( 114.7497167782374561, 1.308140751793751555, 1.308140751793973600 ) ) ;
#5681 = CARTESIAN_POINT ( 'NONE',  ( 135.1875000000000568, 4.242640687119269671, 4.242640687119298093 ) ) ;
#5682 = CARTESIAN_POINT ( 'NONE',  ( 11.37500000000010658, -1.414213562372979016, 1.414213562372979016 ) ) ;
#5683 = ADVANCED_FACE ( 'NONE', ( #4065 ), #22678, .T. ) ;
#5684 = CARTESIAN_POINT ( 'NONE',  ( 7.216878364870455975, -6.409875621278545621E-14, -97.44198729810781856 ) ) ;
#5685 = CARTESIAN_POINT ( 'NONE',  ( 0.000000000000000000, -5.999999999999991118, -78.46132486540524553 ) ) ;
#5686 =( BOUNDED_CURVE ( )  B_SPLINE_CURVE ( 2, ( #12640, #632, #9870, #5525, #16949, #19683, #7688, #28422, #12797 ),
 .UNSPECIFIED., .F., .T. ) 
 B_SPLINE_CURVE_WITH_KNOTS ( ( 3, 2, 2, 2, 3 ),
 ( 0.7124999999999992450, 0.7187499999999994449, 0.7249999999999996447, 0.7312499999999999556, 0.7375000000000002665 ),
 .UNSPECIFIED. ) 
 CURVE ( )  GEOMETRIC_REPRESENTATION_ITEM ( )  RATIONAL_B_SPLINE_CURVE ( ( 1.000000000000009548, 0.9238795325112773016, 1.000000000000000000, 0.9238795325112867385, 1.000000000000000000, 0.9238795325112867385, 1.000000000000000000, 0.9238795325112840739, 1.000000000000002665 ) ) 
 REPRESENTATION_ITEM ( '' )  );
#5687 = CARTESIAN_POINT ( 'NONE',  ( 155.4449251345948255, -5.500000000000012434, 2.278174593052012309 ) ) ;
#5688 = CARTESIAN_POINT ( 'NONE',  ( 113.3124999999997300, -1.035533905932598975, 2.500000000000144773 ) ) ;
#5689 = EDGE_LOOP ( 'NONE', ( #29303, #21241, #25951, #7152 ) ) ;
#5690 = CARTESIAN_POINT ( 'NONE',  ( 141.0000000000000284, -12.00000000000001066, 4.000000000000003553 ) ) ;
#5691 = EDGE_CURVE ( 'NONE', #16117, #1801, #22859, .T. ) ;
#5692 = ORIENTED_EDGE ( 'NONE', *, *, #4417, .F. ) ;
#5693 = CARTESIAN_POINT ( 'NONE',  ( 24.93750000000014211, -2.649519052838178457, -1.097466725451619718 ) ) ;
#5694 = ORIENTED_EDGE ( 'NONE', *, *, #12743, .T. ) ;
#5695 = CARTESIAN_POINT ( 'NONE',  ( 18.72617513459488237, -2.499999999999964473, 1.035533905932689347 ) ) ;
#5696 = CARTESIAN_POINT ( 'NONE',  ( -3.175426480542816510, -5.500000000000057732, -48.87500000000001421 ) ) ;
#5698 = VECTOR ( 'NONE', #21580, 1000.000000000000000 ) ;
#5697 = B_SPLINE_CURVE_WITH_KNOTS ( 'NONE', 1,
 ( #26409, #24112 ),
 .UNSPECIFIED., .F., .F.,
 ( 2, 2 ),
 ( 0.000000000000000000, 1.000000000000000000 ),
 .UNSPECIFIED. ) ;
#5699 = CARTESIAN_POINT ( 'NONE',  ( -4.999999999999990230, -24.99999999999999289, -5.000000000000004441 ) ) ;
#5700 = DIRECTION ( 'NONE',  ( -7.147005652999508048E-36, 5.642372883946980038E-36, 1.000000000000000000 ) ) ;
#5701 = CARTESIAN_POINT ( 'NONE',  ( -3.608439182435052128, -6.250000000000110134, -77.80801270189225249 ) ) ;
#5702 = FACE_OUTER_BOUND ( 'NONE', #19699, .T. ) ;
#5703 = CARTESIAN_POINT ( 'NONE',  ( 157.2038997308104058, 2.071067811865468400, 4.999999999999989342 ) ) ;
#5704 = CARTESIAN_POINT ( 'NONE',  ( 5.999999999999949374, 1.607695154586804565, -169.5193375672974696 ) ) ;
#5705 = CARTESIAN_POINT ( 'NONE',  ( -5.999999999999963585, 9.296355089585909904E-15, -168.8363248654052029 ) ) ;
#5706 = CYLINDRICAL_SURFACE ( 'NONE', #29489, 6.000000000000000888 ) ;
#5707 = CARTESIAN_POINT ( 'NONE',  ( -2.775557561562891351E-14, -5.500000000000115463, -135.7500000000000284 ) ) ;
#5708 = CARTESIAN_POINT ( 'NONE',  ( 105.2886751345946550, 2.000000000000057288, 0.000000000000000000 ) ) ;
#5709 = CARTESIAN_POINT ( 'NONE',  ( -5.999999999999971578, 1.607695154586715303, -101.4033121635129930 ) ) ;
#5710 = CARTESIAN_POINT ( 'NONE',  ( 6.000000000000000888, -1.607695154586752384, -72.73066243270262987 ) ) ;
#5711 = CARTESIAN_POINT ( 'NONE',  ( 4.763139720814407951, 2.750000000000002665, -69.25000000000002842 ) ) ;
#5712 = CARTESIAN_POINT ( 'NONE',  ( -3.175426480542816510, -5.500000000000057732, -59.37500000000005684 ) ) ;
#5713 = DIRECTION ( 'NONE',  ( 1.000000000000000000, 1.794541526872559254E-15, 0.000000000000000000 ) ) ;
#5714 = VERTEX_POINT ( 'NONE', #6074 ) ;
#5715 = CARTESIAN_POINT ( 'NONE',  ( 151.8750000000000284, 0.000000000000000000, 6.000000000000005329 ) ) ;
#5716 = CARTESIAN_POINT ( 'NONE',  ( -5.999999999999963585, 1.780251999655701777E-13, -89.91367513459485394 ) ) ;
#5717 = VECTOR ( 'NONE', #8671, 1000.000000000000114 ) ;
#5718 = ADVANCED_FACE ( 'NONE', ( #29251 ), #16437, .T. ) ;
#5719 = CARTESIAN_POINT ( 'NONE',  ( -5.999999999999963585, 1.780251999655701777E-13, -58.41367513459482552 ) ) ;
#5720 = CARTESIAN_POINT ( 'NONE',  ( 111.2497167782375982, -1.308140751793640533, -1.308140751793640533 ) ) ;
#5721 = ORIENTED_EDGE ( 'NONE', *, *, #29940, .F. ) ;
#5722 = CARTESIAN_POINT ( 'NONE',  ( 145.8750000000000284, 0.000000000000000000, 6.000000000000005329 ) ) ;
#5723 = CARTESIAN_POINT ( 'NONE',  ( 161.3386106984802097, -5.845894788924955954, 0.1212874700761470553 ) ) ;
#5724 = COLOUR_RGB ( '', 0.09019608, 0.27058824, 0.51372549) ;
#5725 = EDGE_CURVE ( 'NONE', #14931, #17836, #24270, .T. ) ;
#5726 = CARTESIAN_POINT ( 'NONE',  ( -4.763139720814407951, -2.750000000000016431, -143.5000000000000284 ) ) ;
#5727 = CARTESIAN_POINT ( 'NONE',  ( 0.000000000000000000, 5.499999999999991118, -181.5000000000000000 ) ) ;
#5728 = CARTESIAN_POINT ( 'NONE',  ( 17.00000000000015277, 2.000000000000112799, 0.000000000000000000 ) ) ;
#5729 = VERTEX_POINT ( 'NONE', #13932 ) ;
#5730 = CARTESIAN_POINT ( 'NONE',  ( 2.775557561562891351E-14, 6.250000000000033751, -145.0669872981078470 ) ) ;
#5731 = CARTESIAN_POINT ( 'NONE',  ( -4.763139720814407951, 2.749999999999946709, -77.74999999999998579 ) ) ;
#5732 = CARTESIAN_POINT ( 'NONE',  ( 14.00000000000006750, -1.873492889144789952, -1.873492889145123019 ) ) ;
#5733 = CARTESIAN_POINT ( 'NONE',  ( 5.412658773652712085, -3.125000000000086153, -95.43301270189225249 ) ) ;
#5734 = ORIENTED_EDGE ( 'NONE', *, *, #7157, .T. ) ;
#5735 = DIRECTION ( 'NONE',  ( -1.000000000000000000, -1.387778780781444413E-14, 0.000000000000000000 ) ) ;
#5736 = DIRECTION ( 'NONE',  ( -7.147005652999508048E-36, 5.642372883946980038E-36, 1.000000000000000000 ) ) ;
#5737 = CARTESIAN_POINT ( 'NONE',  ( 135.0000000000000284, -12.00000000000001066, 5.000000000000004441 ) ) ;
#5738 = CARTESIAN_POINT ( 'NONE',  ( 6.000000000000052403, -1.607695154586662678, -90.73066243270264408 ) ) ;
#5739 = CARTESIAN_POINT ( 'NONE',  ( 3.464101615137757051, -5.999999999999979572, -58.83632486540520290 ) ) ;
#5740 = COLOUR_RGB ( '', 0.08235294, 0.09019608, 0.10196078) ;
#5741 = SURFACE_STYLE_USAGE ( .BOTH. , #24481 ) ;
#5742 = CARTESIAN_POINT ( 'NONE',  ( -6.350852961085760029, -1.281975124255709124E-13, -152.6250000000000284 ) ) ;
#5743 = CARTESIAN_POINT ( 'NONE',  ( 3.175426480543072749, 5.499999999999865885, -144.1250000000000000 ) ) ;
#5744 = FACE_OUTER_BOUND ( 'NONE', #14861, .T. ) ;
#5745 = FACE_OUTER_BOUND ( 'NONE', #2945, .T. ) ;
#5746 = CARTESIAN_POINT ( 'NONE',  ( -4.763139720814407951, 2.749999999999946709, -79.25000000000004263 ) ) ;
#5747 = CARTESIAN_POINT ( 'NONE',  ( 150.1011751345948539, 3.889087296526011706, -3.889087296526011706 ) ) ;
#5748 = CARTESIAN_POINT ( 'NONE',  ( 139.5500150635274963, -9.165151389911695645, -8.000000000000007105 ) ) ;
#5749 = CARTESIAN_POINT ( 'NONE',  ( -3.464101615137725076, 5.999999999999979572, -131.5863248654052313 ) ) ;
#5750 = CARTESIAN_POINT ( 'NONE',  ( 22.37500000000011724, -1.414213562372979016, 1.414213562372979016 ) ) ;
#5751 = CARTESIAN_POINT ( 'NONE',  ( -3.464101615137757051, -5.999999999999979572, -165.5863248654052029 ) ) ;
#5752 = EDGE_CURVE ( 'NONE', #27492, #24705, #19544, .T. ) ;
#5753 = CARTESIAN_POINT ( 'NONE',  ( 6.000000000000000888, 1.607695154586715303, -72.59668783648704959 ) ) ;
#5754 = EDGE_CURVE ( 'NONE', #1086, #11750, #4655, .T. ) ;
#5755 = ORIENTED_EDGE ( 'NONE', *, *, #24519, .F. ) ;
#5756 = CARTESIAN_POINT ( 'NONE',  ( -5.999999999999968026, -1.607695154586722186, -157.3466878364870070 ) ) ;
#5757 = CARTESIAN_POINT ( 'NONE',  ( -5.196152422706573404, -3.000000000000002665, -79.28867513459481131 ) ) ;
#5758 = CARTESIAN_POINT ( 'NONE',  ( 104.8122167782375129, 0.7662911109077388261, 1.849990392679712103 ) ) ;
#5759 = CARTESIAN_POINT ( 'NONE',  ( 24.98686014176553982, 2.013139858234869184, -0.2747217959037423496 ) ) ;
#5760 = MECHANICAL_DESIGN_GEOMETRIC_PRESENTATION_REPRESENTATION (  '', ( #20501 ), #12682 ) ;
#5761 = ORIENTED_EDGE ( 'NONE', *, *, #26226, .T. ) ;
#5762 = VECTOR ( 'NONE', #27532, 1000.000000000000000 ) ;
#5763 = ORIENTED_EDGE ( 'NONE', *, *, #7595, .T. ) ;
#5764 = CARTESIAN_POINT ( 'NONE',  ( 3.175426480543072749, -5.500000000000105693, -108.6250000000000284 ) ) ;
#5765 = CARTESIAN_POINT ( 'NONE',  ( 16.43750000000002132, 2.649519052838298805, 1.097466725451559322 ) ) ;
#5766 = CARTESIAN_POINT ( 'NONE',  ( -5.412658773652739619, 3.124999999999975131, -118.6830127018922383 ) ) ;
#5767 = EDGE_LOOP ( 'NONE', ( #10076, #17347, #26510, #3605, #22654 ) ) ;
#5768 = LINE ( 'NONE', #21638, #9301 ) ;
#5769 = CARTESIAN_POINT ( 'NONE',  ( -5.412658773652739619, 3.124999999999975131, -156.8169872981078470 ) ) ;
#5770 = CARTESIAN_POINT ( 'NONE',  ( -6.000000000000000888, 1.067854986875958443E-15, 7.560779664488942560E-35 ) ) ;
#5771 = CARTESIAN_POINT ( 'NONE',  ( 147.6636751345948255, 0.000000000000000000, 5.500000000000005329 ) ) ;
#5772 = ORIENTED_EDGE ( 'NONE', *, *, #11999, .F. ) ;
#5773 = CARTESIAN_POINT ( 'NONE',  ( 124.9999999999999432, -65.00000000000000000, 7.500000000000007105 ) ) ;
#5774 = CARTESIAN_POINT ( 'NONE',  ( 115.9136751345946266, -1.414213562373006772, -1.414213562373034527 ) ) ;
#5775 =( BOUNDED_CURVE ( )  B_SPLINE_CURVE ( 2, ( #19636, #19193, #26523, #19346, #28665, #16903, #28522, #7492, #7639 ),
 .UNSPECIFIED., .F., .T. ) 
 B_SPLINE_CURVE_WITH_KNOTS ( ( 3, 2, 2, 2, 3 ),
 ( 0.6361111111111110716, 0.6370370370370370683, 0.6388888888888888395, 0.6407407407407407218, 0.6416666666666666075 ),
 .UNSPECIFIED. ) 
 CURVE ( )  GEOMETRIC_REPRESENTATION_ITEM ( )  RATIONAL_B_SPLINE_CURVE ( ( 0.9330127018922194093, 0.9330127018922154125, 1.000000000000000000, 0.8660254037844388186, 1.000000000000000000, 0.8660254037844388186, 1.000000000000000000, 0.9330127018922234061, 0.9330127018922194093 ) ) 
 REPRESENTATION_ITEM ( '' )  );
#5776 = DIRECTION ( 'NONE',  ( -1.000000000000000000, 0.000000000000000000, 0.000000000000000000 ) ) ;
#5777 = CARTESIAN_POINT ( 'NONE',  ( 3.175426480543072749, 5.499999999999865885, -168.1250000000000000 ) ) ;
#5778 = CARTESIAN_POINT ( 'NONE',  ( 118.2499999999997584, -8.326672684688674053E-14, 2.500000000000057732 ) ) ;
#5779 = CARTESIAN_POINT ( 'NONE',  ( 7.216878364870455975, -6.409875621278545621E-14, -171.8080127018922667 ) ) ;
#5780 = CARTESIAN_POINT ( 'NONE',  ( -9.757819552369539906E-16, -9.500000000000008882, 5.000000000000004441 ) ) ;
#5781 = CARTESIAN_POINT ( 'NONE',  ( 23.87500000000009237, 1.414213562373256572, -1.414213562373145550 ) ) ;
#5782 = CARTESIAN_POINT ( 'NONE',  ( 3.175426480543072749, 5.499999999999865885, -114.1249999999999858 ) ) ;
#5783 = FILL_AREA_STYLE_COLOUR ( '', #9016 ) ;
#5784 = CARTESIAN_POINT ( 'NONE',  ( 3.175426480543072749, 5.499999999999865885, -105.1250000000000284 ) ) ;
#5785 = CARTESIAN_POINT ( 'NONE',  ( 5.999999999999988454, 1.607695154586737729, -152.0966878364870638 ) ) ;
#5786 = CARTESIAN_POINT ( 'NONE',  ( -5.196152422706601826, 2.999999999999975131, -117.9613248654052313 ) ) ;
#5787 = EDGE_LOOP ( 'NONE', ( #26251, #8710, #19864, #4114 ) ) ;
#5788 = CARTESIAN_POINT ( 'NONE',  ( 16.25000000000012434, -1.873492889144845464, -1.873492889145123019 ) ) ;
#5789 = CARTESIAN_POINT ( 'NONE',  ( 119.0624999999998295, 2.500000000000024425, 1.035533905932809473 ) ) ;
#5790 = CARTESIAN_POINT ( 'NONE',  ( -4.999999999999886313, -9.000000000000007105, -5.000000000000004441 ) ) ;
#5791 = EDGE_CURVE ( 'NONE', #25744, #1672, #15626, .T. ) ;
#5792 = EDGE_LOOP ( 'NONE', ( #23597, #17827, #10147, #3954 ) ) ;
#5793 = CARTESIAN_POINT ( 'NONE',  ( 3.175426480543072749, -5.500000000000105693, -159.6250000000000284 ) ) ;
#5794 = CARTESIAN_POINT ( 'NONE',  ( 5.196152422706629359, 3.000000000000002665, -156.5386751345948539 ) ) ;
#5795 = CARTESIAN_POINT ( 'NONE',  ( 109.9372167782373424, -0.7662911109076785410, 1.849990392679712103 ) ) ;
#5796 = CARTESIAN_POINT ( 'NONE',  ( 3.608439182435180470, -6.249999999999997335, -78.19198729810784698 ) ) ;
#5797 = CARTESIAN_POINT ( 'NONE',  ( 135.8257310488615133, -9.165151389911695645, 8.000000000000007105 ) ) ;
#5798 = VERTEX_POINT ( 'NONE', #6508 ) ;
#5799 = CARTESIAN_POINT ( 'NONE',  ( 24.69685486351175996, 1.596793880121103681, -1.664379001782430700 ) ) ;
#5800 = ORIENTED_EDGE ( 'NONE', *, *, #30256, .T. ) ;
#5801 = EDGE_LOOP ( 'NONE', ( #16858, #5133, #14904, #5772 ) ) ;
#5802 = CARTESIAN_POINT ( 'NONE',  ( 158.6250000000000568, 0.000000000000000000, -6.000000000000005329 ) ) ;
#5803 = CARTESIAN_POINT ( 'NONE',  ( -7.216878364870328078, 0.000000000000000000, -139.5580127018922099 ) ) ;
#5804 = ORIENTED_EDGE ( 'NONE', *, *, #1779, .F. ) ;
#5805 = AXIS2_PLACEMENT_3D ( 'NONE', #29981, #29829, #27663 ) ;
#5806 = CARTESIAN_POINT ( 'NONE',  ( 5.412658773652739619, 3.124999999999988898, -130.3169872981078186 ) ) ;
#5807 = CARTESIAN_POINT ( 'NONE',  ( 3.175426480543072749, -5.500000000000105693, -171.6250000000000284 ) ) ;
#5808 = CARTESIAN_POINT ( 'NONE',  ( -5.999999999999963585, 8.134310703387671600E-14, -130.4136751345948539 ) ) ;
#5809 = EDGE_LOOP ( 'NONE', ( #12518, #15049, #23957, #17991 ) ) ;
#5810 = CARTESIAN_POINT ( 'NONE',  ( 15.49999999999998579, -1.999999999999835243, 0.000000000000000000 ) ) ;
#5811 = CARTESIAN_POINT ( 'NONE',  ( 0.07037525868249273897, -16.32901554376975994, -6.302134984203353163 ) ) ;
#5812 = CARTESIAN_POINT ( 'NONE',  ( 5.999999999999988454, 1.607695154586737729, -164.0966878364870070 ) ) ;
#5813 = DIRECTION ( 'NONE',  ( 1.000000000000000000, -0.000000000000000000, -0.000000000000000000 ) ) ;
#5814 = CARTESIAN_POINT ( 'NONE',  ( -5.999999999999963585, 1.780251999655701777E-13, -89.91367513459485394 ) ) ;
#5815 = CARTESIAN_POINT ( 'NONE',  ( 3.464101615137757051, -5.999999999999979572, -107.4136751345947971 ) ) ;
#5816 = CARTESIAN_POINT ( 'NONE',  ( -5.999999999999963585, 1.780251999655701777E-13, -47.33632486540523132 ) ) ;
#5817 = CARTESIAN_POINT ( 'NONE',  ( -5.412658773652684552, -3.125000000000099920, -71.06698729810784698 ) ) ;
#5818 = CARTESIAN_POINT ( 'NONE',  ( -5.412658773652684552, -3.125000000000099920, -54.56698729810782567 ) ) ;
#5819 = EDGE_CURVE ( 'NONE', #2096, #5313, #11307, .T. ) ;
#5820 =( NAMED_UNIT ( * ) SI_UNIT ( $, .STERADIAN. ) SOLID_ANGLE_UNIT ( ) );
#5821 = CARTESIAN_POINT ( 'NONE',  ( 119.9999999999997584, 0.8621349162983860115, -2.008502556962187491 ) ) ;
#5822 = CYLINDRICAL_SURFACE ( 'NONE', #17218, 0.5000000000000004441 ) ;
#5823 = CARTESIAN_POINT ( 'NONE',  ( 3.175426480543072749, 5.499999999999865885, -127.6249999999999858 ) ) ;
#5824 = CYLINDRICAL_SURFACE ( 'NONE', #23039, 6.000000000000000888 ) ;
#5825 = CARTESIAN_POINT ( 'NONE',  ( 104.7401757384973138, -0.4781124843705381045, -1.791203832787282790 ) ) ;
#5826 = ORIENTED_EDGE ( 'NONE', *, *, #3030, .T. ) ;
#5827 = DIRECTION ( 'NONE',  ( -7.147005652999508048E-36, 5.642372883946980038E-36, 1.000000000000000000 ) ) ;
#5828 =( BOUNDED_CURVE ( )  B_SPLINE_CURVE ( 2, ( #18485, #11434, #27200, #4161, #30126, #15588, #6316, #24903, #8947 ),
 .UNSPECIFIED., .F., .F. ) 
 B_SPLINE_CURVE_WITH_KNOTS ( ( 3, 2, 2, 2, 3 ),
 ( 0.4527777777777777790, 0.4537037037037037202, 0.4555555555555555469, 0.4574074074074074292, 0.4583333333333333148 ),
 .UNSPECIFIED. ) 
 CURVE ( )  GEOMETRIC_REPRESENTATION_ITEM ( )  RATIONAL_B_SPLINE_CURVE ( ( 0.9330127018922194093, 0.9330127018922194093, 1.000000000000000000, 0.8660254037844388186, 1.000000000000000000, 0.8660254037844388186, 1.000000000000000000, 0.9330127018922214077, 0.9330127018922194093 ) ) 
 REPRESENTATION_ITEM ( '' )  );
#5829 = CIRCLE ( 'NONE', #25955, 11.00000000000000355 ) ;
#5830 = CARTESIAN_POINT ( 'NONE',  ( 17.78867513459497829, -2.499999999999835687, -2.220446049250313081E-13 ) ) ;
#5831 = CARTESIAN_POINT ( 'NONE',  ( -5.999999999999971578, 1.607695154586715303, -96.90331216351299304 ) ) ;
#5832 = CARTESIAN_POINT ( 'NONE',  ( -6.000000000000007105, -1.607695154586655129, -100.3466878364870496 ) ) ;
#5833 = CARTESIAN_POINT ( 'NONE',  ( 3.464101615137757051, -5.999999999999979572, -144.3363248654052029 ) ) ;
#5834 = EDGE_CURVE ( 'NONE', #11662, #18727, #29261, .T. ) ;
#5835 = ORIENTED_EDGE ( 'NONE', *, *, #3679, .T. ) ;
#5836 = CARTESIAN_POINT ( 'NONE',  ( 111.9997167782376550, -1.308140751793640533, 1.308140751793640533 ) ) ;
#5837 = DIRECTION ( 'NONE',  ( -7.147005652999508048E-36, 5.642372883946980038E-36, 1.000000000000000000 ) ) ;
#5838 = CARTESIAN_POINT ( 'NONE',  ( 10.31249999999998934, -0.8284271247461753029, 1.999999999999911626 ) ) ;
#5839 = CARTESIAN_POINT ( 'NONE',  ( 5.412658773652739619, 3.124999999999988898, -94.31698729810783277 ) ) ;
#5840 = CARTESIAN_POINT ( 'NONE',  ( 6.000000000000000888, -1.607695154586752384, -54.15331216351300014 ) ) ;
#5841 = DIRECTION ( 'NONE',  ( -1.000000000000000000, -0.000000000000000000, 0.000000000000000000 ) ) ;
#5842 = CARTESIAN_POINT ( 'NONE',  ( 112.4374999999998010, -2.499999999999934719, 1.035533905932989551 ) ) ;
#5843 = CYLINDRICAL_SURFACE ( 'NONE', #21353, 6.000000000000000888 ) ;
#5844 = ORIENTED_EDGE ( 'NONE', *, *, #22214, .T. ) ;
#5845 = CARTESIAN_POINT ( 'NONE',  ( 159.6346307794920563, -11.11465906960594552, 4.524012694217853792 ) ) ;
#5846 = DIRECTION ( 'NONE',  ( 0.000000000000000000, -5.551115123125767911E-17, 1.000000000000000000 ) ) ;
#5847 = VECTOR ( 'NONE', #22516, 1000.000000000000000 ) ;
#5848 = CARTESIAN_POINT ( 'NONE',  ( 140.6324251345948824, -5.500000000000012434, -2.278174593052012309 ) ) ;
#5849 = CARTESIAN_POINT ( 'NONE',  ( -39.99999999999998579, -59.99999999999980105, 4.000000000000003553 ) ) ;
#5850 = CARTESIAN_POINT ( 'NONE',  ( -7.216878364870328078, 0.000000000000000000, -73.55801270189223828 ) ) ;
#5851 = CARTESIAN_POINT ( 'NONE',  ( 150.6636751345948255, 0.000000000000000000, 5.500000000000005329 ) ) ;
#5852 = AXIS2_PLACEMENT_3D ( 'NONE', #906, #2917, #17236 ) ;
#5853 = CARTESIAN_POINT ( 'NONE',  ( 149.7038997308104058, 2.071067811865468400, 4.999999999999989342 ) ) ;
#5854 = CARTESIAN_POINT ( 'NONE',  ( 129.9999999999998010, -89.00000000000001421, -3.000000000000002665 ) ) ;
#5855 = PRESENTATION_STYLE_ASSIGNMENT (( #20173 ) ) ;
#5856 = AXIS2_PLACEMENT_3D ( 'NONE', #623, #11898, #28707 ) ;
#5857 = EDGE_CURVE ( 'NONE', #26328, #11541, #4184, .T. ) ;
#5858 =( NAMED_UNIT ( * ) PLANE_ANGLE_UNIT ( ) SI_UNIT ( $, .RADIAN. ) );
#5859 = CARTESIAN_POINT ( 'NONE',  ( -6.350852961085760029, -1.281975124255709124E-13, -136.1250000000000568 ) ) ;
#5860 = CARTESIAN_POINT ( 'NONE',  ( 2.081668171172167281E-16, 3.582034040661430693E-16, -2.499999999999999112 ) ) ;
#5861 = CARTESIAN_POINT ( 'NONE',  ( 5.196152422706629359, 3.000000000000002665, -101.9613248654052171 ) ) ;
#5862 = ORIENTED_EDGE ( 'NONE', *, *, #5654, .F. ) ;
#5863 = CARTESIAN_POINT ( 'NONE',  ( -6.350852961085760029, -1.281975124255709124E-13, -59.62500000000000000 ) ) ;
#5864 = EDGE_CURVE ( 'NONE', #21338, #30043, #6962, .T. ) ;
#5865 = CARTESIAN_POINT ( 'NONE',  ( 0.000000000000000000, 5.499999999999991118, -55.49999999999999289 ) ) ;
#5866 =( BOUNDED_CURVE ( )  B_SPLINE_CURVE ( 2, ( #20360, #8374, #8207, #13333, #17623, #18084, #6070, #8846, #11164 ),
 .UNSPECIFIED., .F., .T. ) 
 B_SPLINE_CURVE_WITH_KNOTS ( ( 3, 2, 2, 2, 3 ),
 ( 0.7083333333333333703, 0.7092592592592592560, 0.7111111111111111382, 0.7129629629629630205, 0.7138888888888887951 ),
 .UNSPECIFIED. ) 
 CURVE ( )  GEOMETRIC_REPRESENTATION_ITEM ( )  RATIONAL_B_SPLINE_CURVE ( ( 0.9330127018922194093, 0.9330127018922194093, 1.000000000000000000, 0.8660254037844388186, 1.000000000000000000, 0.8660254037844388186, 1.000000000000000000, 0.9330127018922274029, 0.9330127018922194093 ) ) 
 REPRESENTATION_ITEM ( '' )  );
#5867 = CYLINDRICAL_SURFACE ( 'NONE', #22417, 2.000000000000012879 ) ;
#5868 = ORIENTED_EDGE ( 'NONE', *, *, #12748, .F. ) ;
#5869 = CARTESIAN_POINT ( 'NONE',  ( 144.0937500000000284, 6.000000000000005329, 2.485281374238585972 ) ) ;
#5870 = CARTESIAN_POINT ( 'NONE',  ( 141.8511751345948255, -3.889087296526011706, 3.889087296526011706 ) ) ;
#5871 = CARTESIAN_POINT ( 'NONE',  ( 6.000000000000000888, -1.607695154586752384, -88.65331216351300725 ) ) ;
#5872 = CARTESIAN_POINT ( 'NONE',  ( 113.6247167782374987, 1.849990392679551343, 0.000000000000000000 ) ) ;
#5873 =( BOUNDED_CURVE ( )  B_SPLINE_CURVE ( 2, ( #29952, #14186, #18927, #4608, #160, #25183, #2466, #22909, #23524 ),
 .UNSPECIFIED., .F., .T. ) 
 B_SPLINE_CURVE_WITH_KNOTS ( ( 3, 2, 2, 2, 3 ),
 ( 0.1176470588235294101, 0.1250000000000000000, 0.1323529411764705899, 0.1397058823529411797, 0.1470588235294117696 ),
 .UNSPECIFIED. ) 
 CURVE ( )  GEOMETRIC_REPRESENTATION_ITEM ( )  RATIONAL_B_SPLINE_CURVE ( ( 1.000000000000000000, 0.9238795325112867385, 1.000000000000000000, 0.9238795325112867385, 1.000000000000000000, 0.9238795325112867385, 1.000000000000000000, 0.9238795325112867385, 1.000000000000000000 ) ) 
 REPRESENTATION_ITEM ( '' )  );
#5874 = EDGE_LOOP ( 'NONE', ( #19766, #26472 ) ) ;
#5875 = AXIS2_PLACEMENT_3D ( 'NONE', #13548, #1830, #24561 ) ;
#5876 = CARTESIAN_POINT ( 'NONE',  ( 146.3437500000000568, -6.000000000000005329, -2.485281374238555774 ) ) ;
#5877 = CARTESIAN_POINT ( 'NONE',  ( 161.2383870809328528, -4.478016635995236250, 3.602319577417127050 ) ) ;
#5878 = ORIENTED_EDGE ( 'NONE', *, *, #17363, .T. ) ;
#5879 = CARTESIAN_POINT ( 'NONE',  ( -4.763139720814407951, -2.750000000000016431, -149.5000000000000284 ) ) ;
#5880 = CARTESIAN_POINT ( 'NONE',  ( 18.00000000000012790, 2.000000000000112799, 0.000000000000000000 ) ) ;
#5881 = EDGE_LOOP ( 'NONE', ( #21804, #22423, #18656, #19364 ) ) ;
#5882 = CARTESIAN_POINT ( 'NONE',  ( 3.608439182435180470, 6.249999999999982236, -148.1919872981077901 ) ) ;
#5883 = CARTESIAN_POINT ( 'NONE',  ( -2.775557561562891351E-14, -5.500000000000115463, -71.25000000000002842 ) ) ;
#5884 = CARTESIAN_POINT ( 'NONE',  ( 2.775557561562891351E-14, -6.250000000000061284, -94.18301270189222407 ) ) ;
#5885 = ORIENTED_EDGE ( 'NONE', *, *, #24185, .F. ) ;
#5886 = CARTESIAN_POINT ( 'NONE',  ( 0.000000000000000000, -5.999999999999991118, -127.9613248654052313 ) ) ;
#5887 = EDGE_CURVE ( 'NONE', #16367, #8576, #11469, .T. ) ;
#5888 = CARTESIAN_POINT ( 'NONE',  ( 5.196152422706629359, -2.999999999999988898, -96.21132486540523132 ) ) ;
#5889 = CARTESIAN_POINT ( 'NONE',  ( -6.000000000000000888, 1.067854986875958443E-15, 7.560779664488942560E-35 ) ) ;
#5890 = PRESENTATION_LAYER_ASSIGNMENT (  '', '', ( #28458 ) ) ;
#5891 = CARTESIAN_POINT ( 'NONE',  ( 110.3511751345946266, 2.000000000000122125, 0.8284271247462955401 ) ) ;
#5892 = CARTESIAN_POINT ( 'NONE',  ( 4.763139720814407951, -2.749999999999988454, -158.0000000000000284 ) ) ;
#5893 = DIRECTION ( 'NONE',  ( -7.147005652999508048E-36, 5.642372883946980038E-36, 1.000000000000000000 ) ) ;
#5894 = CARTESIAN_POINT ( 'NONE',  ( -4.763139720814407951, 2.749999999999946709, -145.2500000000000000 ) ) ;
#5895 = CARTESIAN_POINT ( 'NONE',  ( -3.606777763894024602, 4.527305315996938972, -180.0000000000000853 ) ) ;
#5896 = CARTESIAN_POINT ( 'NONE',  ( -5.999999999999956479, -1.607695154586745057, -92.84668783648702117 ) ) ;
#5897 = CARTESIAN_POINT ( 'NONE',  ( -6.350852961085760029, -1.281975124255709124E-13, -83.62499999999997158 ) ) ;
#5898 = CARTESIAN_POINT ( 'NONE',  ( 104.7401757384973138, 1.387249626875697306, 1.223929297688219897 ) ) ;
#5899 = CYLINDRICAL_SURFACE ( 'NONE', #15788, 5.500000000000000000 ) ;
#5900 = ADVANCED_FACE ( 'NONE', ( #28589 ), #26295, .F. ) ;
#5901 = CARTESIAN_POINT ( 'NONE',  ( -6.350852961085760029, -1.281975124255709124E-13, -80.62500000000004263 ) ) ;
#5902 = CIRCLE ( 'NONE', #1507, 6.000000000000000888 ) ;
#5903 = FACE_OUTER_BOUND ( 'NONE', #26428, .T. ) ;
#5904 = CARTESIAN_POINT ( 'NONE',  ( 151.6949251345948255, 5.500000000000012434, -2.278174593052012309 ) ) ;
#5905 = CARTESIAN_POINT ( 'NONE',  ( -5.196152422706601826, 2.999999999999975131, -103.5386751345947971 ) ) ;
#5906 = CARTESIAN_POINT ( 'NONE',  ( 22.68750000000017764, -0.8284271247460552878, -2.000000000000031530 ) ) ;
#5907 = CARTESIAN_POINT ( 'NONE',  ( 19.96132486540530593, 5.551115123125782702E-14, 2.500000000000002220 ) ) ;
#5908 = DIRECTION ( 'NONE',  ( -0.000000000000000000, -1.000000000000000000, 0.000000000000000000 ) ) ;
#5909 = CARTESIAN_POINT ( 'NONE',  ( 19.99999999999998934, 0.000000000000000000, 0.000000000000000000 ) ) ;
#5910 = ORIENTED_EDGE ( 'NONE', *, *, #4807, .T. ) ;
#5911 = CARTESIAN_POINT ( 'NONE',  ( 159.9375000000000284, -4.242640687119298093, -4.242640687119298093 ) ) ;
#5912 = FACE_OUTER_BOUND ( 'NONE', #16925, .T. ) ;
#5913 = CARTESIAN_POINT ( 'NONE',  ( 118.5627832217621034, 0.7662911109077087390, 1.849990392679772278 ) ) ;
#5914 = AXIS2_PLACEMENT_3D ( 'NONE', #7716, #24445, #24156 ) ;
#5915 = CARTESIAN_POINT ( 'NONE',  ( 5.196152422706629359, -2.999999999999988898, -115.7113248654052455 ) ) ;
#5916 = EDGE_LOOP ( 'NONE', ( #5968, #1938, #14192, #20015 ) ) ;
#5917 = AXIS2_PLACEMENT_3D ( 'NONE', #23911, #5148, #25905 ) ;
#5918 =( GEOMETRIC_REPRESENTATION_CONTEXT ( 3 ) GLOBAL_UNCERTAINTY_ASSIGNED_CONTEXT ( ( #26215 ) ) GLOBAL_UNIT_ASSIGNED_CONTEXT ( ( #8737, #30223, #4575 ) ) REPRESENTATION_CONTEXT ( 'NONE', 'WORKASPACE' ) );
#5919 = UNCERTAINTY_MEASURE_WITH_UNIT (LENGTH_MEASURE( 1.000000000000000082E-05 ), #21653, 'distance_accuracy_value', 'NONE');
#5920 = VERTEX_POINT ( 'NONE', #5094 ) ;
#5921 = CARTESIAN_POINT ( 'NONE',  ( 6.350852961086080661, -9.614813431917819062E-14, -94.87500000000004263 ) ) ;
#5922 = CARTESIAN_POINT ( 'NONE',  ( 2.081668171172167281E-16, 3.582034040661430693E-16, -2.499999999999999112 ) ) ;
#5923 = CARTESIAN_POINT ( 'NONE',  ( -5.412658773652684552, -3.125000000000099920, -112.4330127018922099 ) ) ;
#5924 = ORIENTED_EDGE ( 'NONE', *, *, #26577, .T. ) ;
#5925 = CARTESIAN_POINT ( 'NONE',  ( -5.999999999999963585, 1.780251999655701777E-13, -91.41367513459486815 ) ) ;
#5926 = DIRECTION ( 'NONE',  ( -7.147005652999508048E-36, 5.642372883946980038E-36, 1.000000000000000000 ) ) ;
#5927 = AXIS2_PLACEMENT_3D ( 'NONE', #29176, #10634, #19983 ) ;
#5928 = EDGE_CURVE ( 'NONE', #2252, #2328, #27800, .T. ) ;
#5929 = CARTESIAN_POINT ( 'NONE',  ( -5.412658773652739619, 3.124999999999975131, -49.68301270189223828 ) ) ;
#5930 = EDGE_LOOP ( 'NONE', ( #8625, #11809, #727, #4548 ) ) ;
#5931 = CARTESIAN_POINT ( 'NONE',  ( 0.000000000000000000, 5.999999999999977796, -153.2886751345948824 ) ) ;
#5932 = ADVANCED_FACE ( 'NONE', ( #21714 ), #5250, .T. ) ;
#5933 = DIRECTION ( 'NONE',  ( 1.000000000000000000, -0.000000000000000000, -0.000000000000000000 ) ) ;
#5934 = CARTESIAN_POINT ( 'NONE',  ( 3.464101615137757051, -5.999999999999979572, -61.83632486540521001 ) ) ;
#5935 = CARTESIAN_POINT ( 'NONE',  ( 155.5238248654052313, 3.889087296526011706, -3.889087296526011706 ) ) ;
#5936 = CARTESIAN_POINT ( 'NONE',  ( -6.350852961085760029, -1.281975124255709124E-13, -169.1249999999999716 ) ) ;
#5937 = CARTESIAN_POINT ( 'NONE',  ( 119.2499999999999574, -5.551115123125782702E-14, 2.500000000000168754 ) ) ;
#5938 = CARTESIAN_POINT ( 'NONE',  ( 119.9999999999999574, -0.4876318259219858398, 1.939643060552387333 ) ) ;
#5939 = CARTESIAN_POINT ( 'NONE',  ( -5.412658773652739619, 3.124999999999975131, -169.6830127018922383 ) ) ;
#5940 = CARTESIAN_POINT ( 'NONE',  ( -1.000000000000002665, -9.000000000000007105, 4.000000000000005329 ) ) ;
#5941 = AXIS2_PLACEMENT_3D ( 'NONE', #26812, #22392, #29123 ) ;
#5942 = CARTESIAN_POINT ( 'NONE',  ( -4.763139720814407951, -2.750000000000016431, -110.5000000000000426 ) ) ;
#5943 = DIRECTION ( 'NONE',  ( 1.000000000000000000, -0.000000000000000000, -0.000000000000000000 ) ) ;
#5944 = CARTESIAN_POINT ( 'NONE',  ( 3.175426480543072749, -5.500000000000105693, -107.1250000000000284 ) ) ;
#5945 = CARTESIAN_POINT ( 'NONE',  ( -5.999999999999963585, -1.487416814333745711E-14, -87.83632486540521711 ) ) ;
#5946 = CARTESIAN_POINT ( 'NONE',  ( 11.41367513459493033, 1.767766952966487448, 1.767766952966209892 ) ) ;
#5947 = CARTESIAN_POINT ( 'NONE',  ( 135.0000000000000284, -8.296337134229657906, 7.693139387096130655 ) ) ;
#5948 = CIRCLE ( 'NONE', #21679, 28.99999999999999645 ) ;
#5949 = ORIENTED_EDGE ( 'NONE', *, *, #17393, .F. ) ;
#5950 = CARTESIAN_POINT ( 'NONE',  ( 15.56250000000000533, 2.649519052838358757, -1.097466725451739622 ) ) ;
#5951 = CARTESIAN_POINT ( 'NONE',  ( 130.0000000000000284, -60.00000000000001421, -4.000000000000003553 ) ) ;
#5952 = CARTESIAN_POINT ( 'NONE',  ( 161.2500000000000284, -6.000000000000005329, 0.000000000000000000 ) ) ;
#5953 = CARTESIAN_POINT ( 'NONE',  ( 111.7502832217623165, -1.308140751793585022, 1.308140751793862577 ) ) ;
#5954 = AXIS2_PLACEMENT_3D ( 'NONE', #3298, #11719, #11878 ) ;
#5955 = CARTESIAN_POINT ( 'NONE',  ( -3.608439182435052128, -6.250000000000110134, -84.44198729810780435 ) ) ;
#5956 = PRODUCT ( 'MAS-675', 'MAS-675', '', ( #25395 ) ) ;
#5957 = CARTESIAN_POINT ( 'NONE',  ( -3.464101615137757051, -5.999999999999979572, -103.1636751345948397 ) ) ;
#5958 = VERTEX_POINT ( 'NONE', #3094 ) ;
#5959 = DIRECTION ( 'NONE',  ( 1.000000000000000000, -5.551115123125773458E-17, -1.260129944081490338E-35 ) ) ;
#5960 = PRESENTATION_LAYER_ASSIGNMENT (  '', '', ( #14358 ) ) ;
#5961 = ORIENTED_EDGE ( 'NONE', *, *, #13476, .T. ) ;
#5962 = VERTEX_POINT ( 'NONE', #12074 ) ;
#5963 = CARTESIAN_POINT ( 'NONE',  ( 154.7812500000000568, 2.485281374238585972, 6.000000000000005329 ) ) ;
#5964 = AXIS2_PLACEMENT_3D ( 'NONE', #28616, #9920, #10369 ) ;
#5965 = CARTESIAN_POINT ( 'NONE',  ( 0.000000000000000000, 5.499999999999991118, -132.0000000000000000 ) ) ;
#5966 =( BOUNDED_CURVE ( )  B_SPLINE_CURVE ( 2, ( #19753, #5753, #28645, #12726, #26643, #15164, #26495, #12134, #21477 ),
 .UNSPECIFIED., .F., .F. ) 
 B_SPLINE_CURVE_WITH_KNOTS ( ( 3, 2, 2, 2, 3 ),
 ( 0.8083333333333333481, 0.8092592592592592338, 0.8111111111111111160, 0.8129629629629629983, 0.8138888888888888840 ),
 .UNSPECIFIED. ) 
 CURVE ( )  GEOMETRIC_REPRESENTATION_ITEM ( )  RATIONAL_B_SPLINE_CURVE ( ( 0.9330127018922194093, 0.9330127018922194093, 1.000000000000000000, 0.8660254037844388186, 1.000000000000000000, 0.8660254037844388186, 1.000000000000000000, 0.9330127018922194093, 0.9330127018922194093 ) ) 
 REPRESENTATION_ITEM ( '' )  );
#5967 = CARTESIAN_POINT ( 'NONE',  ( 5.412658773652739619, 3.124999999999988898, -141.6830127018922099 ) ) ;
#5968 = ORIENTED_EDGE ( 'NONE', *, *, #610, .T. ) ;
#5969 = CARTESIAN_POINT ( 'NONE',  ( 151.1324251345948255, -5.500000000000012434, -2.278174593052012309 ) ) ;
#5970 = CARTESIAN_POINT ( 'NONE',  ( 2.775557561562891351E-14, -6.250000000000061284, -121.8169872981078612 ) ) ;
#5971 = DIRECTION ( 'NONE',  ( 0.000000000000000000, 0.000000000000000000, -1.000000000000000000 ) ) ;
#5972 = CARTESIAN_POINT ( 'NONE',  ( -3.175426480542816510, 5.499999999999865885, -175.3750000000000568 ) ) ;
#5973 = CIRCLE ( 'NONE', #5004, 1.000000000000000888 ) ;
#5974 = CARTESIAN_POINT ( 'NONE',  ( -6.000000000000000888, 1.067854986875958443E-15, 7.560779664488942560E-35 ) ) ;
#5975 = CARTESIAN_POINT ( 'NONE',  ( 116.0000000000000142, 0.000000000000000000, -5.500000000000000000 ) ) ;
#5976 = EDGE_CURVE ( 'NONE', #2098, #22382, #7333, .T. ) ;
#5977 = ORIENTED_EDGE ( 'NONE', *, *, #18630, .F. ) ;
#5978 = CARTESIAN_POINT ( 'NONE',  ( 16.75000000000015277, 1.665334536937734811E-13, -2.000000000000001776 ) ) ;
#5979 = CARTESIAN_POINT ( 'NONE',  ( 0.7669223171414771834, -15.58766199952933107, -7.954545454545431049 ) ) ;
#5980 = EDGE_CURVE ( 'NONE', #23459, #22223, #28443, .T. ) ;
#5981 = DIRECTION ( 'NONE',  ( 0.000000000000000000, 0.000000000000000000, 1.000000000000000000 ) ) ;
#5982 = CARTESIAN_POINT ( 'NONE',  ( 5.196152422706629359, -2.999999999999988898, -107.2886751345948397 ) ) ;
#5983 = CARTESIAN_POINT ( 'NONE',  ( 0.8032275580764794976, -15.44744712271809739, -8.223858897419269454 ) ) ;
#5984 = CARTESIAN_POINT ( 'NONE',  ( 116.7502832217622171, -1.308140751793529510, 1.308140751793640533 ) ) ;
#5985 = CARTESIAN_POINT ( 'NONE',  ( 7.216878364870455975, -6.409875621278545621E-14, -64.44198729810784698 ) ) ;
#5986 = CARTESIAN_POINT ( 'NONE',  ( 5.412658773652712085, -3.125000000000086153, -54.06698729810782567 ) ) ;
#5987 = CARTESIAN_POINT ( 'NONE',  ( -39.00000000000000000, -20.00000000000021316, -3.000000000000002665 ) ) ;
#5988 = CARTESIAN_POINT ( 'NONE',  ( 6.000000000000026645, -1.607695154586707753, -128.2306624327026157 ) ) ;
#5989 = CARTESIAN_POINT ( 'NONE',  ( -9.999999999999994671, -9.000000000000007105, 4.000000000000003553 ) ) ;
#5990 = LINE ( 'NONE', #8286, #19631 ) ;
#5991 = CARTESIAN_POINT ( 'NONE',  ( 3.175426480543072749, 5.499999999999865885, -129.1250000000000284 ) ) ;
#5992 = ORIENTED_EDGE ( 'NONE', *, *, #1889, .F. ) ;
#5993 = CARTESIAN_POINT ( 'NONE',  ( -3.464101615137725076, 5.999999999999979572, -157.6636751345948255 ) ) ;
#5994 = FACE_OUTER_BOUND ( 'NONE', #5376, .T. ) ;
#5995 = CARTESIAN_POINT ( 'NONE',  ( 16.64882486540528106, 2.500000000000205169, -1.035533905932809473 ) ) ;
#5996 = DIRECTION ( 'NONE',  ( -7.147005652999508048E-36, 5.642372883946980038E-36, 1.000000000000000000 ) ) ;
#5997 = VERTEX_POINT ( 'NONE', #7113 ) ;
#5998 = CARTESIAN_POINT ( 'NONE',  ( 113.1872167782373992, -1.849990392679441875, -0.7662911109075883909 ) ) ;
#5999 = DIRECTION ( 'NONE',  ( -7.147005652999508048E-36, 5.642372883946980038E-36, 1.000000000000000000 ) ) ;
#6000 = CARTESIAN_POINT ( 'NONE',  ( 11.18750000000003908, 0.8284271247462955401, 2.000000000000031530 ) ) ;
#6001 = CARTESIAN_POINT ( 'NONE',  ( -3.608439182435115633, 6.249999999999965361, -113.4419872981078328 ) ) ;
#6002 = CARTESIAN_POINT ( 'NONE',  ( -5.999999999999962697, -1.607695154586733954, -173.8466878364870354 ) ) ;
#6003 = CARTESIAN_POINT ( 'NONE',  ( -5.999999999999963585, 1.780251999655701777E-13, -90.83632486540521711 ) ) ;
#6004 = CARTESIAN_POINT ( 'NONE',  ( 114.4374999999998010, -2.499999999999964473, 1.035533905932929599 ) ) ;
#6005 = ORIENTED_EDGE ( 'NONE', *, *, #11079, .F. ) ;
#6006 = CARTESIAN_POINT ( 'NONE',  ( 138.1949251345948255, 5.500000000000012434, -2.278174593052012309 ) ) ;
#6007 = EDGE_CURVE ( 'NONE', #16120, #24823, #8304, .T. ) ;
#6008 = CARTESIAN_POINT ( 'NONE',  ( 139.9687500000000284, -2.485281374238585972, 6.000000000000005329 ) ) ;
#6009 = CARTESIAN_POINT ( 'NONE',  ( 9.500000000000008882, -1.999999999999835243, 0.000000000000000000 ) ) ;
#6010 = CARTESIAN_POINT ( 'NONE',  ( 136.3050748654052882, 5.500000000000012434, 2.278174593052012309 ) ) ;
#6011 = CARTESIAN_POINT ( 'NONE',  ( 3.175426480543072749, -5.500000000000105693, -47.12500000000006395 ) ) ;
#6012 = CARTESIAN_POINT ( 'NONE',  ( 136.9761751345948539, 3.889087296526011706, 3.889087296526011706 ) ) ;
#6013 = CARTESIAN_POINT ( 'NONE',  ( 0.000000000000000000, 0.000000000000000000, 0.000000000000000000 ) ) ;
#6014 = CARTESIAN_POINT ( 'NONE',  ( -5.999999999999963585, -1.487416814333745711E-14, -80.33632486540523132 ) ) ;
#6015 = CARTESIAN_POINT ( 'NONE',  ( 5.412658773652712085, -3.125000000000086153, -77.43301270189223828 ) ) ;
#6016 = EDGE_CURVE ( 'NONE', #21299, #1154, #3997, .T. ) ;
#6017 = CARTESIAN_POINT ( 'NONE',  ( 116.5238248654049471, 0.8284271247462654530, -1.999999999999851674 ) ) ;
#6018 = VECTOR ( 'NONE', #4063, 1000.000000000000000 ) ;
#6019 = CARTESIAN_POINT ( 'NONE',  ( 148.9538997308104342, -2.071067811865468400, -4.999999999999989342 ) ) ;
#6020 = CARTESIAN_POINT ( 'NONE',  ( 5.999999999999993783, 1.607695154586726627, -177.5966878364870070 ) ) ;
#6021 = CARTESIAN_POINT ( 'NONE',  ( -5.999999999999963585, 1.780251999655701777E-13, -99.83632486540521711 ) ) ;
#6022 = CARTESIAN_POINT ( 'NONE',  ( 6.000000000000000888, 1.607695154586715303, -105.0193375672974554 ) ) ;
#6023 = CARTESIAN_POINT ( 'NONE',  ( 4.763139720814407951, -2.749999999999988454, -131.0000000000000000 ) ) ;
#6024 = CARTESIAN_POINT ( 'NONE',  ( 105.7886751345946550, -1.999999999999946265, 0.000000000000000000 ) ) ;
#6025 = FACE_OUTER_BOUND ( 'NONE', #13686, .T. ) ;
#6026 = CARTESIAN_POINT ( 'NONE',  ( 0.000000000000000000, 5.999999999999977796, -178.2113248654052597 ) ) ;
#6027 = EDGE_LOOP ( 'NONE', ( #12549, #12007, #25159, #342 ) ) ;
#6028 = CARTESIAN_POINT ( 'NONE',  ( -3.175426480542816066, 5.499999999999865885, -65.87500000000002842 ) ) ;
#6029 = CARTESIAN_POINT ( 'NONE',  ( -3.175426480542816510, 5.499999999999865885, -55.37500000000004263 ) ) ;
#6030 = CARTESIAN_POINT ( 'NONE',  ( 3.464101615137852974, 5.999999999999884537, -170.8363248654052029 ) ) ;
#6031 = VERTEX_POINT ( 'NONE', #19263 ) ;
#6032 = CARTESIAN_POINT ( 'NONE',  ( 107.7499999999998579, 5.551115123125782702E-14, -2.499999999999946709 ) ) ;
#6033 = CARTESIAN_POINT ( 'NONE',  ( 143.6250000000000284, 0.000000000000000000, -6.000000000000005329 ) ) ;
#6034 = FACE_OUTER_BOUND ( 'NONE', #27641, .T. ) ;
#6035 = CARTESIAN_POINT ( 'NONE',  ( 14.31250000000002132, -0.8284271247461152399, 2.000000000000151879 ) ) ;
#6036 =( NAMED_UNIT ( * ) PLANE_ANGLE_UNIT ( ) SI_UNIT ( $, .RADIAN. ) );
#6037 = AXIS2_PLACEMENT_3D ( 'NONE', #19171, #5007, #2705 ) ;
#6038 = EDGE_LOOP ( 'NONE', ( #30235, #7805, #24541, #27449 ) ) ;
#6039 = CARTESIAN_POINT ( 'NONE',  ( 145.6875000000000284, 4.242640687119269671, 4.242640687119298093 ) ) ;
#6040 = CARTESIAN_POINT ( 'NONE',  ( 143.2425748654052313, -2.278174593052290753, -5.499999999999732658 ) ) ;
#6041 = ADVANCED_FACE ( 'NONE', ( #7556 ), #13628, .T. ) ;
#6042 = AXIS2_PLACEMENT_3D ( 'NONE', #1295, #22208, #19898 ) ;
#6043 = ORIENTED_EDGE ( 'NONE', *, *, #22963, .F. ) ;
#6044 = EDGE_CURVE ( 'NONE', #12501, #19344, #852, .T. ) ;
#6045 = CARTESIAN_POINT ( 'NONE',  ( -3.175426480542816510, 5.499999999999865885, -146.8750000000000284 ) ) ;
#6046 = VERTEX_POINT ( 'NONE', #10651 ) ;
#6047 = CARTESIAN_POINT ( 'NONE',  ( 18.50000000000012790, -1.999999999999835243, 0.000000000000000000 ) ) ;
#6048 = ORIENTED_EDGE ( 'NONE', *, *, #5976, .F. ) ;
#6049 = CARTESIAN_POINT ( 'NONE',  ( 4.763139720814407951, 2.750000000000002665, -76.74999999999998579 ) ) ;
#6050 = CARTESIAN_POINT ( 'NONE',  ( 13.75000000000003908, -1.873492889144900975, 1.873492889144734441 ) ) ;
#6051 = EDGE_CURVE ( 'NONE', #19511, #3951, #6165, .T. ) ;
#6052 = CARTESIAN_POINT ( 'NONE',  ( 7.216878364870455975, -6.409875621278545621E-14, -92.30801270189225249 ) ) ;
#6053 = EDGE_CURVE ( 'NONE', #16791, #13814, #17419, .T. ) ;
#6054 = DIRECTION ( 'NONE',  ( 1.000000000000000000, 1.665334536937735797E-16, 0.000000000000000000 ) ) ;
#6055 = DIRECTION ( 'NONE',  ( -1.000000000000000000, -1.665334536937731113E-16, 1.526556658859586792E-16 ) ) ;
#6056 = DIRECTION ( 'NONE',  ( -7.147005652999508048E-36, 5.642372883946980038E-36, 1.000000000000000000 ) ) ;
#6057 = CARTESIAN_POINT ( 'NONE',  ( 0.000000000000000000, -5.999999999999991118, -91.03867513459485394 ) ) ;
#6058 = CARTESIAN_POINT ( 'NONE',  ( 24.51662501065472100, 0.2042826450495058288, 2.483374989345329187 ) ) ;
#6059 = SHAPE_DEFINITION_REPRESENTATION ( #8682, #15661 ) ;
#6060 =( BOUNDED_CURVE ( )  B_SPLINE_CURVE ( 2, ( #26350, #29094, #5599, #5299, #3296, #14712, #24055, #12421, #17784 ),
 .UNSPECIFIED., .F., .T. ) 
 B_SPLINE_CURVE_WITH_KNOTS ( ( 3, 2, 2, 2, 3 ),
 ( 0.8638888888888889284, 0.8648148148148148140, 0.8666666666666666963, 0.8685185185185184675, 0.8694444444444443532 ),
 .UNSPECIFIED. ) 
 CURVE ( )  GEOMETRIC_REPRESENTATION_ITEM ( )  RATIONAL_B_SPLINE_CURVE ( ( 0.9330127018922194093, 0.9330127018922234061, 1.000000000000000000, 0.8660254037844388186, 1.000000000000000000, 0.8660254037844388186, 1.000000000000000000, 0.9330127018922234061, 0.9330127018922194093 ) ) 
 REPRESENTATION_ITEM ( '' )  );
#6061 = CARTESIAN_POINT ( 'NONE',  ( -4.763139720814407951, 2.749999999999946709, -155.7500000000000568 ) ) ;
#6062 = CYLINDRICAL_SURFACE ( 'NONE', #766, 6.000000000000000888 ) ;
#6063 = AXIS2_PLACEMENT_3D ( 'NONE', #25528, #6649, #16068 ) ;
#6064 = DIRECTION ( 'NONE',  ( -7.147005652999508048E-36, 5.642372883946980038E-36, 1.000000000000000000 ) ) ;
#6065 = UNCERTAINTY_MEASURE_WITH_UNIT (LENGTH_MEASURE( 1.000000000000000082E-05 ), #12500, 'distance_accuracy_value', 'NONE');
#6066 = CARTESIAN_POINT ( 'NONE',  ( -2.775557561562891351E-14, -5.500000000000115463, -87.75000000000000000 ) ) ;
#6067 = CARTESIAN_POINT ( 'NONE',  ( 104.6247167782375271, 1.849990392679523588, 0.000000000000000000 ) ) ;
#6068 = CARTESIAN_POINT ( 'NONE',  ( 3.175426480543072749, -5.500000000000105693, -83.12500000000004263 ) ) ;
#6069 = CARTESIAN_POINT ( 'NONE',  ( 153.5773502691896510, 5.000000000000004441, 0.000000000000000000 ) ) ;
#6070 = CARTESIAN_POINT ( 'NONE',  ( 5.196152422706629359, 3.000000000000002665, -142.4613248654052029 ) ) ;
#6071 = CARTESIAN_POINT ( 'NONE',  ( 112.2886751345947118, 2.000000000000112799, 3.330669073875469621E-13 ) ) ;
#6072 = DIRECTION ( 'NONE',  ( 0.000000000000000000, 0.000000000000000000, -1.000000000000000000 ) ) ;
#6073 = CARTESIAN_POINT ( 'NONE',  ( -5.196152422706601826, 2.999999999999975131, -124.5386751345948255 ) ) ;
#6074 = CARTESIAN_POINT ( 'NONE',  ( 6.000000000000000888, 7.762456499804235646E-14, -123.0863248654052313 ) ) ;
#6075 = DIRECTION ( 'NONE',  ( -7.147005652999508048E-36, 5.642372883946980038E-36, 1.000000000000000000 ) ) ;
#6076 = VERTEX_POINT ( 'NONE', #1404 ) ;
#6077 = CARTESIAN_POINT ( 'NONE',  ( 159.7500000000000284, -6.000000000000005329, 0.000000000000000000 ) ) ;
#6078 = CARTESIAN_POINT ( 'NONE',  ( -4.999999999999990230, -24.99999999999999289, 8.000000000000007105 ) ) ;
#6079 = CARTESIAN_POINT ( 'NONE',  ( 145.4136751345948539, 0.000000000000000000, -5.500000000000005329 ) ) ;
#6080 = CARTESIAN_POINT ( 'NONE',  ( 118.1252832217622881, -2.775557561562891351E-14, -1.849990392679523588 ) ) ;
#6081 = EDGE_CURVE ( 'NONE', #4935, #25253, #2832, .T. ) ;
#6082 = ORIENTED_EDGE ( 'NONE', *, *, #15662, .T. ) ;
#6083 = CARTESIAN_POINT ( 'NONE',  ( -4.763139720814407951, -2.750000000000016431, -100.0000000000000284 ) ) ;
#6084 = AXIS2_PLACEMENT_3D ( 'NONE', #23848, #2936, #28430 ) ;
#6085 = CARTESIAN_POINT ( 'NONE',  ( 16.50000000000015277, 1.873492889145067508, 1.873492889144734441 ) ) ;
#6086 = DIRECTION ( 'NONE',  ( 5.551115123125785167E-17, -1.000000000000000000, -8.881784197001256268E-16 ) ) ;
#6087 = EDGE_CURVE ( 'NONE', #2251, #5496, #7148, .T. ) ;
#6088 = CARTESIAN_POINT ( 'NONE',  ( 5.412658773652739619, 3.124999999999988898, -117.6830127018922383 ) ) ;
#6089 = ADVANCED_FACE ( 'NONE', ( #940 ), #13156, .F. ) ;
#6090 = ORIENTED_EDGE ( 'NONE', *, *, #21156, .T. ) ;
#6091 = CARTESIAN_POINT ( 'NONE',  ( 3.464101615137852974, 5.999999999999884537, -94.33632486540517448 ) ) ;
#6092 = CARTESIAN_POINT ( 'NONE',  ( 6.000000000000000888, -3.330669073875464691E-16, -7.560779664488942560E-35 ) ) ;
#6093 = CARTESIAN_POINT ( 'NONE',  ( -5.999999999999963585, 1.780251999655701777E-13, -62.91367513459483973 ) ) ;
#6094 = CARTESIAN_POINT ( 'NONE',  ( 2.775557561562891351E-14, 6.250000000000033751, -55.93301270189221697 ) ) ;
#6095 = ORIENTED_EDGE ( 'NONE', *, *, #18510, .T. ) ;
#6096 = DIRECTION ( 'NONE',  ( 1.000000000000000000, -0.000000000000000000, -0.000000000000000000 ) ) ;
#6097 = LINE ( 'NONE', #29429, #10922 ) ;
#6098 = DIRECTION ( 'NONE',  ( -8.326672684688675286E-17, -2.081668171172168821E-17, 1.000000000000000000 ) ) ;
#6099 = CARTESIAN_POINT ( 'NONE',  ( 0.9868033348211120437, -16.18260772123499081, -6.670819112052091882 ) ) ;
#6100 = CARTESIAN_POINT ( 'NONE',  ( 3.175426480543072749, -5.500000000000105693, -171.6250000000000284 ) ) ;
#6101 = CARTESIAN_POINT ( 'NONE',  ( 115.8124999999997584, 1.035533905932719101, -2.499999999999784173 ) ) ;
#6102 = CARTESIAN_POINT ( 'NONE',  ( 3.464101615137852974, 5.999999999999884537, -107.8363248654052313 ) ) ;
#6103 = CARTESIAN_POINT ( 'NONE',  ( -7.216878364870328078, 0.000000000000000000, -163.5580127018922099 ) ) ;
#6104 = CARTESIAN_POINT ( 'NONE',  ( -0.05236263670367936190, -9.947637363296344404, 4.619711369386890532 ) ) ;
#6105 = CARTESIAN_POINT ( 'NONE',  ( 3.175426480543072749, 5.499999999999865885, -112.6249999999999858 ) ) ;
#6106 = CARTESIAN_POINT ( 'NONE',  ( 160.2261751345948539, -3.889087296526011706, -3.889087296526011706 ) ) ;
#6107 = CARTESIAN_POINT ( 'NONE',  ( 0.000000000000000000, 5.499999999999991118, -103.5000000000000426 ) ) ;
#6108 = CARTESIAN_POINT ( 'NONE',  ( 5.196152422706629359, -2.999999999999988898, -111.7886751345948397 ) ) ;
#6109 = CARTESIAN_POINT ( 'NONE',  ( 141.2886751345948539, 5.500000000000005329, 0.000000000000000000 ) ) ;
#6110 = CARTESIAN_POINT ( 'NONE',  ( -5.999999999999971578, 1.607695154586715303, -117.9033121635130072 ) ) ;
#6111 = ORIENTED_EDGE ( 'NONE', *, *, #17010, .F. ) ;
#6112 = CARTESIAN_POINT ( 'NONE',  ( 120.6874999999997584, -1.035533905932719101, -2.499999999999844569 ) ) ;
#6113 = CARTESIAN_POINT ( 'NONE',  ( 110.0002832217622597, -1.308140751793585022, -1.308140751793640533 ) ) ;
#6114 = FACE_OUTER_BOUND ( 'NONE', #7553, .T. ) ;
#6115 = VERTEX_POINT ( 'NONE', #19702 ) ;
#6116 = CARTESIAN_POINT ( 'NONE',  ( 6.350852961086080661, -9.614813431917819062E-14, -157.8750000000000000 ) ) ;
#6117 = CARTESIAN_POINT ( 'NONE',  ( -5.412658773652684552, -3.125000000000099920, -80.06698729810779014 ) ) ;
#6118 = ADVANCED_FACE ( 'NONE', ( #1099 ), #3007, .T. ) ;
#6119 = DIRECTION ( 'NONE',  ( 1.000000000000000000, -0.000000000000000000, -0.000000000000000000 ) ) ;
#6120 = ORIENTED_EDGE ( 'NONE', *, *, #11215, .T. ) ;
#6121 = LINE ( 'NONE', #21962, #27718 ) ;
#6122 = STYLED_ITEM ( 'NONE', ( #6220 ), #17033 ) ;
#6123 = VERTEX_POINT ( 'NONE', #2334 ) ;
#6124 = EDGE_LOOP ( 'NONE', ( #29773, #29411, #4613, #24956 ) ) ;
#6125 = CARTESIAN_POINT ( 'NONE',  ( 155.7187500000000568, 2.485281374238555774, -6.000000000000005329 ) ) ;
#6126 = VECTOR ( 'NONE', #22714, 1000.000000000000000 ) ;
#6127 = CARTESIAN_POINT ( 'NONE',  ( 4.763139720814407951, -2.749999999999988454, -120.5000000000000568 ) ) ;
#6128 = EDGE_CURVE ( 'NONE', #91, #1235, #21227, .T. ) ;
#6129 = CARTESIAN_POINT ( 'NONE',  ( 2.775557561562891351E-14, 6.250000000000033751, -135.4330127018922383 ) ) ;
#6130 = VERTEX_POINT ( 'NONE', #171 ) ;
#6131 = DIRECTION ( 'NONE',  ( 0.000000000000000000, 0.000000000000000000, -1.000000000000000000 ) ) ;
#6132 = CARTESIAN_POINT ( 'NONE',  ( -5.412658773652739619, 3.124999999999975131, -126.8169872981078612 ) ) ;
#6133 = CARTESIAN_POINT ( 'NONE',  ( -5.999999999999963585, 8.134310703387671600E-14, -146.3363248654052313 ) ) ;
#6134 = CARTESIAN_POINT ( 'NONE',  ( -3.175426480542816510, -5.500000000000057732, -170.3750000000000568 ) ) ;
#6135 = CARTESIAN_POINT ( 'NONE',  ( 5.000000000000018652, 8.326672684688674053E-14, 1.110223024625156540E-13 ) ) ;
#6136 = EDGE_LOOP ( 'NONE', ( #24105, #3650, #30260, #28696 ) ) ;
#6137 = CARTESIAN_POINT ( 'NONE',  ( 13.12500000000016342, 1.414213562373145550, 1.414213562373034527 ) ) ;
#6138 = CYLINDRICAL_SURFACE ( 'NONE', #8845, 6.000000000000000888 ) ;
#6140 = VECTOR ( 'NONE', #9996, 1000.000000000000000 ) ;
#6139 = CARTESIAN_POINT ( 'NONE',  ( 160.5991965838383351, -11.35444276374069617, -3.884274201564634765 ) ) ;
#6141 = CARTESIAN_POINT ( 'NONE',  ( 0.000000000000000000, 0.000000000000000000, 0.000000000000000000 ) ) ;
#6142 = CARTESIAN_POINT ( 'NONE',  ( 0.8631338372297875372, -15.37878787878789133, -8.351220472436782671 ) ) ;
#6143 = CARTESIAN_POINT ( 'NONE',  ( 111.3752832217622739, 1.849990392679468076, 0.000000000000000000 ) ) ;
#6144 = CARTESIAN_POINT ( 'NONE',  ( 3.608439182435180470, 6.249999999999982236, -65.69198729810780435 ) ) ;
#6145 = CARTESIAN_POINT ( 'NONE',  ( -6.000000000000000888, 1.067854986875958443E-15, 7.560779664488942560E-35 ) ) ;
#6146 = CARTESIAN_POINT ( 'NONE',  ( 6.000000000000000888, -1.607695154586752384, -63.73066243270262987 ) ) ;
#6147 = CARTESIAN_POINT ( 'NONE',  ( 119.9999999999998721, -0.4876318259425804769, -1.939643060543838615 ) ) ;
#6148 = CARTESIAN_POINT ( 'NONE',  ( -4.999999999999990230, -55.00000000000002132, -5.000000000000004441 ) ) ;
#6149 = CARTESIAN_POINT ( 'NONE',  ( 3.175426480543072749, -5.500000000000105693, -129.6250000000000284 ) ) ;
#6150 = CARTESIAN_POINT ( 'NONE',  ( 104.7401757384972427, 0.5979633189608006827, -1.754835448641252293 ) ) ;
#6151 = ORIENTED_EDGE ( 'NONE', *, *, #10133, .T. ) ;
#6152 = CARTESIAN_POINT ( 'NONE',  ( -5.196152422706573404, -3.000000000000002665, -119.2113248654052029 ) ) ;
#6153 = AXIS2_PLACEMENT_3D ( 'NONE', #25413, #4534, #13490 ) ;
#6154 = CARTESIAN_POINT ( 'NONE',  ( 17.97617513459486105, -1.035533905932568999, -2.499999999999904521 ) ) ;
#6155 = CYLINDRICAL_SURFACE ( 'NONE', #5927, 1.000000000000000000 ) ;
#6156 = CARTESIAN_POINT ( 'NONE',  ( 142.1398502691896510, -3.535533905932752852, 3.535533905932725318 ) ) ;
#6157 = ORIENTED_EDGE ( 'NONE', *, *, #21884, .F. ) ;
#6158 = CARTESIAN_POINT ( 'NONE',  ( 115.0622167782373850, -1.849990392679411677, 0.7662911109078888172 ) ) ;
#6159 = FACE_OUTER_BOUND ( 'NONE', #29428, .T. ) ;
#6160 = CARTESIAN_POINT ( 'NONE',  ( 114.0386751345946834, 1.110223024625156540E-13, -1.999999999999668709 ) ) ;
#6161 = CARTESIAN_POINT ( 'NONE',  ( -3.608439182435052128, -6.250000000000110134, -112.9419872981078186 ) ) ;
#6162 = ADVANCED_FACE ( 'NONE', ( #28260 ), #7239, .T. ) ;
#6163 = CARTESIAN_POINT ( 'NONE',  ( 135.0000000000000284, 3.755552545897461236, -4.233421981095762732 ) ) ;
#6164 = EDGE_CURVE ( 'NONE', #16384, #29310, #685, .T. ) ;
#6165 =( BOUNDED_CURVE ( )  B_SPLINE_CURVE ( 2, ( #12975, #8152, #8476, #6175, #8011, #13129, #6012, #12521, #15267 ),
 .UNSPECIFIED., .F., .T. ) 
 B_SPLINE_CURVE_WITH_KNOTS ( ( 3, 2, 2, 2, 3 ),
 ( 0.1374999999999996780, 0.1437499999999995448, 0.1499999999999992728, 0.1562499999999990008, 0.1624999999999987566 ),
 .UNSPECIFIED. ) 
 CURVE ( )  GEOMETRIC_REPRESENTATION_ITEM ( )  RATIONAL_B_SPLINE_CURVE ( ( 1.000000000000003331, 0.9238795325112834078, 1.000000000000000000, 0.9238795325112867385, 1.000000000000000000, 0.9238795325112867385, 1.000000000000000000, 0.9238795325113016155, 0.9999999999999851230 ) ) 
 REPRESENTATION_ITEM ( '' )  );
#6166 = VECTOR ( 'NONE', #20213, 1000.000000000000000 ) ;
#6167 = CARTESIAN_POINT ( 'NONE',  ( 112.8749999999998437, 1.767766952966320915, -1.767766952966320915 ) ) ;
#6168 = CIRCLE ( 'NONE', #6653, 1.000000000000000888 ) ;
#6169 = ORIENTED_EDGE ( 'NONE', *, *, #5980, .T. ) ;
#6170 = CARTESIAN_POINT ( 'NONE',  ( 137.9136751345948539, 0.000000000000000000, -5.500000000000005329 ) ) ;
#6171 = CARTESIAN_POINT ( 'NONE',  ( 141.5625000000000284, -4.242640687119298093, 4.242640687119298093 ) ) ;
#6172 = ORIENTED_EDGE ( 'NONE', *, *, #9983, .F. ) ;
#6173 = AXIS2_PLACEMENT_3D ( 'NONE', #9912, #225, #9610 ) ;
#6174 = CARTESIAN_POINT ( 'NONE',  ( 3.175426480543072749, 5.499999999999865885, -48.12500000000000000 ) ) ;
#6175 = CARTESIAN_POINT ( 'NONE',  ( 136.6949251345948255, 5.500000000000012434, -2.278174593052012309 ) ) ;
#6176 = DIRECTION ( 'NONE',  ( -7.147005652999508048E-36, 5.642372883946980038E-36, 1.000000000000000000 ) ) ;
#6177 = CARTESIAN_POINT ( 'NONE',  ( -7.216878364870328078, 0.000000000000000000, -66.05801270189226670 ) ) ;
#6178 = CARTESIAN_POINT ( 'NONE',  ( 6.000000000000000888, 1.743066579297358182E-13, -81.66367513459481131 ) ) ;
#6179 = CARTESIAN_POINT ( 'NONE',  ( 147.6413997308104058, 2.071067811865468400, -4.999999999999989342 ) ) ;
#6180 = CARTESIAN_POINT ( 'NONE',  ( 5.999999999999949374, 1.607695154586804565, -102.5966878364870780 ) ) ;
#6181 = CARTESIAN_POINT ( 'NONE',  ( 0.000000000000000000, 0.000000000000000000, 0.000000000000000000 ) ) ;
#6182 = FACE_OUTER_BOUND ( 'NONE', #12989, .T. ) ;
#6183 = LINE ( 'NONE', #8161, #8396 ) ;
#6184 = CARTESIAN_POINT ( 'NONE',  ( -3.175426480542816066, -5.500000000000057732, -134.3750000000000284 ) ) ;
#6185 = CARTESIAN_POINT ( 'NONE',  ( 16.35117513459494276, 2.500000000000084821, 1.035533905932689347 ) ) ;
#6186 = ORIENTED_EDGE ( 'NONE', *, *, #22000, .F. ) ;
#6187 =( GEOMETRIC_REPRESENTATION_CONTEXT ( 3 ) GLOBAL_UNCERTAINTY_ASSIGNED_CONTEXT ( ( #16752 ) ) GLOBAL_UNIT_ASSIGNED_CONTEXT ( ( #17509, #20096, #22250 ) ) REPRESENTATION_CONTEXT ( 'NONE', 'WORKASPACE' ) );
#6188 = CARTESIAN_POINT ( 'NONE',  ( -3.175426480542816066, 5.499999999999865885, -62.87500000000001421 ) ) ;
#6189 = CARTESIAN_POINT ( 'NONE',  ( -6.000000000000000888, 1.067854986875958443E-15, 7.560779664488942560E-35 ) ) ;
#6190 = CYLINDRICAL_SURFACE ( 'NONE', #23881, 0.5000000000000004441 ) ;
#6191 = ORIENTED_EDGE ( 'NONE', *, *, #7767, .F. ) ;
#6192 = CARTESIAN_POINT ( 'NONE',  ( 109.4374999999998721, -2.499999999999934719, 1.035533905932929599 ) ) ;
#6193 = CARTESIAN_POINT ( 'NONE',  ( 146.2500000000000568, -6.000000000000005329, 0.000000000000000000 ) ) ;
#6194 = TOROIDAL_SURFACE ( 'NONE', #1759, 1.000000000000000000, 0.5000000000000000000 ) ;
#6195 = EDGE_CURVE ( 'NONE', #20877, #25219, #24253, .T. ) ;
#6196 = ORIENTED_EDGE ( 'NONE', *, *, #10297, .T. ) ;
#6197 = CARTESIAN_POINT ( 'NONE',  ( 137.6250000000000284, 0.000000000000000000, -6.000000000000005329 ) ) ;
#6198 = CARTESIAN_POINT ( 'NONE',  ( 161.1892173070653200, -3.029880711177796115, 4.825706568618548964 ) ) ;
#6199 = EDGE_LOOP ( 'NONE', ( #20071, #10414, #11424, #25587 ) ) ;
#6200 = CARTESIAN_POINT ( 'NONE',  ( -6.350852961085760029, -1.281975124255709124E-13, -142.1250000000000000 ) ) ;
#6201 = EDGE_LOOP ( 'NONE', ( #9682, #17910, #13654, #13534 ) ) ;
#6202 = CARTESIAN_POINT ( 'NONE',  ( 14.56249999999998934, -1.999999999999851674, -0.8284271247462354770 ) ) ;
#6203 = ORIENTED_EDGE ( 'NONE', *, *, #9114, .T. ) ;
#6204 = CARTESIAN_POINT ( 'NONE',  ( 6.350852961086080661, -9.614813431917819062E-14, -70.87500000000004263 ) ) ;
#6205 = CARTESIAN_POINT ( 'NONE',  ( 14.62500000000008171, 1.110223024625156540E-13, 2.649519052838333888 ) ) ;
#6206 = CARTESIAN_POINT ( 'NONE',  ( -3.608439182435115633, 6.249999999999965361, -96.30801270189219565 ) ) ;
#6207 = CARTESIAN_POINT ( 'NONE',  ( -1.000434615788078574, -10.95616177385589651, -19.08065934301228239 ) ) ;
#6208 = CARTESIAN_POINT ( 'NONE',  ( 5.196152422706629359, 3.000000000000002665, -107.0386751345948682 ) ) ;
#6209 = DIRECTION ( 'NONE',  ( 1.000000000000000000, -5.551115123125773458E-17, -1.260129944081490338E-35 ) ) ;
#6210 = DIRECTION ( 'NONE',  ( 0.3742395684072007955, 0.4425345409093102700, 0.8149281720130788775 ) ) ;
#6211 = CARTESIAN_POINT ( 'NONE',  ( 3.464101615137757051, -5.999999999999979572, -64.83632486540523132 ) ) ;
#6212 =( LENGTH_UNIT ( ) NAMED_UNIT ( * ) SI_UNIT ( .MILLI., .METRE. ) );
#6213 = CARTESIAN_POINT ( 'NONE',  ( -6.350852961085760029, -1.281975124255709124E-13, -155.6249999999999716 ) ) ;
#6214 = CARTESIAN_POINT ( 'NONE',  ( 17.83632486540526330, 1.767766952966431937, 1.767766952966376426 ) ) ;
#6215 = CARTESIAN_POINT ( 'NONE',  ( -4.293779821584444711, 3.976156217467954779, -179.9999999999999147 ) ) ;
#6216 = EDGE_CURVE ( 'NONE', #4423, #21660, #9313, .T. ) ;
#6217 = PRODUCT ( 'Fixed Jaw', 'Fixed Jaw', '', ( #4206 ) ) ;
#6218 = CARTESIAN_POINT ( 'NONE',  ( -6.350852961085760029, -1.281975124255709124E-13, -85.12499999999998579 ) ) ;
#6219 = TOROIDAL_SURFACE ( 'NONE', #7686, 11.00000000000000355, 1.000000000000000000 ) ;
#6220 = PRESENTATION_STYLE_ASSIGNMENT (( #25403 ) ) ;
#6221 = CARTESIAN_POINT ( 'NONE',  ( -3.175426480542816510, -5.500000000000057732, -71.37499999999997158 ) ) ;
#6222 = CARTESIAN_POINT ( 'NONE',  ( 116.0000000000000142, 6.735557395310442023E-16, 5.500000000000000000 ) ) ;
#6223 = CARTESIAN_POINT ( 'NONE',  ( 0.000000000000000000, 0.000000000000000000, 0.000000000000000000 ) ) ;
#6224 = CARTESIAN_POINT ( 'NONE',  ( 5.999999999999949374, 1.607695154586804565, -104.0966878364870638 ) ) ;
#6225 = LINE ( 'NONE', #18235, #19065 ) ;
#6226 = FACE_OUTER_BOUND ( 'NONE', #197, .T. ) ;
#6227 = EDGE_CURVE ( 'NONE', #15395, #28093, #10429, .T. ) ;
#6228 = ORIENTED_EDGE ( 'NONE', *, *, #14952, .T. ) ;
#6229 = CARTESIAN_POINT ( 'NONE',  ( 156.7500000000000284, -6.000000000000005329, 0.000000000000000000 ) ) ;
#6230 = CARTESIAN_POINT ( 'NONE',  ( 3.464101615137757051, -5.999999999999979572, -171.9136751345948255 ) ) ;
#6231 = CARTESIAN_POINT ( 'NONE',  ( 116.4377832217621602, 1.849990392679621953, 0.7662911109081291805 ) ) ;
#6232 = VERTEX_POINT ( 'NONE', #7672 ) ;
#6233 = CIRCLE ( 'NONE', #18054, 11.00000000000000355 ) ;
#6234 = ORIENTED_EDGE ( 'NONE', *, *, #6051, .T. ) ;
#6235 = CARTESIAN_POINT ( 'NONE',  ( -4.763139720814407951, -2.750000000000016431, -97.00000000000002842 ) ) ;
#6236 = LINE ( 'NONE', #4077, #7238 ) ;
#6237 =( BOUNDED_CURVE ( )  B_SPLINE_CURVE ( 2, ( #23203, #4589, #23654, #11552, #20894, #28076, #14015, #21343, #23358 ),
 .UNSPECIFIED., .F., .T. ) 
 B_SPLINE_CURVE_WITH_KNOTS ( ( 3, 2, 2, 2, 3 ),
 ( 0.6875000000000002220, 0.6937499999999999778, 0.6999999999999997335, 0.7062499999999994893, 0.7124999999999992450 ),
 .UNSPECIFIED. ) 
 CURVE ( )  GEOMETRIC_REPRESENTATION_ITEM ( )  RATIONAL_B_SPLINE_CURVE ( ( 0.9999999999999973355, 0.9238795325112894030, 1.000000000000000000, 0.9238795325112867385, 1.000000000000000000, 0.9238795325112867385, 1.000000000000000000, 0.9238795325112961754, 0.9999999999999905631 ) ) 
 REPRESENTATION_ITEM ( '' )  );
#6238 = CARTESIAN_POINT ( 'NONE',  ( 3.608439182435180470, -6.249999999999997335, -116.5580127018922525 ) ) ;
#6239 = ORIENTED_EDGE ( 'NONE', *, *, #14386, .F. ) ;
#6240 = CARTESIAN_POINT ( 'NONE',  ( 5.999999999999949374, 1.607695154586804565, -141.0193375672974128 ) ) ;
#6241 = CARTESIAN_POINT ( 'NONE',  ( -1.000000000000000888, -9.000000000000007105, -4.000000000000003553 ) ) ;
#6242 = CARTESIAN_POINT ( 'NONE',  ( 6.000000000000000888, 1.743066579297358182E-13, -52.58632486540518869 ) ) ;
#6243 = CARTESIAN_POINT ( 'NONE',  ( 5.412658773652739619, 3.124999999999988898, -54.68301270189223828 ) ) ;
#6244 = ORIENTED_EDGE ( 'NONE', *, *, #5524, .T. ) ;
#6245 = CARTESIAN_POINT ( 'NONE',  ( 5.999999999999999112, 2.951592740943527306E-14, -153.6636751345948539 ) ) ;
#6246 = AXIS2_PLACEMENT_3D ( 'NONE', #5503, #29002, #9999 ) ;
#6247 = CARTESIAN_POINT ( 'NONE',  ( 0.000000000000000000, 5.999999999999977796, -136.2113248654052029 ) ) ;
#6248 = CIRCLE ( 'NONE', #22455, 1.000000000000000888 ) ;
#6249 = CARTESIAN_POINT ( 'NONE',  ( 3.175426480543072749, -5.500000000000105693, -164.1249999999999716 ) ) ;
#6250 = CARTESIAN_POINT ( 'NONE',  ( 116.1249999999999574, 1.767766952966265404, 1.767766952966431937 ) ) ;
#6251 = CARTESIAN_POINT ( 'NONE',  ( 140.5384615384615756, -11.07692307692306777, 4.615384615384604317 ) ) ;
#6252 = EDGE_CURVE ( 'NONE', #13261, #18063, #17762, .T. ) ;
#6253 = CARTESIAN_POINT ( 'NONE',  ( 4.763139720814407951, 2.750000000000002665, -106.7500000000000142 ) ) ;
#6254 = CARTESIAN_POINT ( 'NONE',  ( 13.41367513459493210, 1.767766952966542959, 1.767766952966376426 ) ) ;
#6255 = CARTESIAN_POINT ( 'NONE',  ( -6.350852961085760029, -1.281975124255709124E-13, -109.1250000000000426 ) ) ;
#6256 = CARTESIAN_POINT ( 'NONE',  ( 3.464101615137852974, 5.999999999999884537, -151.9136751345947971 ) ) ;
#6257 = CARTESIAN_POINT ( 'NONE',  ( -3.464101615137757051, -5.999999999999979572, -82.16367513459481131 ) ) ;
#6258 = EDGE_LOOP ( 'NONE', ( #22547, #14035, #21215, #15731 ) ) ;
#6259 = CARTESIAN_POINT ( 'NONE',  ( 15.18750000000010125, -2.649519052838298805, -1.097466725451559322 ) ) ;
#6260 = CARTESIAN_POINT ( 'NONE',  ( 116.6874999999997726, -1.035533905932659149, -2.499999999999784173 ) ) ;
#6261 = CARTESIAN_POINT ( 'NONE',  ( 111.6252832217622739, 0.000000000000000000, 1.849990392679523588 ) ) ;
#6262 = EDGE_CURVE ( 'NONE', #17525, #27786, #20710, .T. ) ;
#6263 = ADVANCED_FACE ( 'NONE', ( #15224 ), #10152, .T. ) ;
#6264 = ORIENTED_EDGE ( 'NONE', *, *, #24154, .T. ) ;
#6265 = CARTESIAN_POINT ( 'NONE',  ( 109.1247167782376124, -1.849990392679523588, 1.110223024625156540E-13 ) ) ;
#6266 = CARTESIAN_POINT ( 'NONE',  ( 2.775557561562891351E-14, 6.250000000000033751, -88.06698729810780435 ) ) ;
#6267 = CARTESIAN_POINT ( 'NONE',  ( 149.5238248654052313, 3.889087296526011706, -3.889087296526011706 ) ) ;
#6268 = ORIENTED_EDGE ( 'NONE', *, *, #11622, .F. ) ;
#6269 = CARTESIAN_POINT ( 'NONE',  ( -0.4053696738521141985, 10.99999999999998579, -31.00000000000003553 ) ) ;
#6270 = CARTESIAN_POINT ( 'NONE',  ( -6.350852961085760029, -1.281975124255709124E-13, -151.1250000000000568 ) ) ;
#6271 = ORIENTED_EDGE ( 'NONE', *, *, #15305, .F. ) ;
#6272 = CARTESIAN_POINT ( 'NONE',  ( 153.6562500000000568, -6.000000000000005329, 2.485281374238555774 ) ) ;
#6273 = CARTESIAN_POINT ( 'NONE',  ( 3.175426480543072749, -5.500000000000105693, -123.6250000000000426 ) ) ;
#6274 = CARTESIAN_POINT ( 'NONE',  ( 7.216878364870455975, -6.409875621278545621E-14, -140.3080127018922099 ) ) ;
#6275 = ORIENTED_EDGE ( 'NONE', *, *, #25722, .T. ) ;
#6276 = CARTESIAN_POINT ( 'NONE',  ( 157.0238248654052313, 3.889087296526011706, -3.889087296526011706 ) ) ;
#6277 = CARTESIAN_POINT ( 'NONE',  ( -5.412658773652684552, -3.125000000000099920, -122.0669872981078328 ) ) ;
#6278 = CARTESIAN_POINT ( 'NONE',  ( -5.412658773652739619, 3.124999999999975131, -174.8169872981077901 ) ) ;
#6279 = CARTESIAN_POINT ( 'NONE',  ( 6.350852961086080661, -9.614813431917819062E-14, -174.3750000000000284 ) ) ;
#6280 = DIRECTION ( 'NONE',  ( -1.000000000000000000, 0.000000000000000000, 0.000000000000000000 ) ) ;
#6281 = ORIENTED_EDGE ( 'NONE', *, *, #10770, .T. ) ;
#6282 = CARTESIAN_POINT ( 'NONE',  ( 6.055081547227420202, 0.000000000000000000, 0.000000000000000000 ) ) ;
#6283 = CARTESIAN_POINT ( 'NONE',  ( -9.999999999999793943, 10.00000000000000888, 4.000000000000003553 ) ) ;
#6284 = CARTESIAN_POINT ( 'NONE',  ( 139.9613248654052313, -5.500000000000005329, 0.000000000000000000 ) ) ;
#6285 = CARTESIAN_POINT ( 'NONE',  ( 23.33632486540526685, -1.767766952966154381, -1.767766952966542959 ) ) ;
#6286 = CARTESIAN_POINT ( 'NONE',  ( 113.0002832217622455, -1.308140751793585022, -1.308140751793640533 ) ) ;
#6287 = CARTESIAN_POINT ( 'NONE',  ( -7.216878364870328078, 0.000000000000000000, -69.69198729810781856 ) ) ;
#6288 = CARTESIAN_POINT ( 'NONE',  ( 2.775557561562891351E-14, 6.250000000000033751, -53.56698729810782567 ) ) ;
#6289 = DIRECTION ( 'NONE',  ( 6.938893903907222067E-15, 1.000000000000000000, 0.000000000000000000 ) ) ;
#6290 = CARTESIAN_POINT ( 'NONE',  ( 3.175426480543072749, 5.499999999999865885, -51.12500000000002132 ) ) ;
#6291 = CARTESIAN_POINT ( 'NONE',  ( 6.000000000000000888, -1.859271017917181981E-14, -171.0863248654052313 ) ) ;
#6292 =( BOUNDED_SURFACE ( )  B_SPLINE_SURFACE ( 1, 2, ( 
 ( #15222, #6892, #20887, #16315, #2144, #8590, #6739, #25009, #25158, #25308, #22882, #25637, #11544, #25467, #6585, #20577, #13242, #9201, #13389, #27608, #27763, #1675, #20276, #4121, #16007, #22585, #1982, #11228, #27452, #13543, #29624, #30238, #4431, #15859, #6424, #16158, #18593, #29775, #20416, #8752, #1825, #8904, #1515, #13857, #23197, #18294, #10927, #17994, #27310, #27915, #6278, #15698, #3962, #29927, #4279, #22732, #18139, #13702, #23041, #11390, #20733, #30084, #9053, #18444, #11700, #19053, #21339, #2296, #11543, #28370, #18750, #25307, #6891, #7048, #25787, #18905, #4278, #23501, #13701, #134, #280, #23355, #9052, #4430, #13856, #30391, #23649, #14308, #18592, #27914, #16610, #16006, #18443, #4585, #30237, #2582, #11854, #11389, #14010, #20886, #9358, #25636, #25931, #9200, #9518, #2445, #30083, #21044, #21192, #28072, #28224, #7198, #4878, #4735, #16460, #23196, #1981, #27762, #25466, #16157, #12005, #2143, #23040, #9663, #20732, #16314, #14164, #6738, #19628, #19189, #5022, #24218, #23938, #574, #421, #21494, #7931, #5467, #14452, #26372, #17041, #12740, #28967, #12590, #17342, #5173, #23787, #14731, #16756, #14876, #10114, #14587, #7350, #26657, #12295, #5618, #28659, #10416, #17193, #26517, #15026, #7488, #19484, #28517, #9962, #3166, #24369, #21931, #19768, #2876, #3314, #12150, #21639, #10265, #26080, #26218, #21786, #9810, #28815, #7777, #2723, #1016, #19340, #22082, #864, #16898, #3023, #7631, #5321, #24074, #12441, #729, #29114, #8072, #5769, #26803, #15178, #17491, #16713, #19145, #14838, #23893, #25886, #7590, #830, #14266, #17149, #21446, #17001, #16859, #14690, #26037, #23604, #11966, #12108, #24035, #28482, #9770, #2979, #7447, #12400, #26180, #7741, #10226, #3127, #5127, #21748, #4984, #21893, #378, #7151, #16565, #14550, #21293, #233, #21596, #528, #23080, #3421, #18333, #25344, #17449, #1127, #22036, #17302, #17757, #29385, #15304, #2022, #11266, #1862, #24629, #19588, #5575, #7889, #20617, #4320, #14981, #28926, #26921, #3578, #6625, #26620, #5882, #4157, #22193, #972, #24321, #3274, #29224, #13006, #12701, #13737, #22345, #15140, #10373, #1280, #19729, #10525, #10691, #8350, #22919, #29076, #27081, #8040, #13579, #26764, #20038, #5730, #24470, #12849, #6469, #27648, #16045, #19879, #8189, #29964, #17604, #15895, #25192, #8942, #9701, #7236, #6776, #6, #6924, #4771, #21076, #12038, #25667, #25967, #18942, #25505, #16495, #16644, #28106, #4913, #2618, #14342, #170, #25822, #18628, #27799, #4470, #20924, #28259, #9391, #16195, #9086, #14198, #11732, #313, #5058, #21226, #7385, #14488, #19084, #23825, #28406, #13895, #23680, #23236, #23385, #23533, #18785, #11430, #16792, #21377, #2474, #7080, #20774, #26113, #11579, #11891, #30122, #30273, #18481, #2333, #9549, #2176, #9235, #27948, #4617, #16348, #14046, #10452, #15063, #5359, #17080, #5657, #22120, #19374, #614, #21677, #14766, #21822, #28698, #26557, #12484, #3349, #26408, #17376, #10300, #16932, #7815, #29003, #19523, #7968, #24407, #12777, #21967, #17231, #10000, #19224, #26260, #12330, #19662, #768, #7521, #457, #5504, #3059, #1063, #26844, #12623, #29151, #5806, #19806, #15221, #8111, #28553, #26693, #14624, #24111, #14912, #10151, #2762, #17530, #12190, #24251, #28857, #21531, #9847, #2910, #3200, #5211, #7670, #23973, #900, #17993, #24553, #13388, #22584, #8436, #6132, #1199, #1824, #6423, #27161, #17842, #27451, #13542, #10774, #22425, #13093, #15545, #20275, #6584, #15858, #25157, #29623, #3506, #10605, #12935, #4120, #8903, #19959, #22271, #1514, #8589, #11227, #27607, #10926, #8751, #24864, #27006, #29311, #8267, #3812, #27309, #17682, #29926, #6277, #20122, #5970, #15697, #15390, #13241, #25008, #3961, #22881, #24714, #1674, #3657, #18138, #18293, #22731, #1364, #29465, #11069, #20415, #20576, #29774, #22613, #1547, #20608, #2012, #13120, #8617, #13270, #18324, #15886, #15419, #27342, #29341, #18171, #22761, #27190, #19989, #1852, #24891, #11256, #10955, #23071, #29803, #8782, #27638, #20153, #1703, #10803, #20305, #27482, #6616, #6460, #8301, #15578, #16038, #24745, #17873, #22911, #17712, #8466, #3994, #22458, #11100, #20446, #27035, #13729, #29650, #29954, #13571, #6001, #15729, #8934, #3685, #6161, #1392, #25185, #29501, #18025, #6305, #25038, #13414, #4151, #25335, #4310, #9382, #18618, #20766, #6914, #7071, #30112, #11495, #23226, #16337, #30263, #25658, #25496, #9077, #18469, #13887, #14039, #11571, #2171, #4609, #20916, #23377, #9228, #11723, #16486, #18776, #27941, #2323, #6767, #28095, #27791, #21066, #11421, #16187, #4460, #483, #14509, #336, #9877, #21105, #5083, #12216, #4644, #18810, #9266, #4498, #4938, #16670, #6952, #23850, #23412, #13921, #9728, #12061, #11760, #28136, #7262, #19106, #18659, #23264, #23707, #2358, #34, #30303, #20952, #7410, #14369, #2206, #25846, #16524, #21556, #28431, #21403, #16816, #14077, #11610, #23557, #9422, #19253, #9574, #16224, #7104, #28284, #2642, #26138, #25537, #2788, #27978, #6800, #16370, #14221, #25693, #4793, #2495, #21249, #11920, #190, #18968, #10178, #29182, #10639, #21704, #17258, #12508, #26877, #24432, #23994, #26581, #24139, #21993, #7843, #8142, #21846, #12806, #5684, #12354, #3227, #3380, #14941, #22147, #19835, #10485, #17407, #12652, #5387, #14648, #643, #7697, #15094, #5535, #2937, #26286, #928, #28881, #17560, #22300, #8001, #24583, #1231, #5839, #28580, #15254, #10025, #3532, #19403, #19549, #10328, #24280, #7549, #12963, #16958, #29036, #26721, #5236, #28726, #17106, #26431, #14795, #3083, #794, #6409, #20562, #10913, #6571, #13531, #18125, #15846, #17979, #27750, #11379, #27439, #25144, #1970, #9040, #20402, #11056, #1662, #4108, #1809, #20267, #30070, #20722, #11214, #29614, #15685, #27293, #18428, #8574, #22718, #6266, #18281, #15995, #24994, #3949, #23024, #29759, #25293, #22871, #29913, #8891, #6728, #16146, #8738, #27594, #4264, #13684, #25452, #4416, #5648, #17219, #13083, #24702, #24400, #1050, #19950, #1350, #893, #26547, #5955, #15052, #12768, #12618, #3192, #20107, #17669, #5495, #8102, #29143, #24853, #10763, #3645, #29452, #17369, #14902, #26832, #28845, #26993, #22261, #26684, #19514, #8425, #3342, #17831, #10442, #22571, #29301, #8256, #27149, #19653, #1190, #10288, #22110, #15376, #6117, #22415, #1502, #19797, #15534, #24243, #17518, #3801, #7802, #7960, #3495, #21959, #10597, #13229, #28993, #5796, #15210, #24544, #12922, #6898, #25315, #13867, #13399, #22894, #22743, #30095, #11083, #1685, #13710, #29935, #23051, #20427, #11239, #4291, #27925, #11398, #18149, #18453, #29787, #6439, #8763, #1990, #25476, #20745, #23207, #8915, #25167, #4131, #16016, #2153, #9060, #27773, #4442, #6750, #20899, #16171, #9211, #27461, #15869, #11555, #18603, #1836, #20587, #18305, #27619, #6594, #17540, #20286, #15710, #29634, #15558, #25020, #5817, #8600, #27324, #19816, #3518, #24416, #19675, #18006, #24875, #3975, #15234, #6287, #21979, #29162, #12946, #3360, #29015, #20133, #1376, #22132, #912, #8125, #7980, #3824, #27172, #26857, #22283, #22439, #13254, #12788, #17387, #8448, #24567, #1211, #15075, #5667, #22595, #29480, #26703, #10619, #19970, #10309, #1527, #6144, #10936, #29323, #1073, #8281, #10463, #17855, #24727, #17694, #27020, #5985, #15403, #3668, #13103, #10786, #9061, #18454, #9212, #25168, #20746, #4132, #8916, #27774, #18604, #6751, #16323, #11240, #30245, #18150, #22895, #13868, #11084, #13552, #1991, #6441, #30096, #16172, #20429, #6899, #20588, #11556, #4443, #25642, #13711, #2154, #1686, #29936, #29788, #23208, #27462, #8764, #20900, #25316, #27926, #15870, #23052, #1837, #18306, #27620, #4292, #6595, #16017, #11400, #29635, #12947, #1377, #29324, #20134, #8126, #17388, #26704, #15235, #17856, #1212, #22284, #29481, #8282, #3825, #17695, #13255, #22744, #8601, #27021, #8450, #1075, #27325, #22133, #1528, #10937, #5818, #18008, #3976, #24568, #5986, #10310, #26858, #10621, #6288, #15404, #7981, #22440, #19676, #5669, #15711, #24728, #27173, #3669, #15560, #13105, #15076, #24417, #20287, #25021, #29017, #3361, #12789, #10464, #19817, #15463, #4317, #22190, #20773, #13167, #27646, #3575, #1124, #13003, #13736, #11428, #20035, #10522, #19876, #8186, #17601, #26918, #22503, #15301, #22342, #1438, #1277, #20199, #27078, #29382, #8347, #29549, #8505, #9921, #21443, #17300, #28924, #28617, #5280, #24180, #5573, #5125, #376, #10224, #19295 ),
 ( #5727, #9768, #12105, #24319, #8037, #19143, #23748, #686, #28769, #10371, #26761, #10071, #7887, #26324, #14548, #28480, #7445, #2977, #7739, #2680, #29073, #17147, #7588, #16856, #26470, #23890, #14687, #14836, #3125, #3271, #2833, #828, #12255, #22034, #24032, #12398, #12699, #21593, #525, #21746, #16998, #970, #19586, #5426, #12547, #21890, #17446, #1366, #15699, #5972, #8591, #10928, #24554, #8438, #20277, #29466, #29625, #6279, #17995, #22586, #27163, #8269, #26846, #3508, #10606, #27312, #10776, #15223, #8113, #17843, #22428, #3963, #29777, #13243, #1676, #8753, #22733, #18140, #13390, #5807, #25010, #12936, #3659, #15546, #20124, #19807, #11070, #20417, #24865, #6134, #17532, #22272, #13094, #1200, #19960, #3815, #27008, #1516, #29312, #17684, #15392, #24716, #12261, #19302, #11973, #24042, #7594, #2987, #12408, #21753, #693, #16720, #10079, #28337, #16571, #240, #19014, #16425, #25748, #20849, #7158, #11191, #13505, #4694, #9479, #20539, #25120, #2104, #30203, #21155, #28184, #18558, #9320, #27726, #27568, #18254, #6548, #13817, #25599, #4084, #18863, #4551, #20696, #22846, #14129, #1784, #23468, #2406, #15968, #25266, #1944, #11350, #30046, #6705, #3944, #24700, #8100, #24542, #3492, #10759, #24398, #19947, #20266, #3340, #29297, #8253, #1188, #3642, #29449, #1046, #10441, #19795, #17828, #29141, #12920, #5793, #17516, #26830, #17668, #15208, #22568, #29611, #22258, #26991, #13080, #22413, #27148, #8572, #1500, #6116, #15531, #7170, #6603, #16025, #25906, #9491, #25324, #23624, #4299, #16585, #11982, #21312, #19029, #23058, #254, #1999, #28347, #13717, #2558, #18873, #4856, #14282, #9637, #11408, #20754, #109, #28196, #12101, #30190, #11653, #18852, #14118, #21441, #27874, #16416, #2539, #11963, #23307, #15310, #26768, #17608, #20042, #29388, #8355, #17763, #16754, #12439, #19482, #11060, #1666, #8580, #17984, #24999, #6270, #15689, #27300, #18901, #130, #23934, #2871, #19763, #9958, #28656, #7627, #17883, #15967, #5879, #15774, #1592, #3573, #15137, #10995, #22652, #22341, #29380, #17912, #29692, #29221, #24467, #3879, #13002, #10688, #10521, #1123, #18064, #15619, #3418, #6045, #27077, #22802, #8664, #20338, #27378, #15300, #12846, #24787, #26759, #24930, #1276, #20034, #19875, #8185, #6340, #13312, #22188, #15460, #3731, #1740, #25081, #4038, #13458, #24625, #17600, #13165, #5726, #11139, #20197, #8346, #17445, #20487, #17754, #29846, #22500, #26916, #27229, #6200, #1435, #10845, #29548, #8503, #11464, #6958, #25852, #27985, #11926, #4342, #7108, #13610, #6663, #11766, #27526, #27681, #23269, #1894, #20958, #9270, #6504, #2499, #13767, #9429, #2365, #21255, #4505, #40, #8826, #16078, #18208, #30309, #15928, #25225, #6806, #23113, #25543, #4194, #25383, #30156, #16529, #13926, #22957, #18664, #11300, #20651, #28142, #2063, #16376, #27836, #25698, #20808, #29997, #8973, #9119, #4650, #18513, #16230, #14082, #2211, #23419, #11616, #21110, #18364, #4799, #18813, #14227, #23563, #17678, #12066, #14801, #3087, #26142, #28886, #24709, #8264, #24145, #3653, #14514, #27002, #5965, #28438, #12220, #2647, #28291, #26292, #19110, #15385, #12515, #16822, #7269, #21853, #5394, #5087, #21559, #648, #798, #21408, #16675, #17112, #21710, #18973, #13089, #28585, #23854, #16964, #194, #7415, #488, #9579, #5244, #25997, #12360, #4944, #14375, #19554, #2795, #10032, #19258, #19408, #9884, #23710, #340, #7552, #7705, #14655, #23999, #28733, #2943, #10183, #26439, #9734, #25459, #11384, #1669, #11222, #13237, #9046, #3807, #6579, #25302, #17988, #20727, #16152, #30078, #16002, #4424, #6273, #18438, #27755, #20273, #3957, #24860, #20118, #18132, #10923, #6733, #4273, #8585, #29460, #13695, #27600, #27304, #13384, #22876, #23033, #22580, #8433, #8898, #15693, #25004, #15541, #6127, #1976, #20572, #17839, #11065, #20410, #22421, #1360, #10769, #27157, #29619, #1510, #29770, #22727, #29920, #25152, #8747, #27447, #6419, #15853, #4115, #13538, #1818, #18289, #2577, #21489, #14005, #25925, #4579, #16455, #12000, #415, #21332, #16893, #9353, #12144, #18587, #11695, #16749, #2137, #2290, #28220, #6885, #4873, #14304, #11538, #7481, #18745, #14447, #7343, #26212, #9512, #5016, #13852, #21039, #23192, #23495, #20879, #9804, #26075, #7193, #21187, #30232, #19182, #23350, #16604, #28364, #30385, #9195, #4730, #23644, #27907, #275, #11849, #28066, #25782, #16310, #28512, #23782, #14158, #7042, #2717, #25631, #2438, #128, #18899, #9657, #19048, #17637, #26798, #17485, #860, #5168, #21635, #23932, #5764, #19918, #568, #14579, #12586, #10260, #22226, #8224, #21928, #19762, #7770, #7625, #9956, #19335, #14869, #19620, #2869, #10559, #28963, #724, #12289, #7926, #28654, #26511, #26652, #15022, #8068, #17034, #12736, #26367, #29109, #29263, #17336, #5316, #24068, #3018, #5612, #12891, #3457, #17187, #5462, #15174, #14725, #12434, #24212, #19478, #1157, #1010, #21781, #3161, #10109, #24363, #3310, #24508, #28810, #22076, #10412, #10729, #1627, #22839, #13347, #1780, #18247, #29882, #15813, #11028, #3772, #13046, #20076, #6083, #13498, #15656, #1317, #24667, #20374, #27264, #15962, #20690, #6380, #22996, #17951, #25260, #4233, #22537, #22379, #20533, #8389, #8545, #8705, #26959, #8863, #1471, #27561, #6235, #30041, #25115, #4076, #13656, #27115, #18097, #17796, #29585, #11183, #1939, #6541, #9011, #10883, #11344, #29419, #24825, #5921, #15349, #15500, #29728, #13204, #27413, #3612, #20238, #24963, #3916, #22690, #11969, #380, #14123, #9618, #18403, #16272, #27720, #9472, #6699, #16118, #16421, #13970, #4689, #21448, #6847, #9315, #26039, #23462, #25422, #89, #4384, #13811, #7309, #11660, #18858, #7001, #28179, #25593, #23158, #2099, #23311, #25888, #18706, #30350, #7153, #28028, #2544, #25742, #21295, #11506, #16715, #2400, #16567, #9160, #4986, #30198, #235, #19009, #2255, #14416, #12111, #23752, #28332, #20845, #21004, #2684, #18553, #4545, #11812, #27879, #21149, #4842, #14268, #23606, #24323, #26329, #7449, #3276, #14982, #14692, #21750, #10229, #22039, #21598, #16861, #26621, #5284, #2981, #2836, #23895, #10374, #7891, #26182, #28773, #19447, #15141, #974, #12703, #19730, #7592, #5130, #17151, #19147, #17304, #12551, #17005, #24183, #12258, #21895, #19590, #14552, #3423, #24037, #29077, #8041, #22194, #5429, #17450, #9772, #12402, #28484, #832, #530, #9924, #7743, #689, #26473, #12850, #28620, #10074, #26765, #14840, #19298, #28928, #3129, #5577, #5731, #24471, #22655, #20202, #10999, #20039, #8190, #17605, #6049, #8670, #22506, #13170, #1596, #10849, #15778, #29552, #4041, #4197, #20492, #8509, #20344, #22346, #18213, #13007, #25084, #13462, #27083, #29850, #25228, #8829, #22805, #13615, #15466, #27529, #6507, #29386, #1441, #3579, #29225, #27233, #8351, #15932, #1745, #17758, #26922, #11144, #6344, #24791, #17917, #29696, #1128, #1281, #5883, #18068, #3736, #6204, #24630, #15306, #10526, #27382, #10692, #15623, #24933, #19880, #3882, #13315, #2503, #20812, #8976, #30314, #1899, #21112, #25701, #30160, #22961, #4804, #27840, #14232, #13931, #26001, #2369, #11770, #199, #23118, #4654, #13774, #25548, #47, #9585, #9432, #4947, #18518, #21259, #27684, #9123, #25856, #11305, #11468, #18818, #6666, #27989, #28144, #9274, #7112, #23568, #11930, #16532, #6961, #6810, #18368, #16082, #2067, #18975, #11619, #25388, #20655, #16380, #23274, #28294, #16678, #7274, #30002, #2215, #4346, #16237, #4510, #20963, #18670, #14086, #23422, #26443, #24002, #26731, #12664, #26589, #7710, #21713, #14379, #10339, #14520, #28737, #28891, #2798, #21411, #5249, #17117, #23714, #3093, #12363, #28588, #26294, #344, #22001, #5545, #16972, #7555, #17268, #3237, #492, #12225, #21562, #14658, #10036, #2649, #14949, #24291, #19412, #12073, #9736, #19112, #938, #29044, #28442, #7419, #655, #5398, #19701, #17417, #14806, #7857, #2948, #16825, #26145, #5093, #24149, #12520, #23859, #8010, #21857, #9888, #19262, #803, #10189, #19557, #27198, #15586, #8629, #24439, #13279, #3389, #20314, #20456, #13127, #29190, #24593, #3542, #20164, #13424, #4008, #8312, #17721, #6314, #18179, #8151, #24757, #19999, #22769, #1560, #1098, #3697, #1241, #29513, #15430, #15737, #29350, #29661, #12816, #29816, #10648, #25048, #18035, #5696, #1403, #27351, #15107, #12974, #22159, #6174, #10494, #19843, #22465, #27047, #10814, #8793, #22309, #6011, #1713, #8475, #17569, #17884, #26886 ) ),
 .UNSPECIFIED., .F., .F., .F. ) 
 B_SPLINE_SURFACE_WITH_KNOTS ( ( 2, 2 ),
 ( 3, 2, 2, 2, 2, 2, 2, 2, 2, 2, 2, 2, 2, 2, 2, 2, 2, 2, 2, 2, 2, 2, 2, 2, 2, 2, 2, 2, 2, 2, 2, 2, 2, 2, 2, 2, 2, 2, 2, 2, 2, 2, 2, 2, 2, 2, 2, 2, 2, 2, 2, 2, 2, 2, 2, 2, 2, 2, 2, 2, 2, 2, 2, 2, 2, 2, 2, 2, 2, 2, 2, 2, 2, 2, 2, 2, 2, 2, 2, 2, 2, 2, 2, 2, 2, 2, 2, 2, 2, 2, 2, 2, 2, 2, 2, 2, 2, 2, 2, 2, 2, 2, 2, 2, 2, 2, 2, 2, 2, 2, 2, 2, 2, 2, 2, 2, 2, 2, 2, 2, 2, 2, 2, 2, 2, 2, 2, 2, 2, 2, 2, 2, 2, 2, 2, 2, 2, 2, 2, 2, 2, 2, 2, 2, 2, 2, 2, 2, 2, 2, 2, 2, 2, 2, 2, 2, 2, 2, 2, 2, 2, 2, 2, 2, 2, 2, 2, 2, 2, 2, 2, 2, 2, 2, 2, 2, 2, 2, 2, 2, 2, 2, 2, 2, 2, 2, 2, 2, 2, 2, 2, 2, 2, 2, 2, 2, 2, 2, 2, 2, 2, 2, 2, 2, 2, 2, 2, 2, 2, 2, 2, 2, 2, 2, 2, 2, 2, 2, 2, 2, 2, 2, 2, 2, 2, 2, 2, 2, 2, 2, 2, 2, 2, 2, 2, 2, 2, 2, 2, 2, 2, 2, 2, 2, 2, 2, 2, 2, 2, 2, 2, 2, 2, 2, 2, 2, 2, 2, 2, 2, 2, 2, 2, 2, 2, 2, 2, 2, 2, 2, 2, 2, 2, 2, 2, 2, 2, 2, 2, 2, 2, 2, 2, 2, 2, 2, 2, 2, 2, 2, 2, 2, 2, 2, 2, 2, 2, 2, 2, 2, 2, 2, 2, 2, 2, 2, 2, 2, 2, 2, 2, 2, 2, 2, 2, 2, 2, 2, 2, 2, 2, 2, 2, 2, 2, 2, 2, 2, 2, 2, 2, 2, 2, 2, 2, 2, 2, 2, 2, 2, 2, 2, 2, 2, 2, 2, 2, 2, 2, 2, 2, 2, 2, 2, 2, 2, 2, 2, 2, 2, 2, 2, 2, 2, 2, 2, 2, 2, 2, 2, 2, 2, 2, 2, 2, 2, 2, 2, 2, 2, 2, 2, 2, 2, 2, 2, 2, 2, 2, 2, 2, 2, 2, 2, 2, 2, 2, 2, 2, 2, 2, 2, 2, 2, 2, 2, 2, 2, 2, 2, 2, 2, 2, 2, 2, 2, 2, 2, 2, 2, 2, 2, 2, 2, 2, 2, 2, 2, 2, 2, 2, 2, 2, 2, 2, 2, 2, 2, 2, 2, 2, 2, 2, 2, 2, 2, 2, 2, 2, 2, 2, 2, 2, 2, 2, 2, 2, 2, 2, 2, 2, 2, 2, 2, 2, 2, 2, 2, 2, 2, 2, 2, 2, 2, 2, 2, 2, 2, 2, 2, 2, 2, 2, 2, 2, 2, 2, 2, 2, 2, 2, 2, 2, 2, 2, 2, 2, 2, 2, 2, 2, 2, 2, 2, 2, 2, 2, 2, 2, 2, 2, 2, 2, 2, 2, 2, 2, 2, 2, 2, 2, 2, 2, 2, 2, 2, 2, 2, 2, 2, 2, 2, 2, 2, 2, 2, 2, 2, 2, 2, 3 ),
 ( 0.000000000000000000, 1.000000000000000000 ),
 ( 0.000000000000000000, 0.001851851851851851923, 0.003703703703703703845, 0.005555555555555555768, 0.007407407407407407690, 0.009259259259259258745, 0.01111111111111111154, 0.01296296296296296259, 0.01481481481481481538, 0.01666666666666666644, 0.01851851851851851749, 0.02037037037037037202, 0.02222222222222222307, 0.02407407407407407413, 0.02592592592592592518, 0.02777777777777777624, 0.02962962962962963076, 0.03148148148148147835, 0.03333333333333333287, 0.03518518518518518740, 0.03703703703703703498, 0.03888888888888888951, 0.04074074074074074403, 0.04259259259259259162, 0.04444444444444444614, 0.04629629629629629373, 0.04814814814814814825, 0.05000000000000000278, 0.05185185185185185036, 0.05370370370370370489, 0.05555555555555555247, 0.05740740740740740700, 0.05925925925925926152, 0.06111111111111110911, 0.06296296296296295669, 0.06481481481481481122, 0.06666666666666666574, 0.06851851851851852027, 0.07037037037037037479, 0.07222222222222221544, 0.07407407407407406996, 0.07592592592592592449, 0.07777777777777777901, 0.07962962962962963354, 0.08148148148148148806, 0.08333333333333332871, 0.08518518518518518323, 0.08703703703703703776, 0.08888888888888889228, 0.09074074074074074681, 0.09259259259259258745, 0.09444444444444444198, 0.09629629629629629650, 0.09814814814814815103, 0.1000000000000000056, 0.1018518518518518462, 0.1037037037037037007, 0.1055555555555555552, 0.1074074074074074098, 0.1092592592592592643, 0.1111111111111111049, 0.1129629629629629595, 0.1148148148148148140, 0.1166666666666666685, 0.1185185185185185230, 0.1203703703703703637, 0.1222222222222222182, 0.1240740740740740727, 0.1259259259259259134, 0.1277777777777777679, 0.1296296296296296224, 0.1314814814814814770, 0.1333333333333333315, 0.1351851851851851860, 0.1370370370370370405, 0.1388888888888888951, 0.1407407407407407496, 0.1425925925925926041, 0.1444444444444444309, 0.1462962962962962854, 0.1481481481481481399, 0.1499999999999999944, 0.1518518518518518490, 0.1537037037037037035, 0.1555555555555555580, 0.1574074074074074125, 0.1592592592592592671, 0.1611111111111111216, 0.1629629629629629761, 0.1648148148148148029, 0.1666666666666666574, 0.1685185185185185119, 0.1703703703703703665, 0.1722222222222222210, 0.1740740740740740755, 0.1759259259259259300, 0.1777777777777777846, 0.1796296296296296391, 0.1814814814814814936, 0.1833333333333333204, 0.1851851851851851749, 0.1870370370370370294, 0.1888888888888888840, 0.1907407407407407385, 0.1925925925925925930, 0.1944444444444444475, 0.1962962962962963021, 0.1981481481481481566, 0.2000000000000000111, 0.2018518518518518656, 0.2037037037037036924, 0.2055555555555555469, 0.2074074074074074014, 0.2092592592592592560, 0.2111111111111111105, 0.2129629629629629650, 0.2148148148148148195, 0.2166666666666666741, 0.2185185185185185286, 0.2203703703703703831, 0.2222222222222222099, 0.2240740740740740644, 0.2259259259259259189, 0.2277777777777777735, 0.2296296296296296280, 0.2314814814814814825, 0.2333333333333333370, 0.2351851851851851916, 0.2370370370370370461, 0.2388888888888889006, 0.2407407407407407274, 0.2425925925925925819, 0.2444444444444444364, 0.2462962962962962910, 0.2481481481481481455, 0.2500000000000000000, 0.2518518518518518268, 0.2537037037037037090, 0.2555555555555555358, 0.2574074074074074181, 0.2592592592592592449, 0.2611111111111111271, 0.2629629629629629539, 0.2648148148148148362, 0.2666666666666666630, 0.2685185185185185452, 0.2703703703703703720, 0.2722222222222221988, 0.2740740740740740811, 0.2759259259259259078, 0.2777777777777777901, 0.2796296296296296169, 0.2814814814814814992, 0.2833333333333333259, 0.2851851851851852082, 0.2870370370370370350, 0.2888888888888888618, 0.2907407407407407440, 0.2925925925925925708, 0.2944444444444444531, 0.2962962962962962798, 0.2981481481481481621, 0.2999999999999999889, 0.3018518518518518712, 0.3037037037037036979, 0.3055555555555555802, 0.3074074074074074070, 0.3092592592592592338, 0.3111111111111111160, 0.3129629629629629428, 0.3148148148148148251, 0.3166666666666666519, 0.3185185185185185341, 0.3203703703703703609, 0.3222222222222222432, 0.3240740740740740700, 0.3259259259259259522, 0.3277777777777777790, 0.3296296296296296058, 0.3314814814814814881, 0.3333333333333333148, 0.3351851851851851971, 0.3370370370370370239, 0.3388888888888889062, 0.3407407407407407329, 0.3425925925925926152, 0.3444444444444444420, 0.3462962962962962687, 0.3481481481481481510, 0.3499999999999999778, 0.3518518518518518601, 0.3537037037037036868, 0.3555555555555555691, 0.3574074074074073959, 0.3592592592592592782, 0.3611111111111111049, 0.3629629629629629872, 0.3648148148148148140, 0.3666666666666666408, 0.3685185185185185230, 0.3703703703703703498, 0.3722222222222222321, 0.3740740740740740589, 0.3759259259259259411, 0.3777777777777777679, 0.3796296296296296502, 0.3814814814814814770, 0.3833333333333333592, 0.3851851851851851860, 0.3870370370370370128, 0.3888888888888888951, 0.3907407407407407218, 0.3925925925925926041, 0.3944444444444444309, 0.3962962962962963132, 0.3981481481481481399, 0.4000000000000000222, 0.4018518518518518490, 0.4037037037037037313, 0.4055555555555555580, 0.4074074074074073848, 0.4092592592592592671, 0.4111111111111110938, 0.4129629629629629761, 0.4148148148148148029, 0.4166666666666666852, 0.4185185185185185119, 0.4203703703703703942, 0.4222222222222222210, 0.4240740740740740478, 0.4259259259259259300, 0.4277777777777777568, 0.4296296296296296391, 0.4314814814814814659, 0.4333333333333333481, 0.4351851851851851749, 0.4370370370370370572, 0.4388888888888888840, 0.4407407407407407662, 0.4425925925925925930, 0.4444444444444444198, 0.4462962962962963021, 0.4481481481481481288, 0.4500000000000000111, 0.4518518518518518379, 0.4537037037037037202, 0.4555555555555555469, 0.4574074074074074292, 0.4592592592592592560, 0.4611111111111111382, 0.4629629629629629650, 0.4648148148148147918, 0.4666666666666666741, 0.4685185185185185008, 0.4703703703703703831, 0.4722222222222222099, 0.4740740740740740922, 0.4759259259259259189, 0.4777777777777778012, 0.4796296296296296280, 0.4814814814814814548, 0.4833333333333333370, 0.4851851851851851638, 0.4870370370370370461, 0.4888888888888888729, 0.4907407407407407551, 0.4925925925925925819, 0.4944444444444444642, 0.4962962962962962910, 0.4981481481481481732, 0.5000000000000000000, 0.5018518518518518823, 0.5037037037037036535, 0.5055555555555555358, 0.5074074074074074181, 0.5092592592592593004, 0.5111111111111110716, 0.5129629629629629539, 0.5148148148148148362, 0.5166666666666667185, 0.5185185185185184897, 0.5203703703703703720, 0.5222222222222222543, 0.5240740740740740256, 0.5259259259259259078, 0.5277777777777777901, 0.5296296296296296724, 0.5314814814814814437, 0.5333333333333333259, 0.5351851851851852082, 0.5370370370370370905, 0.5388888888888888618, 0.5407407407407407440, 0.5425925925925926263, 0.5444444444444443976, 0.5462962962962962798, 0.5481481481481481621, 0.5500000000000000444, 0.5518518518518518157, 0.5537037037037036979, 0.5555555555555555802, 0.5574074074074074625, 0.5592592592592592338, 0.5611111111111111160, 0.5629629629629629983, 0.5648148148148147696, 0.5666666666666666519, 0.5685185185185185341, 0.5703703703703704164, 0.5722222222222221877, 0.5740740740740740700, 0.5759259259259259522, 0.5777777777777777235, 0.5796296296296296058, 0.5814814814814814881, 0.5833333333333333703, 0.5851851851851851416, 0.5870370370370370239, 0.5888888888888889062, 0.5907407407407407884, 0.5925925925925925597, 0.5944444444444444420, 0.5962962962962963243, 0.5981481481481480955, 0.5999999999999999778, 0.6018518518518518601, 0.6037037037037037424, 0.6055555555555555136, 0.6074074074074073959, 0.6092592592592592782, 0.6111111111111111605, 0.6129629629629629317, 0.6148148148148148140, 0.6166666666666666963, 0.6185185185185184675, 0.6203703703703703498, 0.6222222222222222321, 0.6240740740740741144, 0.6259259259259258856, 0.6277777777777777679, 0.6296296296296296502, 0.6314814814814815325, 0.6333333333333333037, 0.6351851851851851860, 0.6370370370370370683, 0.6388888888888888395, 0.6407407407407407218, 0.6425925925925926041, 0.6444444444444444864, 0.6462962962962962576, 0.6481481481481481399, 0.6500000000000000222, 0.6518518518518519045, 0.6537037037037036757, 0.6555555555555555580, 0.6574074074074074403, 0.6592592592592592116, 0.6611111111111110938, 0.6629629629629629761, 0.6648148148148148584, 0.6666666666666666297, 0.6685185185185185119, 0.6703703703703703942, 0.6722222222222222765, 0.6740740740740740478, 0.6759259259259259300, 0.6777777777777778123, 0.6796296296296295836, 0.6814814814814814659, 0.6833333333333333481, 0.6851851851851852304, 0.6870370370370370017, 0.6888888888888888840, 0.6907407407407407662, 0.6925925925925925375, 0.6944444444444444198, 0.6962962962962963021, 0.6981481481481481843, 0.6999999999999999556, 0.7018518518518518379, 0.7037037037037037202, 0.7055555555555556024, 0.7074074074074073737, 0.7092592592592592560, 0.7111111111111111382, 0.7129629629629629095, 0.7148148148148147918, 0.7166666666666666741, 0.7185185185185185563, 0.7203703703703703276, 0.7222222222222222099, 0.7240740740740740922, 0.7259259259259259744, 0.7277777777777777457, 0.7296296296296296280, 0.7314814814814815103, 0.7333333333333332815, 0.7351851851851851638, 0.7370370370370370461, 0.7388888888888889284, 0.7407407407407406996, 0.7425925925925925819, 0.7444444444444444642, 0.7462962962962963465, 0.7481481481481481177, 0.7500000000000000000, 0.7518518518518518823, 0.7537037037037036535, 0.7555555555555555358, 0.7574074074074074181, 0.7592592592592593004, 0.7611111111111110716, 0.7629629629629629539, 0.7648148148148148362, 0.7666666666666667185, 0.7685185185185184897, 0.7703703703703703720, 0.7722222222222222543, 0.7740740740740740256, 0.7759259259259259078, 0.7777777777777777901, 0.7796296296296296724, 0.7814814814814814437, 0.7833333333333333259, 0.7851851851851852082, 0.7870370370370370905, 0.7888888888888888618, 0.7907407407407407440, 0.7925925925925926263, 0.7944444444444443976, 0.7962962962962962798, 0.7981481481481481621, 0.8000000000000000444, 0.8018518518518518157, 0.8037037037037036979, 0.8055555555555555802, 0.8074074074074074625, 0.8092592592592592338, 0.8111111111111111160, 0.8129629629629629983, 0.8148148148148147696, 0.8166666666666666519, 0.8185185185185185341, 0.8203703703703704164, 0.8222222222222221877, 0.8240740740740740700, 0.8259259259259259522, 0.8277777777777777235, 0.8296296296296296058, 0.8314814814814814881, 0.8333333333333333703, 0.8351851851851851416, 0.8370370370370370239, 0.8388888888888889062, 0.8407407407407407884, 0.8425925925925925597, 0.8444444444444444420, 0.8462962962962963243, 0.8481481481481480955, 0.8499999999999999778, 0.8518518518518518601, 0.8537037037037037424, 0.8555555555555555136, 0.8574074074074073959, 0.8592592592592592782, 0.8611111111111111605, 0.8629629629629629317, 0.8648148148148148140, 0.8666666666666666963, 0.8685185185185184675, 0.8703703703703703498, 0.8722222222222222321, 0.8740740740740741144, 0.8759259259259258856, 0.8777777777777777679, 0.8796296296296296502, 0.8814814814814815325, 0.8833333333333333037, 0.8851851851851851860, 0.8870370370370370683, 0.8888888888888888395, 0.8907407407407407218, 0.8925925925925926041, 0.8944444444444444864, 0.8962962962962962576, 0.8981481481481481399, 0.9000000000000000222, 0.9018518518518519045, 0.9037037037037036757, 0.9055555555555555580, 0.9074074074074074403, 0.9092592592592592116, 0.9111111111111110938, 0.9129629629629629761, 0.9148148148148148584, 0.9166666666666666297, 0.9185185185185185119, 0.9203703703703703942, 0.9222222222222222765, 0.9240740740740740478, 0.9259259259259259300, 0.9277777777777778123, 0.9296296296296295836, 0.9314814814814814659, 0.9333333333333333481, 0.9351851851851852304, 0.9370370370370370017, 0.9388888888888888840, 0.9407407407407407662, 0.9425925925925925375, 0.9444444444444444198, 0.9462962962962963021, 0.9481481481481481843, 0.9499999999999999556, 0.9518518518518518379, 0.9537037037037037202, 0.9555555555555556024, 0.9574074074074073737, 0.9592592592592592560, 0.9611111111111111382, 0.9629629629629629095, 0.9648148148148147918, 0.9666666666666666741, 0.9685185185185185563, 0.9703703703703703276, 0.9722222222222222099, 0.9740740740740740922, 0.9759259259259259744, 0.9777777777777777457, 0.9796296296296296280, 0.9814814814814815103, 0.9833333333333332815, 0.9851851851851851638, 0.9870370370370370461, 0.9888888888888889284, 0.9907407407407406996, 0.9925925925925925819, 0.9944444444444444642, 0.9962962962962963465, 0.9981481481481481177, 1.000000000000000000 ),
 .UNSPECIFIED. ) 
 GEOMETRIC_REPRESENTATION_ITEM ( )  RATIONAL_B_SPLINE_SURFACE ( (
 ( 1.000000000000000000, 0.8660254037844387076, 1.000000000000000000, 0.8660254037844387076, 1.000000000000000000, 0.8660254037844387076, 1.000000000000000000, 0.8660254037844387076, 1.000000000000000000, 0.8660254037844387076, 1.000000000000000000, 0.8660254037844387076, 1.000000000000000000, 0.8660254037844387076, 1.000000000000000000, 0.8660254037844387076, 1.000000000000000000, 0.8660254037844387076, 1.000000000000000000, 0.8660254037844387076, 1.000000000000000000, 0.8660254037844387076, 1.000000000000000000, 0.8660254037844387076, 1.000000000000000000, 0.8660254037844387076, 1.000000000000000000, 0.8660254037844387076, 1.000000000000000000, 0.8660254037844387076, 1.000000000000000000, 0.8660254037844387076, 1.000000000000000000, 0.8660254037844387076, 1.000000000000000000, 0.8660254037844387076, 1.000000000000000000, 0.8660254037844387076, 1.000000000000000000, 0.8660254037844387076, 1.000000000000000000, 0.8660254037844387076, 1.000000000000000000, 0.8660254037844387076, 1.000000000000000000, 0.8660254037844387076, 1.000000000000000000, 0.8660254037844387076, 1.000000000000000000, 0.8660254037844387076, 1.000000000000000000, 0.8660254037844387076, 1.000000000000000000, 0.8660254037844387076, 1.000000000000000000, 0.8660254037844387076, 1.000000000000000000, 0.8660254037844387076, 1.000000000000000000, 0.8660254037844387076, 1.000000000000000000, 0.8660254037844387076, 1.000000000000000000, 0.8660254037844387076, 1.000000000000000000, 0.8660254037844387076, 1.000000000000000000, 0.8660254037844387076, 1.000000000000000000, 0.8660254037844387076, 1.000000000000000000, 0.8660254037844387076, 1.000000000000000000, 0.8660254037844387076, 1.000000000000000000, 0.8660254037844387076, 1.000000000000000000, 0.8660254037844387076, 1.000000000000000000, 0.8660254037844387076, 1.000000000000000000, 0.8660254037844387076, 1.000000000000000000, 0.8660254037844387076, 1.000000000000000000, 0.8660254037844387076, 1.000000000000000000, 0.8660254037844387076, 1.000000000000000000, 0.8660254037844387076, 1.000000000000000000, 0.8660254037844387076, 1.000000000000000000, 0.8660254037844387076, 1.000000000000000000, 0.8660254037844387076, 1.000000000000000000, 0.8660254037844387076, 1.000000000000000000, 0.8660254037844387076, 1.000000000000000000, 0.8660254037844387076, 1.000000000000000000, 0.8660254037844387076, 1.000000000000000000, 0.8660254037844387076, 1.000000000000000000, 0.8660254037844387076, 1.000000000000000000, 0.8660254037844387076, 1.000000000000000000, 0.8660254037844387076, 1.000000000000000000, 0.8660254037844387076, 1.000000000000000000, 0.8660254037844387076, 1.000000000000000000, 0.8660254037844387076, 1.000000000000000000, 0.8660254037844387076, 1.000000000000000000, 0.8660254037844387076, 1.000000000000000000, 0.8660254037844387076, 1.000000000000000000, 0.8660254037844387076, 1.000000000000000000, 0.8660254037844387076, 1.000000000000000000, 0.8660254037844387076, 1.000000000000000000, 0.8660254037844387076, 1.000000000000000000, 0.8660254037844387076, 1.000000000000000000, 0.8660254037844387076, 1.000000000000000000, 0.8660254037844387076, 1.000000000000000000, 0.8660254037844387076, 1.000000000000000000, 0.8660254037844387076, 1.000000000000000000, 0.8660254037844387076, 1.000000000000000000, 0.8660254037844387076, 1.000000000000000000, 0.8660254037844387076, 1.000000000000000000, 0.8660254037844387076, 1.000000000000000000, 0.8660254037844387076, 1.000000000000000000, 0.8660254037844387076, 1.000000000000000000, 0.8660254037844387076, 1.000000000000000000, 0.8660254037844387076, 1.000000000000000000, 0.8660254037844387076, 1.000000000000000000, 0.8660254037844387076, 1.000000000000000000, 0.8660254037844387076, 1.000000000000000000, 0.8660254037844387076, 1.000000000000000000, 0.8660254037844387076, 1.000000000000000000, 0.8660254037844387076, 1.000000000000000000, 0.8660254037844387076, 1.000000000000000000, 0.8660254037844387076, 1.000000000000000000, 0.8660254037844387076, 1.000000000000000000, 0.8660254037844387076, 1.000000000000000000, 0.8660254037844387076, 1.000000000000000000, 0.8660254037844387076, 1.000000000000000000, 0.8660254037844387076, 1.000000000000000000, 0.8660254037844387076, 1.000000000000000000, 0.8660254037844387076, 1.000000000000000000, 0.8660254037844387076, 1.000000000000000000, 0.8660254037844387076, 1.000000000000000000, 0.8660254037844387076, 1.000000000000000000, 0.8660254037844387076, 1.000000000000000000, 0.8660254037844387076, 1.000000000000000000, 0.8660254037844387076, 1.000000000000000000, 0.8660254037844387076, 1.000000000000000000, 0.8660254037844387076, 1.000000000000000000, 0.8660254037844387076, 1.000000000000000000, 0.8660254037844387076, 1.000000000000000000, 0.8660254037844387076, 1.000000000000000000, 0.8660254037844387076, 1.000000000000000000, 0.8660254037844387076, 1.000000000000000000, 0.8660254037844387076, 1.000000000000000000, 0.8660254037844387076, 1.000000000000000000, 0.8660254037844387076, 1.000000000000000000, 0.8660254037844387076, 1.000000000000000000, 0.8660254037844387076, 1.000000000000000000, 0.8660254037844387076, 1.000000000000000000, 0.8660254037844387076, 1.000000000000000000, 0.8660254037844387076, 1.000000000000000000, 0.8660254037844387076, 1.000000000000000000, 0.8660254037844387076, 1.000000000000000000, 0.8660254037844387076, 1.000000000000000000, 0.8660254037844387076, 1.000000000000000000, 0.8660254037844387076, 1.000000000000000000, 0.8660254037844387076, 1.000000000000000000, 0.8660254037844387076, 1.000000000000000000, 0.8660254037844387076, 1.000000000000000000, 0.8660254037844387076, 1.000000000000000000, 0.8660254037844387076, 1.000000000000000000, 0.8660254037844387076, 1.000000000000000000, 0.8660254037844387076, 1.000000000000000000, 0.8660254037844387076, 1.000000000000000000, 0.8660254037844387076, 1.000000000000000000, 0.8660254037844387076, 1.000000000000000000, 0.8660254037844387076, 1.000000000000000000, 0.8660254037844387076, 1.000000000000000000, 0.8660254037844387076, 1.000000000000000000, 0.8660254037844387076, 1.000000000000000000, 0.8660254037844387076, 1.000000000000000000, 0.8660254037844387076, 1.000000000000000000, 0.8660254037844387076, 1.000000000000000000, 0.8660254037844387076, 1.000000000000000000, 0.8660254037844387076, 1.000000000000000000, 0.8660254037844387076, 1.000000000000000000, 0.8660254037844387076, 1.000000000000000000, 0.8660254037844387076, 1.000000000000000000, 0.8660254037844387076, 1.000000000000000000, 0.8660254037844387076, 1.000000000000000000, 0.8660254037844387076, 1.000000000000000000, 0.8660254037844387076, 1.000000000000000000, 0.8660254037844387076, 1.000000000000000000, 0.8660254037844387076, 1.000000000000000000, 0.8660254037844387076, 1.000000000000000000, 0.8660254037844387076, 1.000000000000000000, 0.8660254037844387076, 1.000000000000000000, 0.8660254037844387076, 1.000000000000000000, 0.8660254037844387076, 1.000000000000000000, 0.8660254037844387076, 1.000000000000000000, 0.8660254037844387076, 1.000000000000000000, 0.8660254037844387076, 1.000000000000000000, 0.8660254037844387076, 1.000000000000000000, 0.8660254037844387076, 1.000000000000000000, 0.8660254037844387076, 1.000000000000000000, 0.8660254037844387076, 1.000000000000000000, 0.8660254037844387076, 1.000000000000000000, 0.8660254037844387076, 1.000000000000000000, 0.8660254037844387076, 1.000000000000000000, 0.8660254037844387076, 1.000000000000000000, 0.8660254037844387076, 1.000000000000000000, 0.8660254037844387076, 1.000000000000000000, 0.8660254037844387076, 1.000000000000000000, 0.8660254037844387076, 1.000000000000000000, 0.8660254037844387076, 1.000000000000000000, 0.8660254037844387076, 1.000000000000000000, 0.8660254037844387076, 1.000000000000000000, 0.8660254037844387076, 1.000000000000000000, 0.8660254037844387076, 1.000000000000000000, 0.8660254037844387076, 1.000000000000000000, 0.8660254037844387076, 1.000000000000000000, 0.8660254037844387076, 1.000000000000000000, 0.8660254037844387076, 1.000000000000000000, 0.8660254037844387076, 1.000000000000000000, 0.8660254037844387076, 1.000000000000000000, 0.8660254037844387076, 1.000000000000000000, 0.8660254037844387076, 1.000000000000000000, 0.8660254037844387076, 1.000000000000000000, 0.8660254037844387076, 1.000000000000000000, 0.8660254037844387076, 1.000000000000000000, 0.8660254037844387076, 1.000000000000000000, 0.8660254037844387076, 1.000000000000000000, 0.8660254037844387076, 1.000000000000000000, 0.8660254037844387076, 1.000000000000000000, 0.8660254037844387076, 1.000000000000000000, 0.8660254037844387076, 1.000000000000000000, 0.8660254037844387076, 1.000000000000000000, 0.8660254037844387076, 1.000000000000000000, 0.8660254037844387076, 1.000000000000000000, 0.8660254037844387076, 1.000000000000000000, 0.8660254037844387076, 1.000000000000000000, 0.8660254037844387076, 1.000000000000000000, 0.8660254037844387076, 1.000000000000000000, 0.8660254037844387076, 1.000000000000000000, 0.8660254037844387076, 1.000000000000000000, 0.8660254037844387076, 1.000000000000000000, 0.8660254037844387076, 1.000000000000000000, 0.8660254037844387076, 1.000000000000000000, 0.8660254037844387076, 1.000000000000000000, 0.8660254037844387076, 1.000000000000000000, 0.8660254037844387076, 1.000000000000000000, 0.8660254037844387076, 1.000000000000000000, 0.8660254037844387076, 1.000000000000000000, 0.8660254037844387076, 1.000000000000000000, 0.8660254037844387076, 1.000000000000000000, 0.8660254037844387076, 1.000000000000000000, 0.8660254037844387076, 1.000000000000000000, 0.8660254037844387076, 1.000000000000000000, 0.8660254037844387076, 1.000000000000000000, 0.8660254037844387076, 1.000000000000000000, 0.8660254037844387076, 1.000000000000000000, 0.8660254037844387076, 1.000000000000000000, 0.8660254037844387076, 1.000000000000000000, 0.8660254037844387076, 1.000000000000000000, 0.8660254037844387076, 1.000000000000000000, 0.8660254037844387076, 1.000000000000000000, 0.8660254037844387076, 1.000000000000000000, 0.8660254037844387076, 1.000000000000000000, 0.8660254037844387076, 1.000000000000000000, 0.8660254037844387076, 1.000000000000000000, 0.8660254037844387076, 1.000000000000000000, 0.8660254037844387076, 1.000000000000000000, 0.8660254037844387076, 1.000000000000000000, 0.8660254037844387076, 1.000000000000000000, 0.8660254037844387076, 1.000000000000000000, 0.8660254037844387076, 1.000000000000000000, 0.8660254037844387076, 1.000000000000000000, 0.8660254037844387076, 1.000000000000000000, 0.8660254037844387076, 1.000000000000000000, 0.8660254037844387076, 1.000000000000000000, 0.8660254037844387076, 1.000000000000000000, 0.8660254037844387076, 1.000000000000000000, 0.8660254037844387076, 1.000000000000000000, 0.8660254037844387076, 1.000000000000000000, 0.8660254037844387076, 1.000000000000000000, 0.8660254037844387076, 1.000000000000000000, 0.8660254037844387076, 1.000000000000000000, 0.8660254037844387076, 1.000000000000000000, 0.8660254037844387076, 1.000000000000000000, 0.8660254037844387076, 1.000000000000000000, 0.8660254037844387076, 1.000000000000000000, 0.8660254037844387076, 1.000000000000000000, 0.8660254037844387076, 1.000000000000000000, 0.8660254037844387076, 1.000000000000000000, 0.8660254037844387076, 1.000000000000000000, 0.8660254037844387076, 1.000000000000000000, 0.8660254037844387076, 1.000000000000000000, 0.8660254037844387076, 1.000000000000000000, 0.8660254037844387076, 1.000000000000000000, 0.8660254037844387076, 1.000000000000000000, 0.8660254037844387076, 1.000000000000000000, 0.8660254037844387076, 1.000000000000000000, 0.8660254037844387076, 1.000000000000000000, 0.8660254037844387076, 1.000000000000000000, 0.8660254037844387076, 1.000000000000000000, 0.8660254037844387076, 1.000000000000000000, 0.8660254037844387076, 1.000000000000000000, 0.8660254037844387076, 1.000000000000000000, 0.8660254037844387076, 1.000000000000000000, 0.8660254037844387076, 1.000000000000000000, 0.8660254037844387076, 1.000000000000000000, 0.8660254037844387076, 1.000000000000000000, 0.8660254037844387076, 1.000000000000000000, 0.8660254037844387076, 1.000000000000000000, 0.8660254037844387076, 1.000000000000000000, 0.8660254037844387076, 1.000000000000000000, 0.8660254037844387076, 1.000000000000000000, 0.8660254037844387076, 1.000000000000000000, 0.8660254037844387076, 1.000000000000000000, 0.8660254037844387076, 1.000000000000000000, 0.8660254037844387076, 1.000000000000000000, 0.8660254037844387076, 1.000000000000000000, 0.8660254037844387076, 1.000000000000000000, 0.8660254037844387076, 1.000000000000000000, 0.8660254037844387076, 1.000000000000000000, 0.8660254037844387076, 1.000000000000000000, 0.8660254037844387076, 1.000000000000000000, 0.8660254037844387076, 1.000000000000000000, 0.8660254037844387076, 1.000000000000000000, 0.8660254037844387076, 1.000000000000000000, 0.8660254037844387076, 1.000000000000000000, 0.8660254037844387076, 1.000000000000000000, 0.8660254037844387076, 1.000000000000000000, 0.8660254037844387076, 1.000000000000000000, 0.8660254037844387076, 1.000000000000000000, 0.8660254037844387076, 1.000000000000000000, 0.8660254037844387076, 1.000000000000000000, 0.8660254037844387076, 1.000000000000000000, 0.8660254037844387076, 1.000000000000000000, 0.8660254037844387076, 1.000000000000000000, 0.8660254037844387076, 1.000000000000000000, 0.8660254037844387076, 1.000000000000000000, 0.8660254037844387076, 1.000000000000000000, 0.8660254037844387076, 1.000000000000000000, 0.8660254037844387076, 1.000000000000000000, 0.8660254037844387076, 1.000000000000000000, 0.8660254037844387076, 1.000000000000000000, 0.8660254037844387076, 1.000000000000000000, 0.8660254037844387076, 1.000000000000000000, 0.8660254037844387076, 1.000000000000000000, 0.8660254037844387076, 1.000000000000000000, 0.8660254037844387076, 1.000000000000000000, 0.8660254037844387076, 1.000000000000000000, 0.8660254037844387076, 1.000000000000000000, 0.8660254037844387076, 1.000000000000000000, 0.8660254037844387076, 1.000000000000000000, 0.8660254037844387076, 1.000000000000000000, 0.8660254037844387076, 1.000000000000000000, 0.8660254037844387076, 1.000000000000000000, 0.8660254037844387076, 1.000000000000000000, 0.8660254037844387076, 1.000000000000000000, 0.8660254037844387076, 1.000000000000000000, 0.8660254037844387076, 1.000000000000000000, 0.8660254037844387076, 1.000000000000000000, 0.8660254037844387076, 1.000000000000000000, 0.8660254037844387076, 1.000000000000000000, 0.8660254037844387076, 1.000000000000000000, 0.8660254037844387076, 1.000000000000000000, 0.8660254037844387076, 1.000000000000000000, 0.8660254037844387076, 1.000000000000000000, 0.8660254037844387076, 1.000000000000000000, 0.8660254037844387076, 1.000000000000000000, 0.8660254037844387076, 1.000000000000000000, 0.8660254037844387076, 1.000000000000000000, 0.8660254037844387076, 1.000000000000000000, 0.8660254037844387076, 1.000000000000000000, 0.8660254037844387076, 1.000000000000000000, 0.8660254037844387076, 1.000000000000000000, 0.8660254037844387076, 1.000000000000000000, 0.8660254037844387076, 1.000000000000000000, 0.8660254037844387076, 1.000000000000000000, 0.8660254037844387076, 1.000000000000000000, 0.8660254037844387076, 1.000000000000000000, 0.8660254037844387076, 1.000000000000000000, 0.8660254037844387076, 1.000000000000000000, 0.8660254037844387076, 1.000000000000000000, 0.8660254037844387076, 1.000000000000000000, 0.8660254037844387076, 1.000000000000000000, 0.8660254037844387076, 1.000000000000000000, 0.8660254037844387076, 1.000000000000000000, 0.8660254037844387076, 1.000000000000000000, 0.8660254037844387076, 1.000000000000000000, 0.8660254037844387076, 1.000000000000000000, 0.8660254037844387076, 1.000000000000000000, 0.8660254037844387076, 1.000000000000000000, 0.8660254037844387076, 1.000000000000000000, 0.8660254037844387076, 1.000000000000000000, 0.8660254037844387076, 1.000000000000000000, 0.8660254037844387076, 1.000000000000000000, 0.8660254037844387076, 1.000000000000000000, 0.8660254037844387076, 1.000000000000000000, 0.8660254037844387076, 1.000000000000000000, 0.8660254037844387076, 1.000000000000000000, 0.8660254037844387076, 1.000000000000000000, 0.8660254037844387076, 1.000000000000000000, 0.8660254037844387076, 1.000000000000000000, 0.8660254037844387076, 1.000000000000000000, 0.8660254037844387076, 1.000000000000000000, 0.8660254037844387076, 1.000000000000000000, 0.8660254037844387076, 1.000000000000000000, 0.8660254037844387076, 1.000000000000000000, 0.8660254037844387076, 1.000000000000000000, 0.8660254037844387076, 1.000000000000000000, 0.8660254037844387076, 1.000000000000000000, 0.8660254037844387076, 1.000000000000000000, 0.8660254037844387076, 1.000000000000000000, 0.8660254037844387076, 1.000000000000000000, 0.8660254037844387076, 1.000000000000000000, 0.8660254037844387076, 1.000000000000000000, 0.8660254037844387076, 1.000000000000000000, 0.8660254037844387076, 1.000000000000000000, 0.8660254037844387076, 1.000000000000000000, 0.8660254037844387076, 1.000000000000000000, 0.8660254037844387076, 1.000000000000000000, 0.8660254037844387076, 1.000000000000000000, 0.8660254037844387076, 1.000000000000000000, 0.8660254037844387076, 1.000000000000000000, 0.8660254037844387076, 1.000000000000000000, 0.8660254037844387076, 1.000000000000000000, 0.8660254037844387076, 1.000000000000000000, 0.8660254037844387076, 1.000000000000000000, 0.8660254037844387076, 1.000000000000000000, 0.8660254037844387076, 1.000000000000000000, 0.8660254037844387076, 1.000000000000000000, 0.8660254037844387076, 1.000000000000000000, 0.8660254037844387076, 1.000000000000000000, 0.8660254037844387076, 1.000000000000000000, 0.8660254037844387076, 1.000000000000000000, 0.8660254037844387076, 1.000000000000000000, 0.8660254037844387076, 1.000000000000000000, 0.8660254037844387076, 1.000000000000000000, 0.8660254037844387076, 1.000000000000000000, 0.8660254037844387076, 1.000000000000000000, 0.8660254037844387076, 1.000000000000000000, 0.8660254037844387076, 1.000000000000000000, 0.8660254037844387076, 1.000000000000000000, 0.8660254037844387076, 1.000000000000000000, 0.8660254037844387076, 1.000000000000000000, 0.8660254037844387076, 1.000000000000000000, 0.8660254037844387076, 1.000000000000000000, 0.8660254037844387076, 1.000000000000000000, 0.8660254037844387076, 1.000000000000000000, 0.8660254037844387076, 1.000000000000000000, 0.8660254037844387076, 1.000000000000000000, 0.8660254037844387076, 1.000000000000000000, 0.8660254037844387076, 1.000000000000000000, 0.8660254037844387076, 1.000000000000000000, 0.8660254037844387076, 1.000000000000000000, 0.8660254037844387076, 1.000000000000000000, 0.8660254037844387076, 1.000000000000000000, 0.8660254037844387076, 1.000000000000000000, 0.8660254037844387076, 1.000000000000000000, 0.8660254037844387076, 1.000000000000000000, 0.8660254037844387076, 1.000000000000000000, 0.8660254037844387076, 1.000000000000000000, 0.8660254037844387076, 1.000000000000000000, 0.8660254037844387076, 1.000000000000000000, 0.8660254037844387076, 1.000000000000000000, 0.8660254037844387076, 1.000000000000000000, 0.8660254037844387076, 1.000000000000000000, 0.8660254037844387076, 1.000000000000000000, 0.8660254037844387076, 1.000000000000000000, 0.8660254037844387076, 1.000000000000000000, 0.8660254037844387076, 1.000000000000000000, 0.8660254037844387076, 1.000000000000000000, 0.8660254037844387076, 1.000000000000000000, 0.8660254037844387076, 1.000000000000000000, 0.8660254037844387076, 1.000000000000000000, 0.8660254037844387076, 1.000000000000000000, 0.8660254037844387076, 1.000000000000000000, 0.8660254037844387076, 1.000000000000000000, 0.8660254037844387076, 1.000000000000000000, 0.8660254037844387076, 1.000000000000000000, 0.8660254037844387076, 1.000000000000000000, 0.8660254037844387076, 1.000000000000000000, 0.8660254037844387076, 1.000000000000000000, 0.8660254037844387076, 1.000000000000000000, 0.8660254037844387076, 1.000000000000000000, 0.8660254037844387076, 1.000000000000000000, 0.8660254037844387076, 1.000000000000000000, 0.8660254037844387076, 1.000000000000000000, 0.8660254037844387076, 1.000000000000000000, 0.8660254037844387076, 1.000000000000000000, 0.8660254037844387076, 1.000000000000000000, 0.8660254037844387076, 1.000000000000000000, 0.8660254037844387076, 1.000000000000000000, 0.8660254037844387076, 1.000000000000000000, 0.8660254037844387076, 1.000000000000000000, 0.8660254037844387076, 1.000000000000000000, 0.8660254037844387076, 1.000000000000000000, 0.8660254037844387076, 1.000000000000000000, 0.8660254037844387076, 1.000000000000000000, 0.8660254037844387076, 1.000000000000000000, 0.8660254037844387076, 1.000000000000000000, 0.8660254037844387076, 1.000000000000000000, 0.8660254037844387076, 1.000000000000000000, 0.8660254037844387076, 1.000000000000000000, 0.8660254037844387076, 1.000000000000000000, 0.8660254037844387076, 1.000000000000000000, 0.8660254037844387076, 1.000000000000000000, 0.8660254037844387076, 1.000000000000000000, 0.8660254037844387076, 1.000000000000000000, 0.8660254037844387076, 1.000000000000000000, 0.8660254037844387076, 1.000000000000000000, 0.8660254037844387076, 1.000000000000000000, 0.8660254037844387076, 1.000000000000000000, 0.8660254037844387076, 1.000000000000000000, 0.8660254037844387076, 1.000000000000000000, 0.8660254037844387076, 1.000000000000000000, 0.8660254037844387076, 1.000000000000000000, 0.8660254037844387076, 1.000000000000000000, 0.8660254037844387076, 1.000000000000000000, 0.8660254037844387076, 1.000000000000000000, 0.8660254037844387076, 1.000000000000000000, 0.8660254037844387076, 1.000000000000000000, 0.8660254037844387076, 1.000000000000000000, 0.8660254037844387076, 1.000000000000000000, 0.8660254037844387076, 1.000000000000000000, 0.8660254037844387076, 1.000000000000000000, 0.8660254037844387076, 1.000000000000000000, 0.8660254037844387076, 1.000000000000000000, 0.8660254037844387076, 1.000000000000000000, 0.8660254037844387076, 1.000000000000000000, 0.8660254037844387076, 1.000000000000000000, 0.8660254037844387076, 1.000000000000000000, 0.8660254037844387076, 1.000000000000000000, 0.8660254037844387076, 1.000000000000000000, 0.8660254037844387076, 1.000000000000000000, 0.8660254037844387076, 1.000000000000000000, 0.8660254037844387076, 1.000000000000000000, 0.8660254037844387076, 1.000000000000000000, 0.8660254037844387076, 1.000000000000000000, 0.8660254037844387076, 1.000000000000000000, 0.8660254037844387076, 1.000000000000000000, 0.8660254037844387076, 1.000000000000000000, 0.8660254037844387076, 1.000000000000000000, 0.8660254037844387076, 1.000000000000000000, 0.8660254037844387076, 1.000000000000000000, 0.8660254037844387076, 1.000000000000000000, 0.8660254037844387076, 1.000000000000000000, 0.8660254037844387076, 1.000000000000000000, 0.8660254037844387076, 1.000000000000000000, 0.8660254037844387076, 1.000000000000000000, 0.8660254037844387076, 1.000000000000000000, 0.8660254037844387076, 1.000000000000000000, 0.8660254037844387076, 1.000000000000000000, 0.8660254037844387076, 1.000000000000000000, 0.8660254037844387076, 1.000000000000000000, 0.8660254037844387076, 1.000000000000000000, 0.8660254037844387076, 1.000000000000000000, 0.8660254037844387076, 1.000000000000000000, 0.8660254037844387076, 1.000000000000000000, 0.8660254037844387076, 1.000000000000000000, 0.8660254037844387076, 1.000000000000000000, 0.8660254037844387076, 1.000000000000000000, 0.8660254037844387076, 1.000000000000000000, 0.8660254037844387076, 1.000000000000000000, 0.8660254037844387076, 1.000000000000000000, 0.8660254037844387076, 1.000000000000000000, 0.8660254037844387076, 1.000000000000000000, 0.8660254037844387076, 1.000000000000000000, 0.8660254037844387076, 1.000000000000000000, 0.8660254037844387076, 1.000000000000000000, 0.8660254037844387076, 1.000000000000000000, 0.8660254037844387076, 1.000000000000000000, 0.8660254037844387076, 1.000000000000000000, 0.8660254037844387076, 1.000000000000000000, 0.8660254037844387076, 1.000000000000000000, 0.8660254037844387076, 1.000000000000000000, 0.8660254037844387076, 1.000000000000000000, 0.8660254037844387076, 1.000000000000000000, 0.8660254037844387076, 1.000000000000000000, 0.8660254037844387076, 1.000000000000000000, 0.8660254037844387076, 1.000000000000000000, 0.8660254037844387076, 1.000000000000000000, 0.8660254037844387076, 1.000000000000000000),
 ( 1.000000000000000000, 0.8660254037844387076, 1.000000000000000000, 0.8660254037844387076, 1.000000000000000000, 0.8660254037844387076, 1.000000000000000000, 0.8660254037844387076, 1.000000000000000000, 0.8660254037844387076, 1.000000000000000000, 0.8660254037844387076, 1.000000000000000000, 0.8660254037844387076, 1.000000000000000000, 0.8660254037844387076, 1.000000000000000000, 0.8660254037844387076, 1.000000000000000000, 0.8660254037844387076, 1.000000000000000000, 0.8660254037844387076, 1.000000000000000000, 0.8660254037844387076, 1.000000000000000000, 0.8660254037844387076, 1.000000000000000000, 0.8660254037844387076, 1.000000000000000000, 0.8660254037844387076, 1.000000000000000000, 0.8660254037844387076, 1.000000000000000000, 0.8660254037844387076, 1.000000000000000000, 0.8660254037844387076, 1.000000000000000000, 0.8660254037844387076, 1.000000000000000000, 0.8660254037844387076, 1.000000000000000000, 0.8660254037844387076, 1.000000000000000000, 0.8660254037844387076, 1.000000000000000000, 0.8660254037844387076, 1.000000000000000000, 0.8660254037844387076, 1.000000000000000000, 0.8660254037844387076, 1.000000000000000000, 0.8660254037844387076, 1.000000000000000000, 0.8660254037844387076, 1.000000000000000000, 0.8660254037844387076, 1.000000000000000000, 0.8660254037844387076, 1.000000000000000000, 0.8660254037844387076, 1.000000000000000000, 0.8660254037844387076, 1.000000000000000000, 0.8660254037844387076, 1.000000000000000000, 0.8660254037844387076, 1.000000000000000000, 0.8660254037844387076, 1.000000000000000000, 0.8660254037844387076, 1.000000000000000000, 0.8660254037844387076, 1.000000000000000000, 0.8660254037844387076, 1.000000000000000000, 0.8660254037844387076, 1.000000000000000000, 0.8660254037844387076, 1.000000000000000000, 0.8660254037844387076, 1.000000000000000000, 0.8660254037844387076, 1.000000000000000000, 0.8660254037844387076, 1.000000000000000000, 0.8660254037844387076, 1.000000000000000000, 0.8660254037844387076, 1.000000000000000000, 0.8660254037844387076, 1.000000000000000000, 0.8660254037844387076, 1.000000000000000000, 0.8660254037844387076, 1.000000000000000000, 0.8660254037844387076, 1.000000000000000000, 0.8660254037844387076, 1.000000000000000000, 0.8660254037844387076, 1.000000000000000000, 0.8660254037844387076, 1.000000000000000000, 0.8660254037844387076, 1.000000000000000000, 0.8660254037844387076, 1.000000000000000000, 0.8660254037844387076, 1.000000000000000000, 0.8660254037844387076, 1.000000000000000000, 0.8660254037844387076, 1.000000000000000000, 0.8660254037844387076, 1.000000000000000000, 0.8660254037844387076, 1.000000000000000000, 0.8660254037844387076, 1.000000000000000000, 0.8660254037844387076, 1.000000000000000000, 0.8660254037844387076, 1.000000000000000000, 0.8660254037844387076, 1.000000000000000000, 0.8660254037844387076, 1.000000000000000000, 0.8660254037844387076, 1.000000000000000000, 0.8660254037844387076, 1.000000000000000000, 0.8660254037844387076, 1.000000000000000000, 0.8660254037844387076, 1.000000000000000000, 0.8660254037844387076, 1.000000000000000000, 0.8660254037844387076, 1.000000000000000000, 0.8660254037844387076, 1.000000000000000000, 0.8660254037844387076, 1.000000000000000000, 0.8660254037844387076, 1.000000000000000000, 0.8660254037844387076, 1.000000000000000000, 0.8660254037844387076, 1.000000000000000000, 0.8660254037844387076, 1.000000000000000000, 0.8660254037844387076, 1.000000000000000000, 0.8660254037844387076, 1.000000000000000000, 0.8660254037844387076, 1.000000000000000000, 0.8660254037844387076, 1.000000000000000000, 0.8660254037844387076, 1.000000000000000000, 0.8660254037844387076, 1.000000000000000000, 0.8660254037844387076, 1.000000000000000000, 0.8660254037844387076, 1.000000000000000000, 0.8660254037844387076, 1.000000000000000000, 0.8660254037844387076, 1.000000000000000000, 0.8660254037844387076, 1.000000000000000000, 0.8660254037844387076, 1.000000000000000000, 0.8660254037844387076, 1.000000000000000000, 0.8660254037844387076, 1.000000000000000000, 0.8660254037844387076, 1.000000000000000000, 0.8660254037844387076, 1.000000000000000000, 0.8660254037844387076, 1.000000000000000000, 0.8660254037844387076, 1.000000000000000000, 0.8660254037844387076, 1.000000000000000000, 0.8660254037844387076, 1.000000000000000000, 0.8660254037844387076, 1.000000000000000000, 0.8660254037844387076, 1.000000000000000000, 0.8660254037844387076, 1.000000000000000000, 0.8660254037844387076, 1.000000000000000000, 0.8660254037844387076, 1.000000000000000000, 0.8660254037844387076, 1.000000000000000000, 0.8660254037844387076, 1.000000000000000000, 0.8660254037844387076, 1.000000000000000000, 0.8660254037844387076, 1.000000000000000000, 0.8660254037844387076, 1.000000000000000000, 0.8660254037844387076, 1.000000000000000000, 0.8660254037844387076, 1.000000000000000000, 0.8660254037844387076, 1.000000000000000000, 0.8660254037844387076, 1.000000000000000000, 0.8660254037844387076, 1.000000000000000000, 0.8660254037844387076, 1.000000000000000000, 0.8660254037844387076, 1.000000000000000000, 0.8660254037844387076, 1.000000000000000000, 0.8660254037844387076, 1.000000000000000000, 0.8660254037844387076, 1.000000000000000000, 0.8660254037844387076, 1.000000000000000000, 0.8660254037844387076, 1.000000000000000000, 0.8660254037844387076, 1.000000000000000000, 0.8660254037844387076, 1.000000000000000000, 0.8660254037844387076, 1.000000000000000000, 0.8660254037844387076, 1.000000000000000000, 0.8660254037844387076, 1.000000000000000000, 0.8660254037844387076, 1.000000000000000000, 0.8660254037844387076, 1.000000000000000000, 0.8660254037844387076, 1.000000000000000000, 0.8660254037844387076, 1.000000000000000000, 0.8660254037844387076, 1.000000000000000000, 0.8660254037844387076, 1.000000000000000000, 0.8660254037844387076, 1.000000000000000000, 0.8660254037844387076, 1.000000000000000000, 0.8660254037844387076, 1.000000000000000000, 0.8660254037844387076, 1.000000000000000000, 0.8660254037844387076, 1.000000000000000000, 0.8660254037844387076, 1.000000000000000000, 0.8660254037844387076, 1.000000000000000000, 0.8660254037844387076, 1.000000000000000000, 0.8660254037844387076, 1.000000000000000000, 0.8660254037844387076, 1.000000000000000000, 0.8660254037844387076, 1.000000000000000000, 0.8660254037844387076, 1.000000000000000000, 0.8660254037844387076, 1.000000000000000000, 0.8660254037844387076, 1.000000000000000000, 0.8660254037844387076, 1.000000000000000000, 0.8660254037844387076, 1.000000000000000000, 0.8660254037844387076, 1.000000000000000000, 0.8660254037844387076, 1.000000000000000000, 0.8660254037844387076, 1.000000000000000000, 0.8660254037844387076, 1.000000000000000000, 0.8660254037844387076, 1.000000000000000000, 0.8660254037844387076, 1.000000000000000000, 0.8660254037844387076, 1.000000000000000000, 0.8660254037844387076, 1.000000000000000000, 0.8660254037844387076, 1.000000000000000000, 0.8660254037844387076, 1.000000000000000000, 0.8660254037844387076, 1.000000000000000000, 0.8660254037844387076, 1.000000000000000000, 0.8660254037844387076, 1.000000000000000000, 0.8660254037844387076, 1.000000000000000000, 0.8660254037844387076, 1.000000000000000000, 0.8660254037844387076, 1.000000000000000000, 0.8660254037844387076, 1.000000000000000000, 0.8660254037844387076, 1.000000000000000000, 0.8660254037844387076, 1.000000000000000000, 0.8660254037844387076, 1.000000000000000000, 0.8660254037844387076, 1.000000000000000000, 0.8660254037844387076, 1.000000000000000000, 0.8660254037844387076, 1.000000000000000000, 0.8660254037844387076, 1.000000000000000000, 0.8660254037844387076, 1.000000000000000000, 0.8660254037844387076, 1.000000000000000000, 0.8660254037844387076, 1.000000000000000000, 0.8660254037844387076, 1.000000000000000000, 0.8660254037844387076, 1.000000000000000000, 0.8660254037844387076, 1.000000000000000000, 0.8660254037844387076, 1.000000000000000000, 0.8660254037844387076, 1.000000000000000000, 0.8660254037844387076, 1.000000000000000000, 0.8660254037844387076, 1.000000000000000000, 0.8660254037844387076, 1.000000000000000000, 0.8660254037844387076, 1.000000000000000000, 0.8660254037844387076, 1.000000000000000000, 0.8660254037844387076, 1.000000000000000000, 0.8660254037844387076, 1.000000000000000000, 0.8660254037844387076, 1.000000000000000000, 0.8660254037844387076, 1.000000000000000000, 0.8660254037844387076, 1.000000000000000000, 0.8660254037844387076, 1.000000000000000000, 0.8660254037844387076, 1.000000000000000000, 0.8660254037844387076, 1.000000000000000000, 0.8660254037844387076, 1.000000000000000000, 0.8660254037844387076, 1.000000000000000000, 0.8660254037844387076, 1.000000000000000000, 0.8660254037844387076, 1.000000000000000000, 0.8660254037844387076, 1.000000000000000000, 0.8660254037844387076, 1.000000000000000000, 0.8660254037844387076, 1.000000000000000000, 0.8660254037844387076, 1.000000000000000000, 0.8660254037844387076, 1.000000000000000000, 0.8660254037844387076, 1.000000000000000000, 0.8660254037844387076, 1.000000000000000000, 0.8660254037844387076, 1.000000000000000000, 0.8660254037844387076, 1.000000000000000000, 0.8660254037844387076, 1.000000000000000000, 0.8660254037844387076, 1.000000000000000000, 0.8660254037844387076, 1.000000000000000000, 0.8660254037844387076, 1.000000000000000000, 0.8660254037844387076, 1.000000000000000000, 0.8660254037844387076, 1.000000000000000000, 0.8660254037844387076, 1.000000000000000000, 0.8660254037844387076, 1.000000000000000000, 0.8660254037844387076, 1.000000000000000000, 0.8660254037844387076, 1.000000000000000000, 0.8660254037844387076, 1.000000000000000000, 0.8660254037844387076, 1.000000000000000000, 0.8660254037844387076, 1.000000000000000000, 0.8660254037844387076, 1.000000000000000000, 0.8660254037844387076, 1.000000000000000000, 0.8660254037844387076, 1.000000000000000000, 0.8660254037844387076, 1.000000000000000000, 0.8660254037844387076, 1.000000000000000000, 0.8660254037844387076, 1.000000000000000000, 0.8660254037844387076, 1.000000000000000000, 0.8660254037844387076, 1.000000000000000000, 0.8660254037844387076, 1.000000000000000000, 0.8660254037844387076, 1.000000000000000000, 0.8660254037844387076, 1.000000000000000000, 0.8660254037844387076, 1.000000000000000000, 0.8660254037844387076, 1.000000000000000000, 0.8660254037844387076, 1.000000000000000000, 0.8660254037844387076, 1.000000000000000000, 0.8660254037844387076, 1.000000000000000000, 0.8660254037844387076, 1.000000000000000000, 0.8660254037844387076, 1.000000000000000000, 0.8660254037844387076, 1.000000000000000000, 0.8660254037844387076, 1.000000000000000000, 0.8660254037844387076, 1.000000000000000000, 0.8660254037844387076, 1.000000000000000000, 0.8660254037844387076, 1.000000000000000000, 0.8660254037844387076, 1.000000000000000000, 0.8660254037844387076, 1.000000000000000000, 0.8660254037844387076, 1.000000000000000000, 0.8660254037844387076, 1.000000000000000000, 0.8660254037844387076, 1.000000000000000000, 0.8660254037844387076, 1.000000000000000000, 0.8660254037844387076, 1.000000000000000000, 0.8660254037844387076, 1.000000000000000000, 0.8660254037844387076, 1.000000000000000000, 0.8660254037844387076, 1.000000000000000000, 0.8660254037844387076, 1.000000000000000000, 0.8660254037844387076, 1.000000000000000000, 0.8660254037844387076, 1.000000000000000000, 0.8660254037844387076, 1.000000000000000000, 0.8660254037844387076, 1.000000000000000000, 0.8660254037844387076, 1.000000000000000000, 0.8660254037844387076, 1.000000000000000000, 0.8660254037844387076, 1.000000000000000000, 0.8660254037844387076, 1.000000000000000000, 0.8660254037844387076, 1.000000000000000000, 0.8660254037844387076, 1.000000000000000000, 0.8660254037844387076, 1.000000000000000000, 0.8660254037844387076, 1.000000000000000000, 0.8660254037844387076, 1.000000000000000000, 0.8660254037844387076, 1.000000000000000000, 0.8660254037844387076, 1.000000000000000000, 0.8660254037844387076, 1.000000000000000000, 0.8660254037844387076, 1.000000000000000000, 0.8660254037844387076, 1.000000000000000000, 0.8660254037844387076, 1.000000000000000000, 0.8660254037844387076, 1.000000000000000000, 0.8660254037844387076, 1.000000000000000000, 0.8660254037844387076, 1.000000000000000000, 0.8660254037844387076, 1.000000000000000000, 0.8660254037844387076, 1.000000000000000000, 0.8660254037844387076, 1.000000000000000000, 0.8660254037844387076, 1.000000000000000000, 0.8660254037844387076, 1.000000000000000000, 0.8660254037844387076, 1.000000000000000000, 0.8660254037844387076, 1.000000000000000000, 0.8660254037844387076, 1.000000000000000000, 0.8660254037844387076, 1.000000000000000000, 0.8660254037844387076, 1.000000000000000000, 0.8660254037844387076, 1.000000000000000000, 0.8660254037844387076, 1.000000000000000000, 0.8660254037844387076, 1.000000000000000000, 0.8660254037844387076, 1.000000000000000000, 0.8660254037844387076, 1.000000000000000000, 0.8660254037844387076, 1.000000000000000000, 0.8660254037844387076, 1.000000000000000000, 0.8660254037844387076, 1.000000000000000000, 0.8660254037844387076, 1.000000000000000000, 0.8660254037844387076, 1.000000000000000000, 0.8660254037844387076, 1.000000000000000000, 0.8660254037844387076, 1.000000000000000000, 0.8660254037844387076, 1.000000000000000000, 0.8660254037844387076, 1.000000000000000000, 0.8660254037844387076, 1.000000000000000000, 0.8660254037844387076, 1.000000000000000000, 0.8660254037844387076, 1.000000000000000000, 0.8660254037844387076, 1.000000000000000000, 0.8660254037844387076, 1.000000000000000000, 0.8660254037844387076, 1.000000000000000000, 0.8660254037844387076, 1.000000000000000000, 0.8660254037844387076, 1.000000000000000000, 0.8660254037844387076, 1.000000000000000000, 0.8660254037844387076, 1.000000000000000000, 0.8660254037844387076, 1.000000000000000000, 0.8660254037844387076, 1.000000000000000000, 0.8660254037844387076, 1.000000000000000000, 0.8660254037844387076, 1.000000000000000000, 0.8660254037844387076, 1.000000000000000000, 0.8660254037844387076, 1.000000000000000000, 0.8660254037844387076, 1.000000000000000000, 0.8660254037844387076, 1.000000000000000000, 0.8660254037844387076, 1.000000000000000000, 0.8660254037844387076, 1.000000000000000000, 0.8660254037844387076, 1.000000000000000000, 0.8660254037844387076, 1.000000000000000000, 0.8660254037844387076, 1.000000000000000000, 0.8660254037844387076, 1.000000000000000000, 0.8660254037844387076, 1.000000000000000000, 0.8660254037844387076, 1.000000000000000000, 0.8660254037844387076, 1.000000000000000000, 0.8660254037844387076, 1.000000000000000000, 0.8660254037844387076, 1.000000000000000000, 0.8660254037844387076, 1.000000000000000000, 0.8660254037844387076, 1.000000000000000000, 0.8660254037844387076, 1.000000000000000000, 0.8660254037844387076, 1.000000000000000000, 0.8660254037844387076, 1.000000000000000000, 0.8660254037844387076, 1.000000000000000000, 0.8660254037844387076, 1.000000000000000000, 0.8660254037844387076, 1.000000000000000000, 0.8660254037844387076, 1.000000000000000000, 0.8660254037844387076, 1.000000000000000000, 0.8660254037844387076, 1.000000000000000000, 0.8660254037844387076, 1.000000000000000000, 0.8660254037844387076, 1.000000000000000000, 0.8660254037844387076, 1.000000000000000000, 0.8660254037844387076, 1.000000000000000000, 0.8660254037844387076, 1.000000000000000000, 0.8660254037844387076, 1.000000000000000000, 0.8660254037844387076, 1.000000000000000000, 0.8660254037844387076, 1.000000000000000000, 0.8660254037844387076, 1.000000000000000000, 0.8660254037844387076, 1.000000000000000000, 0.8660254037844387076, 1.000000000000000000, 0.8660254037844387076, 1.000000000000000000, 0.8660254037844387076, 1.000000000000000000, 0.8660254037844387076, 1.000000000000000000, 0.8660254037844387076, 1.000000000000000000, 0.8660254037844387076, 1.000000000000000000, 0.8660254037844387076, 1.000000000000000000, 0.8660254037844387076, 1.000000000000000000, 0.8660254037844387076, 1.000000000000000000, 0.8660254037844387076, 1.000000000000000000, 0.8660254037844387076, 1.000000000000000000, 0.8660254037844387076, 1.000000000000000000, 0.8660254037844387076, 1.000000000000000000, 0.8660254037844387076, 1.000000000000000000, 0.8660254037844387076, 1.000000000000000000, 0.8660254037844387076, 1.000000000000000000, 0.8660254037844387076, 1.000000000000000000, 0.8660254037844387076, 1.000000000000000000, 0.8660254037844387076, 1.000000000000000000, 0.8660254037844387076, 1.000000000000000000, 0.8660254037844387076, 1.000000000000000000, 0.8660254037844387076, 1.000000000000000000, 0.8660254037844387076, 1.000000000000000000, 0.8660254037844387076, 1.000000000000000000, 0.8660254037844387076, 1.000000000000000000, 0.8660254037844387076, 1.000000000000000000, 0.8660254037844387076, 1.000000000000000000, 0.8660254037844387076, 1.000000000000000000, 0.8660254037844387076, 1.000000000000000000, 0.8660254037844387076, 1.000000000000000000, 0.8660254037844387076, 1.000000000000000000, 0.8660254037844387076, 1.000000000000000000, 0.8660254037844387076, 1.000000000000000000, 0.8660254037844387076, 1.000000000000000000, 0.8660254037844387076, 1.000000000000000000, 0.8660254037844387076, 1.000000000000000000, 0.8660254037844387076, 1.000000000000000000, 0.8660254037844387076, 1.000000000000000000, 0.8660254037844387076, 1.000000000000000000, 0.8660254037844387076, 1.000000000000000000, 0.8660254037844387076, 1.000000000000000000, 0.8660254037844387076, 1.000000000000000000, 0.8660254037844387076, 1.000000000000000000, 0.8660254037844387076, 1.000000000000000000, 0.8660254037844387076, 1.000000000000000000, 0.8660254037844387076, 1.000000000000000000, 0.8660254037844387076, 1.000000000000000000, 0.8660254037844387076, 1.000000000000000000, 0.8660254037844387076, 1.000000000000000000, 0.8660254037844387076, 1.000000000000000000, 0.8660254037844387076, 1.000000000000000000, 0.8660254037844387076, 1.000000000000000000, 0.8660254037844387076, 1.000000000000000000, 0.8660254037844387076, 1.000000000000000000, 0.8660254037844387076, 1.000000000000000000, 0.8660254037844387076, 1.000000000000000000, 0.8660254037844387076, 1.000000000000000000, 0.8660254037844387076, 1.000000000000000000, 0.8660254037844387076, 1.000000000000000000, 0.8660254037844387076, 1.000000000000000000, 0.8660254037844387076, 1.000000000000000000, 0.8660254037844387076, 1.000000000000000000, 0.8660254037844387076, 1.000000000000000000, 0.8660254037844387076, 1.000000000000000000, 0.8660254037844387076, 1.000000000000000000, 0.8660254037844387076, 1.000000000000000000, 0.8660254037844387076, 1.000000000000000000, 0.8660254037844387076, 1.000000000000000000, 0.8660254037844387076, 1.000000000000000000, 0.8660254037844387076, 1.000000000000000000, 0.8660254037844387076, 1.000000000000000000, 0.8660254037844387076, 1.000000000000000000, 0.8660254037844387076, 1.000000000000000000, 0.8660254037844387076, 1.000000000000000000, 0.8660254037844387076, 1.000000000000000000, 0.8660254037844387076, 1.000000000000000000, 0.8660254037844387076, 1.000000000000000000, 0.8660254037844387076, 1.000000000000000000, 0.8660254037844387076, 1.000000000000000000, 0.8660254037844387076, 1.000000000000000000, 0.8660254037844387076, 1.000000000000000000, 0.8660254037844387076, 1.000000000000000000, 0.8660254037844387076, 1.000000000000000000, 0.8660254037844387076, 1.000000000000000000, 0.8660254037844387076, 1.000000000000000000, 0.8660254037844387076, 1.000000000000000000, 0.8660254037844387076, 1.000000000000000000, 0.8660254037844387076, 1.000000000000000000, 0.8660254037844387076, 1.000000000000000000, 0.8660254037844387076, 1.000000000000000000, 0.8660254037844387076, 1.000000000000000000, 0.8660254037844387076, 1.000000000000000000, 0.8660254037844387076, 1.000000000000000000, 0.8660254037844387076, 1.000000000000000000, 0.8660254037844387076, 1.000000000000000000, 0.8660254037844387076, 1.000000000000000000, 0.8660254037844387076, 1.000000000000000000, 0.8660254037844387076, 1.000000000000000000, 0.8660254037844387076, 1.000000000000000000, 0.8660254037844387076, 1.000000000000000000, 0.8660254037844387076, 1.000000000000000000, 0.8660254037844387076, 1.000000000000000000, 0.8660254037844387076, 1.000000000000000000, 0.8660254037844387076, 1.000000000000000000, 0.8660254037844387076, 1.000000000000000000, 0.8660254037844387076, 1.000000000000000000, 0.8660254037844387076, 1.000000000000000000, 0.8660254037844387076, 1.000000000000000000, 0.8660254037844387076, 1.000000000000000000, 0.8660254037844387076, 1.000000000000000000, 0.8660254037844387076, 1.000000000000000000, 0.8660254037844387076, 1.000000000000000000, 0.8660254037844387076, 1.000000000000000000, 0.8660254037844387076, 1.000000000000000000, 0.8660254037844387076, 1.000000000000000000, 0.8660254037844387076, 1.000000000000000000, 0.8660254037844387076, 1.000000000000000000, 0.8660254037844387076, 1.000000000000000000, 0.8660254037844387076, 1.000000000000000000, 0.8660254037844387076, 1.000000000000000000, 0.8660254037844387076, 1.000000000000000000, 0.8660254037844387076, 1.000000000000000000, 0.8660254037844387076, 1.000000000000000000, 0.8660254037844387076, 1.000000000000000000, 0.8660254037844387076, 1.000000000000000000, 0.8660254037844387076, 1.000000000000000000, 0.8660254037844387076, 1.000000000000000000, 0.8660254037844387076, 1.000000000000000000, 0.8660254037844387076, 1.000000000000000000, 0.8660254037844387076, 1.000000000000000000, 0.8660254037844387076, 1.000000000000000000, 0.8660254037844387076, 1.000000000000000000, 0.8660254037844387076, 1.000000000000000000, 0.8660254037844387076, 1.000000000000000000, 0.8660254037844387076, 1.000000000000000000, 0.8660254037844387076, 1.000000000000000000, 0.8660254037844387076, 1.000000000000000000, 0.8660254037844387076, 1.000000000000000000, 0.8660254037844387076, 1.000000000000000000, 0.8660254037844387076, 1.000000000000000000, 0.8660254037844387076, 1.000000000000000000, 0.8660254037844387076, 1.000000000000000000, 0.8660254037844387076, 1.000000000000000000, 0.8660254037844387076, 1.000000000000000000, 0.8660254037844387076, 1.000000000000000000, 0.8660254037844387076, 1.000000000000000000, 0.8660254037844387076, 1.000000000000000000, 0.8660254037844387076, 1.000000000000000000, 0.8660254037844387076, 1.000000000000000000, 0.8660254037844387076, 1.000000000000000000, 0.8660254037844387076, 1.000000000000000000, 0.8660254037844387076, 1.000000000000000000, 0.8660254037844387076, 1.000000000000000000, 0.8660254037844387076, 1.000000000000000000, 0.8660254037844387076, 1.000000000000000000, 0.8660254037844387076, 1.000000000000000000, 0.8660254037844387076, 1.000000000000000000, 0.8660254037844387076, 1.000000000000000000, 0.8660254037844387076, 1.000000000000000000, 0.8660254037844387076, 1.000000000000000000, 0.8660254037844387076, 1.000000000000000000, 0.8660254037844387076, 1.000000000000000000, 0.8660254037844387076, 1.000000000000000000, 0.8660254037844387076, 1.000000000000000000, 0.8660254037844387076, 1.000000000000000000, 0.8660254037844387076, 1.000000000000000000, 0.8660254037844387076, 1.000000000000000000, 0.8660254037844387076, 1.000000000000000000, 0.8660254037844387076, 1.000000000000000000, 0.8660254037844387076, 1.000000000000000000, 0.8660254037844387076, 1.000000000000000000, 0.8660254037844387076, 1.000000000000000000, 0.8660254037844387076, 1.000000000000000000, 0.8660254037844387076, 1.000000000000000000, 0.8660254037844387076, 1.000000000000000000, 0.8660254037844387076, 1.000000000000000000, 0.8660254037844387076, 1.000000000000000000, 0.8660254037844387076, 1.000000000000000000, 0.8660254037844387076, 1.000000000000000000, 0.8660254037844387076, 1.000000000000000000, 0.8660254037844387076, 1.000000000000000000, 0.8660254037844387076, 1.000000000000000000, 0.8660254037844387076, 1.000000000000000000, 0.8660254037844387076, 1.000000000000000000, 0.8660254037844387076, 1.000000000000000000, 0.8660254037844387076, 1.000000000000000000, 0.8660254037844387076, 1.000000000000000000, 0.8660254037844387076, 1.000000000000000000, 0.8660254037844387076, 1.000000000000000000, 0.8660254037844387076, 1.000000000000000000, 0.8660254037844387076, 1.000000000000000000, 0.8660254037844387076, 1.000000000000000000, 0.8660254037844387076, 1.000000000000000000, 0.8660254037844387076, 1.000000000000000000, 0.8660254037844387076, 1.000000000000000000) ) ) 
 REPRESENTATION_ITEM ( '' )  SURFACE ( )  );
#6293 = EDGE_CURVE ( 'NONE', #20611, #26866, #9125, .T. ) ;
#6294 = DIRECTION ( 'NONE',  ( 7.147005652999508048E-36, -5.642372883946980038E-36, -1.000000000000000000 ) ) ;
#6295 = CARTESIAN_POINT ( 'NONE',  ( -4.763139720814407951, -2.750000000000016431, -131.5000000000000000 ) ) ;
#6296 = CARTESIAN_POINT ( 'NONE',  ( 124.9999999999999432, -70.00000000000000000, 8.000000000000007105 ) ) ;
#6297 = CARTESIAN_POINT ( 'NONE',  ( 104.7401757384971859, -1.662314916401979259, -0.8208299140997361576 ) ) ;
#6298 = ORIENTED_EDGE ( 'NONE', *, *, #29132, .F. ) ;
#6299 = CARTESIAN_POINT ( 'NONE',  ( 23.87500000000009237, 5.551115123125782702E-14, 2.649519052838333888 ) ) ;
#6300 = LINE ( 'NONE', #17866, #18532 ) ;
#6301 = EDGE_CURVE ( 'NONE', #1053, #17791, #7817, .T. ) ;
#6302 = CARTESIAN_POINT ( 'NONE',  ( 142.6086002691896226, -2.071067811865468400, -4.999999999999989342 ) ) ;
#6303 = ORIENTED_EDGE ( 'NONE', *, *, #22118, .F. ) ;
#6304 = CARTESIAN_POINT ( 'NONE',  ( 10.97617513459489835, -1.035533905932629173, -2.499999999999904521 ) ) ;
#6305 = CARTESIAN_POINT ( 'NONE',  ( 5.412658773652739619, 3.124999999999988898, -112.3169872981077901 ) ) ;
#6306 = CARTESIAN_POINT ( 'NONE',  ( 135.0000000000000568, 5.527055845544526669, -1.966580164914623952 ) ) ;
#6307 = CARTESIAN_POINT ( 'NONE',  ( 119.7113248654050750, 2.000000000000001776, 1.110223024625156540E-13 ) ) ;
#6308 = ORIENTED_EDGE ( 'NONE', *, *, #17222, .T. ) ;
#6309 = DIRECTION ( 'NONE',  ( 0.000000000000000000, -1.000000000000000000, -8.881784197001264156E-16 ) ) ;
#6310 = CARTESIAN_POINT ( 'NONE',  ( 140.2500000000000284, -6.000000000000005329, 0.000000000000000000 ) ) ;
#6311 = VERTEX_POINT ( 'NONE', #12625 ) ;
#6312 = EDGE_LOOP ( 'NONE', ( #10524, #29794, #17806, #19040 ) ) ;
#6313 = CARTESIAN_POINT ( 'NONE',  ( -4.999999999999990230, -24.99999999999999289, -8.000000000000007105 ) ) ;
#6314 = CARTESIAN_POINT ( 'NONE',  ( 6.350852961086080661, -9.614813431917819062E-14, -51.37500000000002132 ) ) ;
#6315 = CARTESIAN_POINT ( 'NONE',  ( 23.81250000000003553, 0.8284271247463557142, -2.000000000000151879 ) ) ;
#6316 = CARTESIAN_POINT ( 'NONE',  ( -5.196152422706601826, 2.999999999999975131, -120.0386751345948255 ) ) ;
#6317 = CARTESIAN_POINT ( 'NONE',  ( 3.608439182435180470, 6.249999999999982236, -65.05801270189225249 ) ) ;
#6318 = CARTESIAN_POINT ( 'NONE',  ( 152.7976497308104058, 0.000000000000000000, 5.000000000000004441 ) ) ;
#6319 = CARTESIAN_POINT ( 'NONE',  ( -5.999999999999963585, -1.487416814333745711E-14, -122.9136751345948255 ) ) ;
#6320 = CARTESIAN_POINT ( 'NONE',  ( 12.10117513459494276, 1.035533905932929599, -2.499999999999964473 ) ) ;
#6321 = CARTESIAN_POINT ( 'NONE',  ( 16.97617513459493566, -1.035533905932568999, -2.499999999999904521 ) ) ;
#6322 = EDGE_CURVE ( 'NONE', #25961, #13568, #2313, .T. ) ;
#6323 = DIRECTION ( 'NONE',  ( -7.147005652999508048E-36, 5.642372883946980038E-36, 1.000000000000000000 ) ) ;
#6324 = ADVANCED_FACE ( 'NONE', ( #13244 ), #20278, .T. ) ;
#6325 = CARTESIAN_POINT ( 'NONE',  ( -3.175426480542816066, -5.500000000000057732, -129.8750000000000284 ) ) ;
#6326 = CARTESIAN_POINT ( 'NONE',  ( 5.412658773652739619, 3.124999999999988898, -147.6830127018922099 ) ) ;
#6327 = LINE ( 'NONE', #3863, #27749 ) ;
#6328 = VERTEX_POINT ( 'NONE', #16008 ) ;
#6329 = CARTESIAN_POINT ( 'NONE',  ( 0.000000000000000000, 5.499999999999991118, -66.00000000000000000 ) ) ;
#6330 = CARTESIAN_POINT ( 'NONE',  ( 0.000000000000000000, 0.000000000000000000, 0.000000000000000000 ) ) ;
#6331 = DIRECTION ( 'NONE',  ( 0.000000000000000000, 0.000000000000000000, -1.000000000000000000 ) ) ;
#6332 =( BOUNDED_CURVE ( )  B_SPLINE_CURVE ( 2, ( #7411, #30151, #16817, #36, #2643, #18811, #12062, #11761, #18969 ),
 .UNSPECIFIED., .F., .T. ) 
 B_SPLINE_CURVE_WITH_KNOTS ( ( 3, 2, 2, 2, 3 ),
 ( 0.9638888888888889062, 0.9648148148148147918, 0.9666666666666666741, 0.9685185185185185563, 0.9694444444444444420 ),
 .UNSPECIFIED. ) 
 CURVE ( )  GEOMETRIC_REPRESENTATION_ITEM ( )  RATIONAL_B_SPLINE_CURVE ( ( 0.9330127018922194093, 0.9330127018922194093, 1.000000000000000000, 0.8660254037844388186, 1.000000000000000000, 0.8660254037844388186, 1.000000000000000000, 0.9330127018922194093, 0.9330127018922194093 ) ) 
 REPRESENTATION_ITEM ( '' )  );
#6333 = ORIENTED_EDGE ( 'NONE', *, *, #7383, .T. ) ;
#6334 = CARTESIAN_POINT ( 'NONE',  ( 143.7187500000000284, 2.485281374238556218, -6.000000000000005329 ) ) ;
#6335 = CARTESIAN_POINT ( 'NONE',  ( 141.6636751345948255, 0.000000000000000000, 5.500000000000005329 ) ) ;
#6336 = DIRECTION ( 'NONE',  ( 1.000000000000000000, 1.067522139062651904E-16, -0.000000000000000000 ) ) ;
#6337 = CARTESIAN_POINT ( 'NONE',  ( 140.1562500000000853, -6.000000000000005329, 2.485281374238555774 ) ) ;
#6338 = DIRECTION ( 'NONE',  ( 1.000000000000000000, 0.000000000000000000, 0.000000000000000000 ) ) ;
#6339 = VERTEX_POINT ( 'NONE', #29467 ) ;
#6340 = CARTESIAN_POINT ( 'NONE',  ( -4.763139720814407951, -2.750000000000016431, -145.0000000000000284 ) ) ;
#6341 = VERTEX_POINT ( 'NONE', #17996 ) ;
#6342 = CARTESIAN_POINT ( 'NONE',  ( 15.00000000000012434, 2.000000000000112799, 0.000000000000000000 ) ) ;
#6343 = VERTEX_POINT ( 'NONE', #18141 ) ;
#6344 = CARTESIAN_POINT ( 'NONE',  ( 0.000000000000000000, 5.499999999999991118, -72.00000000000001421 ) ) ;
#6345 = CARTESIAN_POINT ( 'NONE',  ( 18.64882486540528106, 2.500000000000084821, -1.035533905932869425 ) ) ;
#6346 = CARTESIAN_POINT ( 'NONE',  ( 3.608439182435180470, -6.249999999999997335, -89.55801270189223828 ) ) ;
#6347 = ORIENTED_EDGE ( 'NONE', *, *, #25651, .T. ) ;
#6348 = DIRECTION ( 'NONE',  ( -7.147005652999508048E-36, 5.642372883946980038E-36, 1.000000000000000000 ) ) ;
#6349 =( NAMED_UNIT ( * ) PLANE_ANGLE_UNIT ( ) SI_UNIT ( $, .RADIAN. ) );
#6350 = CARTESIAN_POINT ( 'NONE',  ( 0.000000000000000000, 0.000000000000000000, 0.000000000000000000 ) ) ;
#6351 = CARTESIAN_POINT ( 'NONE',  ( 9.433704689814137012, 0.000000000000000000, 0.000000000000000000 ) ) ;
#6352 = CARTESIAN_POINT ( 'NONE',  ( 24.52451905283846401, 1.480436431285038258E-13, 2.475480947161601275 ) ) ;
#6353 = ITEM_DEFINED_TRANSFORMATION ( 'NONE', 'NONE', #10996,  #18805 ) ;
#6354 = ADVANCED_FACE ( 'NONE', ( #11071 ), #20418, .F. ) ;
#6355 = CARTESIAN_POINT ( 'NONE',  ( 3.175426480543072749, 5.499999999999865885, -159.1250000000000284 ) ) ;
#6356 = CARTESIAN_POINT ( 'NONE',  ( 139.5000000000000284, -8.798545334315209132, -8.160000000000007248 ) ) ;
#6357 = CARTESIAN_POINT ( 'NONE',  ( 3.464101615137852974, 5.999999999999884537, -49.33632486540521711 ) ) ;
#6358 = AXIS2_PLACEMENT_3D ( 'NONE', #12044, #2916, #14051 ) ;
#6359 = CARTESIAN_POINT ( 'NONE',  ( -3.175426480542816066, -5.500000000000057732, -86.37500000000005684 ) ) ;
#6360 = DIRECTION ( 'NONE',  ( 0.000000000000000000, -5.551115123125767911E-17, 1.000000000000000000 ) ) ;
#6361 = CARTESIAN_POINT ( 'NONE',  ( -4.763139720814407951, -2.750000000000016431, -70.00000000000000000 ) ) ;
#6362 = CARTESIAN_POINT ( 'NONE',  ( -5.196152422706573404, -3.000000000000002665, -120.7113248654052597 ) ) ;
#6363 = CARTESIAN_POINT ( 'NONE',  ( 148.4211002691896226, -4.999999999999989342, -2.071067811865468400 ) ) ;
#6364 = CARTESIAN_POINT ( 'NONE',  ( 5.196152422706629359, 3.000000000000002665, -106.4613248654052740 ) ) ;
#6365 = CARTESIAN_POINT ( 'NONE',  ( 0.000000000000000000, -5.999999999999991118, -175.0386751345948255 ) ) ;
#6366 = CARTESIAN_POINT ( 'NONE',  ( 135.5000000000000284, -8.500000000000007105, -7.500000000000007105 ) ) ;
#6367 = CARTESIAN_POINT ( 'NONE',  ( 18.87500000000008527, 1.414213562373256572, -1.414213562373090038 ) ) ;
#6368 = VECTOR ( 'NONE', #6445, 1000.000000000000000 ) ;
#6369 = CARTESIAN_POINT ( 'NONE',  ( 138.6636751345948255, 0.000000000000000000, 5.500000000000005329 ) ) ;
#6370 = CARTESIAN_POINT ( 'NONE',  ( 150.0863248654052313, 0.000000000000000000, 5.500000000000005329 ) ) ;
#6371 = CARTESIAN_POINT ( 'NONE',  ( 0.000000000000000000, 5.999999999999977796, -75.28867513459481131 ) ) ;
#6372 = VERTEX_POINT ( 'NONE', #29778 ) ;
#6373 = CARTESIAN_POINT ( 'NONE',  ( 155.6250000000000284, 0.000000000000000000, -6.000000000000005329 ) ) ;
#6374 = CARTESIAN_POINT ( 'NONE',  ( 6.000000000000052403, -1.607695154586662678, -108.7306624327026157 ) ) ;
#6375 = CARTESIAN_POINT ( 'NONE',  ( 117.3752832217622029, 1.849990392679523588, 0.000000000000000000 ) ) ;
#6376 = FACE_OUTER_BOUND ( 'NONE', #6578, .T. ) ;
#6377 = ORIENTED_EDGE ( 'NONE', *, *, #25421, .F. ) ;
#6378 = ORIENTED_EDGE ( 'NONE', *, *, #25394, .T. ) ;
#6379 = ADVANCED_FACE ( 'NONE', ( #10929 ), #17579, .F. ) ;
#6380 = CARTESIAN_POINT ( 'NONE',  ( -3.175426480542816510, 5.499999999999865885, -98.87499999999998579 ) ) ;
#6381 = CARTESIAN_POINT ( 'NONE',  ( 6.000000000000000888, -1.859271017917181981E-14, -89.16367513459485394 ) ) ;
#6382 = CARTESIAN_POINT ( 'NONE',  ( 3.608439182435180470, 6.249999999999982236, -110.0580127018922099 ) ) ;
#6383 = ORIENTED_EDGE ( 'NONE', *, *, #25573, .T. ) ;
#6384 = CARTESIAN_POINT ( 'NONE',  ( -5.999999999999963585, 1.780251999655701777E-13, -93.83632486540518869 ) ) ;
#6385 = CIRCLE ( 'NONE', #10336, 14.99999999999998579 ) ;
#6386 = CARTESIAN_POINT ( 'NONE',  ( 0.7560853098879504186, -15.51667758746989989, 8.092232509380407279 ) ) ;
#6387 =( NAMED_UNIT ( * ) SI_UNIT ( $, .STERADIAN. ) SOLID_ANGLE_UNIT ( ) );
#6388 = ORIENTED_EDGE ( 'NONE', *, *, #18893, .T. ) ;
#6389 = CARTESIAN_POINT ( 'NONE',  ( 5.196152422706629359, 3.000000000000002665, -153.5386751345948539 ) ) ;
#6390 = DIRECTION ( 'NONE',  ( 0.000000000000000000, -1.000000000000000000, 0.000000000000000000 ) ) ;
#6391 = EDGE_CURVE ( 'NONE', #11657, #22729, #24983, .T. ) ;
#6392 = CARTESIAN_POINT ( 'NONE',  ( 5.196152422706629359, -2.999999999999988898, -61.71132486540520290 ) ) ;
#6393 = CARTESIAN_POINT ( 'NONE',  ( -4.763139720814407951, 2.749999999999946709, -166.2500000000000000 ) ) ;
#6394 = CARTESIAN_POINT ( 'NONE',  ( 114.8749999999998295, 1.767766952966320915, -1.767766952966209892 ) ) ;
#6395 = CARTESIAN_POINT ( 'NONE',  ( -5.196152422706573404, -3.000000000000002665, -158.2113248654052313 ) ) ;
#6396 = CARTESIAN_POINT ( 'NONE',  ( -3.175426480542816066, -5.500000000000057732, -107.3750000000000284 ) ) ;
#6397 = CARTESIAN_POINT ( 'NONE',  ( 160.1324251345948255, -5.500000000000012434, -2.278174593052012309 ) ) ;
#6398 = LINE ( 'NONE', #20548, #22621 ) ;
#6399 = CARTESIAN_POINT ( 'NONE',  ( -6.350852961085760029, -1.281975124255709124E-13, -95.62500000000004263 ) ) ;
#6400 = CARTESIAN_POINT ( 'NONE',  ( 0.000000000000000000, -5.999999999999991118, -112.0386751345948682 ) ) ;
#6401 = CARTESIAN_POINT ( 'NONE',  ( -5.196152422706601826, 2.999999999999975131, -162.0386751345948539 ) ) ;
#6402 = CARTESIAN_POINT ( 'NONE',  ( 6.000000000000000888, 1.743066579297358182E-13, -81.66367513459481131 ) ) ;
#6403 = VERTEX_POINT ( 'NONE', #19919 ) ;
#6404 = CARTESIAN_POINT ( 'NONE',  ( 118.6874999999998295, -1.035533905932719101, -2.499999999999844569 ) ) ;
#6405 = CARTESIAN_POINT ( 'NONE',  ( 108.6877832217621318, -0.7662911109077388261, 1.849990392679712103 ) ) ;
#6406 = CARTESIAN_POINT ( 'NONE',  ( 107.8988248654050750, 0.8284271247461753029, 2.000000000000212275 ) ) ;
#6407 = ORIENTED_EDGE ( 'NONE', *, *, #7034, .F. ) ;
#6408 = CARTESIAN_POINT ( 'NONE',  ( 109.8988248654049755, 0.8284271247462654530, 2.000000000000212275 ) ) ;
#6409 = CARTESIAN_POINT ( 'NONE',  ( 3.608439182435180470, -6.249999999999997335, -91.69198729810777593 ) ) ;
#6410 = CARTESIAN_POINT ( 'NONE',  ( 116.0000000000000142, 6.735557395310442023E-16, 5.500000000000000000 ) ) ;
#6411 = VERTEX_POINT ( 'NONE', #17952 ) ;
#6412 = CARTESIAN_POINT ( 'NONE',  ( -4.874391507318773797, 9.861790235658084214, -28.50395189876372370 ) ) ;
#6413 =( BOUNDED_CURVE ( )  B_SPLINE_CURVE ( 2, ( #10361, #14970, #10060, #24023, #16700, #19719, #26169, #28761, #819 ),
 .UNSPECIFIED., .F., .T. ) 
 B_SPLINE_CURVE_WITH_KNOTS ( ( 3, 2, 2, 2, 3 ),
 ( 0.5972222222222222099, 0.5981481481481480955, 0.5999999999999999778, 0.6018518518518518601, 0.6027777777777777457 ),
 .UNSPECIFIED. ) 
 CURVE ( )  GEOMETRIC_REPRESENTATION_ITEM ( )  RATIONAL_B_SPLINE_CURVE ( ( 0.9330127018922194093, 0.9330127018922194093, 1.000000000000000000, 0.8660254037844388186, 1.000000000000000000, 0.8660254037844388186, 1.000000000000000000, 0.9330127018922194093, 0.9330127018922194093 ) ) 
 REPRESENTATION_ITEM ( '' )  );
#6414 = VECTOR ( 'NONE', #20939, 1000.000000000000000 ) ;
#6415 = EDGE_LOOP ( 'NONE', ( #22650, #26990, #7636, #10846 ) ) ;
#6416 = ORIENTED_EDGE ( 'NONE', *, *, #23, .T. ) ;
#6417 = CARTESIAN_POINT ( 'NONE',  ( 158.5312500000000284, -2.485281374238555774, -6.000000000000005329 ) ) ;
#6418 = ADVANCED_FACE ( 'NONE', ( #8865 ), #26961, .T. ) ;
#6419 = CARTESIAN_POINT ( 'NONE',  ( -4.763139720814407951, 2.749999999999946709, -118.2500000000000284 ) ) ;
#6420 = CARTESIAN_POINT ( 'NONE',  ( 2.775557561562891351E-14, 6.250000000000033751, -138.4330127018922383 ) ) ;
#6421 = VERTEX_POINT ( 'NONE', #22227 ) ;
#6422 = CARTESIAN_POINT ( 'NONE',  ( -5.999999999999962697, 3.323446944526963891E-14, -160.4136751345948255 ) ) ;
#6423 = CARTESIAN_POINT ( 'NONE',  ( -3.608439182435052128, -6.250000000000110134, -126.4419872981078186 ) ) ;
#6424 = CARTESIAN_POINT ( 'NONE',  ( 5.412658773652739619, 3.124999999999988898, -176.8169872981077901 ) ) ;
#6425 = CARTESIAN_POINT ( 'NONE',  ( 159.1341896120059687, -12.00570085348640603, 3.993189331442730250 ) ) ;
#6426 = LINE ( 'NONE', #7452, #1996 ) ;
#6427 = CIRCLE ( 'NONE', #15281, 15.00000000000000000 ) ;
#6428 = ORIENTED_EDGE ( 'NONE', *, *, #7414, .F. ) ;
#6429 = CARTESIAN_POINT ( 'NONE',  ( 12.93750000000004086, 2.000000000000151879, -0.8284271247462955401 ) ) ;
#6430 = EDGE_CURVE ( 'NONE', #27870, #7693, #18098, .T. ) ;
#6431 = DIRECTION ( 'NONE',  ( 0.000000000000000000, 0.000000000000000000, 1.000000000000000000 ) ) ;
#6432 = ADVANCED_FACE ( 'NONE', ( #13048 ), #29264, .F. ) ;
#6433 = CARTESIAN_POINT ( 'NONE',  ( 15.53867513459491967, 1.110223024625156540E-13, 2.499999999999835687 ) ) ;
#6434 = DIRECTION ( 'NONE',  ( 1.000000000000000000, 0.000000000000000000, 0.000000000000000000 ) ) ;
#6435 = EDGE_CURVE ( 'NONE', #17334, #8787, #6236, .T. ) ;
#6436 = AXIS2_PLACEMENT_3D ( 'NONE', #26208, #122, #5161 ) ;
#6437 = CARTESIAN_POINT ( 'NONE',  ( 23.02382486540530948, -1.035533905932629173, 2.499999999999784173 ) ) ;
#6438 = CARTESIAN_POINT ( 'NONE',  ( 111.7502832217623165, -1.308140751793585022, 1.308140751793862577 ) ) ;
#6439 = CARTESIAN_POINT ( 'NONE',  ( 3.608439182435180470, -6.249999999999997335, -75.19198729810783277 ) ) ;
#6440 = VECTOR ( 'NONE', #19267, 1000.000000000000000 ) ;
#6441 = CARTESIAN_POINT ( 'NONE',  ( 7.216878364870455975, -6.409875621278545621E-14, -61.44198729810783277 ) ) ;
#6442 = CARTESIAN_POINT ( 'NONE',  ( -5.999999999999963585, 8.134310703387671600E-14, -121.4136751345948255 ) ) ;
#6443 = CARTESIAN_POINT ( 'NONE',  ( 4.763139720814407951, -2.749999999999988454, -53.00000000000004974 ) ) ;
#6444 = DIRECTION ( 'NONE',  ( -0.000000000000000000, -1.000000000000000000, -0.000000000000000000 ) ) ;
#6445 = DIRECTION ( 'NONE',  ( -1.000000000000000000, -1.665334536937731113E-16, 1.526556658859586792E-16 ) ) ;
#6446 = CARTESIAN_POINT ( 'NONE',  ( -2.775557561562891351E-14, -5.500000000000115463, -119.2500000000000284 ) ) ;
#6448 = VECTOR ( 'NONE', #30258, 1000.000000000000000 ) ;
#6447 = CARTESIAN_POINT ( 'NONE',  ( -5.999999999999971578, 1.607695154586715303, -137.9806624327025872 ) ) ;
#6449 = ORIENTED_EDGE ( 'NONE', *, *, #6535, .T. ) ;
#6450 = CARTESIAN_POINT ( 'NONE',  ( 6.000000000000000888, -1.607695154586752384, -118.6533121635130357 ) ) ;
#6451 = CARTESIAN_POINT ( 'NONE',  ( 124.9999999999999432, -65.50000000000000000, -7.500000000000007105 ) ) ;
#6452 = FACE_OUTER_BOUND ( 'NONE', #4240, .T. ) ;
#6453 = CARTESIAN_POINT ( 'NONE',  ( 140.6398502691896510, -3.535533905932752852, 3.535533905932725318 ) ) ;
#6454 = CARTESIAN_POINT ( 'NONE',  ( -4.999999999999984013, -65.50000000000001421, 7.500000000000007105 ) ) ;
#6455 = ORIENTED_EDGE ( 'NONE', *, *, #14788, .T. ) ;
#6456 = CARTESIAN_POINT ( 'NONE',  ( 108.0622167782374703, -1.849990392679381701, 0.7662911109080090544 ) ) ;
#6457 = CARTESIAN_POINT ( 'NONE',  ( 10.66367513459495697, -1.767766952966265404, 1.767766952966376426 ) ) ;
#6458 = CARTESIAN_POINT ( 'NONE',  ( 114.1011751345946834, 0.8284271247462654530, -1.999999999999731104 ) ) ;
#6459 = CARTESIAN_POINT ( 'NONE',  ( 113.1247167782375556, -1.849990392679523588, 1.110223024625156540E-13 ) ) ;
#6460 = CARTESIAN_POINT ( 'NONE',  ( 3.608439182435180470, -6.249999999999997335, -115.6919872981078328 ) ) ;
#6461 = CARTESIAN_POINT ( 'NONE',  ( 135.0000000000000000, 1.949781249179272091, -5.142796231657337458 ) ) ;
#6462 = CARTESIAN_POINT ( 'NONE',  ( 10.00000000000016520, 0.07538101147688137937, 2.429594365314368787 ) ) ;
#6463 = ORIENTED_EDGE ( 'NONE', *, *, #5351, .T. ) ;
#6464 = VERTEX_POINT ( 'NONE', #13500 ) ;
#6465 = CARTESIAN_POINT ( 'NONE',  ( 138.2886751345948539, 5.500000000000005329, 0.000000000000000000 ) ) ;
#6466 = CARTESIAN_POINT ( 'NONE',  ( 143.7187500000000284, 2.485281374238555774, -6.000000000000005329 ) ) ;
#6467 = ADVANCED_FACE ( 'NONE', ( #10730 ), #24509, .T. ) ;
#6468 = EDGE_LOOP ( 'NONE', ( #5204, #13832, #12773, #3691 ) ) ;
#6469 = CARTESIAN_POINT ( 'NONE',  ( -7.216878364870328078, 0.000000000000000000, -144.6919872981078470 ) ) ;
#6470 = ORIENTED_EDGE ( 'NONE', *, *, #16069, .F. ) ;
#6472 = CARTESIAN_POINT ( 'NONE',  ( -1.000000000000000888, 9.000000000000007105, 3.000000000000002665 ) ) ;
#6471 = AXIS2_PLACEMENT_3D ( 'NONE', #1136, #18077, #8364 ) ;
#6473 = SURFACE_SIDE_STYLE ('',( #13739 ) ) ;
#6474 = PRODUCT ( 'Handle', 'Handle', '', ( #10857 ) ) ;
#6475 = CARTESIAN_POINT ( 'NONE',  ( 24.50000000000015987, -1.999999999999835243, -5.551115123125782702E-14 ) ) ;
#6476 = DIRECTION ( 'NONE',  ( -8.326672684688675286E-17, -2.081668171172168821E-17, 1.000000000000000000 ) ) ;
#6477 = EDGE_CURVE ( 'NONE', #3318, #9839, #10884, .T. ) ;
#6478 = CARTESIAN_POINT ( 'NONE',  ( 105.2113248654051745, -1.999999999999974021, 0.000000000000000000 ) ) ;
#6479 = CARTESIAN_POINT ( 'NONE',  ( 2.775557561562891351E-14, -6.250000000000061284, -65.68301270189225249 ) ) ;
#6480 = EDGE_CURVE ( 'NONE', #15355, #17525, #1781, .T. ) ;
#6481 = CARTESIAN_POINT ( 'NONE',  ( 151.4851497308104342, -3.535533905932725318, 3.535533905932725318 ) ) ;
#6482 = CARTESIAN_POINT ( 'NONE',  ( 0.000000000000000000, 0.000000000000000000, 0.000000000000000000 ) ) ;
#6483 = CARTESIAN_POINT ( 'NONE',  ( -21.99999999999998934, -10.99999999999992362, -14.99152654425661879 ) ) ;
#6484 = CARTESIAN_POINT ( 'NONE',  ( 6.000000000000000888, 5.577813053751546416E-15, -165.6636751345948255 ) ) ;
#6485 = FACE_OUTER_BOUND ( 'NONE', #28227, .T. ) ;
#6486 = CARTESIAN_POINT ( 'NONE',  ( 5.196152422706629359, -2.999999999999988898, -66.78867513459485394 ) ) ;
#6487 = CARTESIAN_POINT ( 'NONE',  ( 3.175426480543072749, 5.499999999999865885, -121.6250000000000426 ) ) ;
#6488 = CARTESIAN_POINT ( 'NONE',  ( 3.608439182435180470, 6.249999999999982236, -146.0580127018922667 ) ) ;
#6489 = DIRECTION ( 'NONE',  ( 0.000000000000000000, 8.346795477010025210E-14, 1.000000000000000000 ) ) ;
#6490 = ORIENTED_EDGE ( 'NONE', *, *, #8809, .T. ) ;
#6491 = CARTESIAN_POINT ( 'NONE',  ( 3.175426480543072749, 5.499999999999865885, -55.62500000000004263 ) ) ;
#6492 = CARTESIAN_POINT ( 'NONE',  ( -5.196152422706573404, -3.000000000000002665, -154.2886751345948255 ) ) ;
#6493 = CARTESIAN_POINT ( 'NONE',  ( -6.000000000000007105, -1.607695154586655129, -77.26933756729744118 ) ) ;
#6494 = DIRECTION ( 'NONE',  ( 0.000000000000000000, 1.000000000000000000, 0.000000000000000000 ) ) ;
#6495 = ORIENTED_EDGE ( 'NONE', *, *, #7345, .T. ) ;
#6496 = CARTESIAN_POINT ( 'NONE',  ( 104.6874999999998579, -1.035533905932689347, -2.499999999999724221 ) ) ;
#6497 = CARTESIAN_POINT ( 'NONE',  ( 146.5312500000000284, -2.485281374238556218, -6.000000000000005329 ) ) ;
#6498 = CARTESIAN_POINT ( 'NONE',  ( 160.0296263098200313, -11.64871681939485093, -2.884697388352327252 ) ) ;
#6499 = SURFACE_STYLE_FILL_AREA ( #10680 ) ;
#6500 = CARTESIAN_POINT ( 'NONE',  ( 137.9062500000000568, 6.000000000000005329, -2.485281374238555774 ) ) ;
#6501 = CARTESIAN_POINT ( 'NONE',  ( -14.99999999999999289, -54.99999999999990763, 8.000000000000007105 ) ) ;
#6502 = ORIENTED_EDGE ( 'NONE', *, *, #17253, .T. ) ;
#6503 = ADVANCED_FACE ( 'NONE', ( #22380 ), #8708, .F. ) ;
#6504 = CARTESIAN_POINT ( 'NONE',  ( 0.000000000000000000, 5.499999999999991118, -139.5000000000000000 ) ) ;
#6505 = CARTESIAN_POINT ( 'NONE',  ( 12.37500000000013500, -1.414213562372979016, 1.414213562373034527 ) ) ;
#6506 = ORIENTED_EDGE ( 'NONE', *, *, #18026, .F. ) ;
#6507 = CARTESIAN_POINT ( 'NONE',  ( 0.000000000000000000, 5.499999999999991118, -73.50000000000001421 ) ) ;
#6508 = CARTESIAN_POINT ( 'NONE',  ( -0.07769256095283699759, -15.23231281889969679, -7.500000000000007105 ) ) ;
#6509 = EDGE_CURVE ( 'NONE', #17900, #9152, #11309, .T. ) ;
#6510 =( BOUNDED_CURVE ( )  B_SPLINE_CURVE ( 2, ( #13870, #16021, #11242, #28081, #30247, #7056, #16174, #6901, #25319 ),
 .UNSPECIFIED., .F., .T. ) 
 B_SPLINE_CURVE_WITH_KNOTS ( ( 3, 2, 2, 2, 3 ),
 ( 0.4805555555555555136, 0.4814814814814815103, 0.4833333333333332815, 0.4851851851851851638, 0.4861111111111111605 ),
 .UNSPECIFIED. ) 
 CURVE ( )  GEOMETRIC_REPRESENTATION_ITEM ( )  RATIONAL_B_SPLINE_CURVE ( ( 0.9330127018922194093, 0.9330127018922154125, 1.000000000000000000, 0.8660254037844388186, 1.000000000000000000, 0.8660254037844388186, 1.000000000000000000, 0.9330127018922154125, 0.9330127018922194093 ) ) 
 REPRESENTATION_ITEM ( '' )  );
#6511 = CARTESIAN_POINT ( 'NONE',  ( -5.960408494996731754, -9.245657484109301549, -25.79492440527506858 ) ) ;
#6512 = CARTESIAN_POINT ( 'NONE',  ( 3.464101615137852974, 5.999999999999884537, -150.4136751345947971 ) ) ;
#6513 = FACE_OUTER_BOUND ( 'NONE', #28888, .T. ) ;
#6514 = CARTESIAN_POINT ( 'NONE',  ( 10.00000000000014566, 5.637083940101657433E-14, -6.000000000000056843 ) ) ;
#6515 =( BOUNDED_CURVE ( )  B_SPLINE_CURVE ( 2, ( #1933, #11807, #4540, #21144, #13965, #15808, #11340, #11655, #6694 ),
 .UNSPECIFIED., .F., .F. ) 
 B_SPLINE_CURVE_WITH_KNOTS ( ( 3, 2, 2, 2, 3 ),
 ( 0.9861111111111111605, 0.9870370370370370461, 0.9888888888888889284, 0.9907407407407406996, 0.9910511276943060333 ),
 .UNSPECIFIED. ) 
 CURVE ( )  GEOMETRIC_REPRESENTATION_ITEM ( )  RATIONAL_B_SPLINE_CURVE ( ( 0.9330127018922194093, 0.9330127018922234061, 1.000000000000000000, 0.8660254037844388186, 1.000000000000000000, 0.8660254037844388186, 1.000000000000000000, 0.9775446579417738091, 0.9626167487132855083 ) ) 
 REPRESENTATION_ITEM ( '' )  );
#6516 = CARTESIAN_POINT ( 'NONE',  ( -3.175426480542816066, 5.499999999999865885, -151.3749999999999716 ) ) ;
#6517 = CARTESIAN_POINT ( 'NONE',  ( 139.5000000000000000, -8.798545334315230448, 8.160000000000007248 ) ) ;
#6518 = DIRECTION ( 'NONE',  ( 3.330669073875465184E-16, -1.000000000000000000, -7.523163845262629360E-36 ) ) ;
#6519 = CARTESIAN_POINT ( 'NONE',  ( -3.175426480542816066, -5.500000000000057732, -84.87500000000004263 ) ) ;
#6520 = CARTESIAN_POINT ( 'NONE',  ( 148.4136751345948539, 0.000000000000000000, -5.500000000000005329 ) ) ;
#6521 = CARTESIAN_POINT ( 'NONE',  ( -6.350852961085760029, -1.281975124255709124E-13, -76.12500000000000000 ) ) ;
#6522 = PRESENTATION_LAYER_ASSIGNMENT (  '', '', ( #26143 ) ) ;
#6523 = CARTESIAN_POINT ( 'NONE',  ( 150.1086002691896510, -2.071067811865468400, -4.999999999999989342 ) ) ;
#6524 = CARTESIAN_POINT ( 'NONE',  ( 116.0000000000000142, 0.000000000000000000, -5.500000000000000000 ) ) ;
#6525 = CARTESIAN_POINT ( 'NONE',  ( 5.196152422706629359, -2.999999999999988898, -71.28867513459479710 ) ) ;
#6526 = CYLINDRICAL_SURFACE ( 'NONE', #25572, 2.000000000000012879 ) ;
#6527 = CARTESIAN_POINT ( 'NONE',  ( 19.37500000000019895, -1.414213562372979016, 1.414213562373034527 ) ) ;
#6528 = CYLINDRICAL_SURFACE ( 'NONE', #15904, 5.500000000000000000 ) ;
#6529 = DIRECTION ( 'NONE',  ( -1.000000000000000000, -1.665334536937731113E-16, 1.526556658859586792E-16 ) ) ;
#6530 = DIRECTION ( 'NONE',  ( -1.000000000000000000, -0.000000000000000000, -0.000000000000000000 ) ) ;
#6531 = PRODUCT_DEFINITION_FORMATION_WITH_SPECIFIED_SOURCE ( 'ANY', '', #6217, .NOT_KNOWN. ) ;
#6532 = ORIENTED_EDGE ( 'NONE', *, *, #16682, .F. ) ;
#6533 = CARTESIAN_POINT ( 'NONE',  ( 157.6875000000000284, 4.242640687119269671, 4.242640687119298093 ) ) ;
#6534 = CARTESIAN_POINT ( 'NONE',  ( 14.71132486540532902, 2.500000000000057732, -1.665334536937734811E-13 ) ) ;
#6535 = EDGE_CURVE ( 'NONE', #8715, #7154, #12303, .T. ) ;
#6536 = CARTESIAN_POINT ( 'NONE',  ( 0.000000000000000000, 0.000000000000000000, 0.000000000000000000 ) ) ;
#6537 = ORIENTED_EDGE ( 'NONE', *, *, #12008, .T. ) ;
#6538 = EDGE_LOOP ( 'NONE', ( #29998, #2210, #9833, #22490 ) ) ;
#6539 = ADVANCED_FACE ( 'NONE', ( #7554, #7273 ), #12362, .F. ) ;
#6540 = ORIENTED_EDGE ( 'NONE', *, *, #12614, .T. ) ;
#6541 = CARTESIAN_POINT ( 'NONE',  ( -6.350852961085760029, -1.281975124255709124E-13, -95.62500000000004263 ) ) ;
#6542 = CARTESIAN_POINT ( 'NONE',  ( -5.999999999999963585, 1.780251999655701777E-13, -89.91367513459485394 ) ) ;
#6543 = CARTESIAN_POINT ( 'NONE',  ( -3.608439182435115633, 6.249999999999965361, -109.8080127018922667 ) ) ;
#6544 = ORIENTED_EDGE ( 'NONE', *, *, #3538, .T. ) ;
#6545 = FILL_AREA_STYLE ('',( #29591 ) ) ;
#6546 = STYLED_ITEM ( 'NONE', ( #19783 ), #10017 ) ;
#6547 = CARTESIAN_POINT ( 'NONE',  ( -5.196152422706573404, -3.000000000000002665, -143.7886751345948255 ) ) ;
#6548 = CARTESIAN_POINT ( 'NONE',  ( -4.763139720814407951, -2.750000000000016431, -164.5000000000000284 ) ) ;
#6549 = CARTESIAN_POINT ( 'NONE',  ( 5.412658773652739619, 3.124999999999988898, -47.18301270189223828 ) ) ;
#6550 = ORIENTED_EDGE ( 'NONE', *, *, #21919, .F. ) ;
#6551 = CARTESIAN_POINT ( 'NONE',  ( 5.999999999999999112, 2.951592740943527306E-14, -160.5863248654052029 ) ) ;
#6552 = CARTESIAN_POINT ( 'NONE',  ( 0.000000000000000000, 0.000000000000000000, 0.000000000000000000 ) ) ;
#6553 = CARTESIAN_POINT ( 'NONE',  ( 140.4121221836153950, -9.236957375441377849, 7.663966194509516328 ) ) ;
#6554 = CARTESIAN_POINT ( 'NONE',  ( -6.350852961085760029, -1.281975124255709124E-13, -160.1250000000000284 ) ) ;
#6555 =( BOUNDED_CURVE ( )  B_SPLINE_CURVE ( 2, ( #21386, #2771, #1327, #5624, #28973, #10741, #7395, #465, #21539 ),
 .UNSPECIFIED., .F., .F. ) 
 B_SPLINE_CURVE_WITH_KNOTS ( ( 3, 2, 2, 2, 3 ),
 ( 0.7968750000000000000, 0.8046875000000000000, 0.8125000000000000000, 0.8203125000000000000, 0.8281250000000000000 ),
 .UNSPECIFIED. ) 
 CURVE ( )  GEOMETRIC_REPRESENTATION_ITEM ( )  RATIONAL_B_SPLINE_CURVE ( ( 1.000000000000000000, 0.9238795325112867385, 1.000000000000000000, 0.9238795325112867385, 1.000000000000000000, 0.9238795325112867385, 1.000000000000000000, 0.9238795325112867385, 1.000000000000000000 ) ) 
 REPRESENTATION_ITEM ( '' )  );
#6556 = CARTESIAN_POINT ( 'NONE',  ( 114.3749999999998010, -1.767766952966154381, 1.767766952966653982 ) ) ;
#6557 =( BOUNDED_CURVE ( )  B_SPLINE_CURVE ( 2, ( #9405, #18794, #25978, #11439, #23395, #2033, #11592, #28118, #4920 ),
 .UNSPECIFIED., .F., .F. ) 
 B_SPLINE_CURVE_WITH_KNOTS ( ( 3, 2, 2, 2, 3 ),
 ( 0.8472222222222222099, 0.8481481481481480955, 0.8499999999999999778, 0.8518518518518518601, 0.8527777777777778567 ),
 .UNSPECIFIED. ) 
 CURVE ( )  GEOMETRIC_REPRESENTATION_ITEM ( )  RATIONAL_B_SPLINE_CURVE ( ( 0.9330127018922194093, 0.9330127018922194093, 1.000000000000000000, 0.8660254037844388186, 1.000000000000000000, 0.8660254037844388186, 1.000000000000000000, 0.9330127018922154125, 0.9330127018922194093 ) ) 
 REPRESENTATION_ITEM ( '' )  );
#6558 = CARTESIAN_POINT ( 'NONE',  ( -6.350852961085760029, -1.281975124255709124E-13, -112.1249999999999858 ) ) ;
#6559 = LINE ( 'NONE', #7018, #26043 ) ;
#6560 = CARTESIAN_POINT ( 'NONE',  ( -2.775557561562891351E-14, -5.500000000000115463, -96.75000000000000000 ) ) ;
#6561 = CARTESIAN_POINT ( 'NONE',  ( 0.2138740463844765738, -15.56974731274248391, 7.989747270033618953 ) ) ;
#6562 = EDGE_LOOP ( 'NONE', ( #4466, #20532, #25146, #24103 ) ) ;
#6563 = CARTESIAN_POINT ( 'NONE',  ( 10.56250000000007461, 2.649519052838358757, -1.097466725451559322 ) ) ;
#6564 = CARTESIAN_POINT ( 'NONE',  ( 115.1249999999998863, 1.767766952966376426, 1.767766952966320915 ) ) ;
#6565 = FACE_OUTER_BOUND ( 'NONE', #17340, .T. ) ;
#6566 = CARTESIAN_POINT ( 'NONE',  ( 109.5627832217622455, 0.7662911109077987781, 1.849990392679652151 ) ) ;
#6567 = FACE_OUTER_BOUND ( 'NONE', #10284, .T. ) ;
#6568 = VERTEX_POINT ( 'NONE', #21561 ) ;
#6569 = SURFACE_STYLE_FILL_AREA ( #29612 ) ;
#6570 = CARTESIAN_POINT ( 'NONE',  ( 108.0622167782374703, -1.849990392679381701, 0.7662911109080090544 ) ) ;
#6571 = CARTESIAN_POINT ( 'NONE',  ( 5.412658773652739619, 3.124999999999988898, -91.31698729810783277 ) ) ;
#6572 = ORIENTED_EDGE ( 'NONE', *, *, #9803, .T. ) ;
#6573 = CARTESIAN_POINT ( 'NONE',  ( -3.679869817085036576, 10.37177793260014802, -29.75506555745397108 ) ) ;
#6574 = EDGE_CURVE ( 'NONE', #11262, #30108, #19709, .T. ) ;
#6575 = ORIENTED_EDGE ( 'NONE', *, *, #11716, .F. ) ;
#6576 = EDGE_LOOP ( 'NONE', ( #9913, #6506 ) ) ;
#6577 = CARTESIAN_POINT ( 'NONE',  ( 150.8437500000000284, -6.000000000000005329, -2.485281374238555774 ) ) ;
#6578 = EDGE_LOOP ( 'NONE', ( #9774, #18859, #6998, #723 ) ) ;
#6579 = CARTESIAN_POINT ( 'NONE',  ( 3.175426480543072749, 5.499999999999865885, -124.6250000000000426 ) ) ;
#6580 = CARTESIAN_POINT ( 'NONE',  ( 22.50000000000013145, 1.873492889145123019, 1.873492889144845464 ) ) ;
#6581 = CARTESIAN_POINT ( 'NONE',  ( -5.412658773652684552, -3.125000000000099920, -133.4330127018922383 ) ) ;
#6582 = ORIENTED_EDGE ( 'NONE', *, *, #29523, .F. ) ;
#6583 = DIRECTION ( 'NONE',  ( -1.000000000000000000, -1.734723475976843579E-16, 0.000000000000000000 ) ) ;
#6584 = CARTESIAN_POINT ( 'NONE',  ( -7.216878364870328078, 0.000000000000000000, -125.1919872981078186 ) ) ;
#6585 = CARTESIAN_POINT ( 'NONE',  ( -5.412658773652739619, 3.124999999999975131, -179.3169872981078470 ) ) ;
#6586 = CARTESIAN_POINT ( 'NONE',  ( 159.5122198478899804, -12.10635047839714673, 3.869002046573032150 ) ) ;
#6587 = DIRECTION ( 'NONE',  ( 0.000000000000000000, 1.000000000000000000, 8.881784197001252323E-16 ) ) ;
#6588 = ORIENTED_EDGE ( 'NONE', *, *, #6391, .F. ) ;
#6589 = CARTESIAN_POINT ( 'NONE',  ( -5.196152422706601826, 2.999999999999975131, -163.5386751345947971 ) ) ;
#6590 = CARTESIAN_POINT ( 'NONE',  ( 3.606777763902872191, 4.527305315990890477, -180.0000000000001990 ) ) ;
#6591 = FACE_OUTER_BOUND ( 'NONE', #21523, .T. ) ;
#6592 = CARTESIAN_POINT ( 'NONE',  ( 112.5238248654049755, 0.8284271247463257382, -1.999999999999731104 ) ) ;
#6593 = CARTESIAN_POINT ( 'NONE',  ( 112.4377832217622455, 1.849990392679621953, 0.7662911109081291805 ) ) ;
#6594 = CARTESIAN_POINT ( 'NONE',  ( 7.216878364870455975, -6.409875621278545621E-14, -71.94198729810780435 ) ) ;
#6595 = CARTESIAN_POINT ( 'NONE',  ( 3.608439182435180470, 6.249999999999982236, -58.19198729810781856 ) ) ;
#6596 = CARTESIAN_POINT ( 'NONE',  ( -2.000000000000003109, 3.559516622919867392E-16, 2.520259888162984417E-35 ) ) ;
#6597 = CARTESIAN_POINT ( 'NONE',  ( -5.412658773652739619, 3.124999999999975131, -181.6830127018922383 ) ) ;
#6598 = DIRECTION ( 'NONE',  ( -1.000000000000000000, -1.665334536937736783E-16, -2.220446049250315546E-16 ) ) ;
#6599 = CYLINDRICAL_SURFACE ( 'NONE', #7837, 6.000000000000001776 ) ;
#6600 = STYLED_ITEM ( 'NONE', ( #335 ), #2752 ) ;
#6601 = CARTESIAN_POINT ( 'NONE',  ( 6.000000000000000888, 1.743066579297358182E-13, -69.08632486540523132 ) ) ;
#6602 = CARTESIAN_POINT ( 'NONE',  ( 0.000000000000000000, 5.499999999999991118, -123.0000000000000000 ) ) ;
#6603 = CARTESIAN_POINT ( 'NONE',  ( 0.000000000000000000, 5.499999999999991118, -157.5000000000000284 ) ) ;
#6604 = CARTESIAN_POINT ( 'NONE',  ( -3.464101615137725076, 5.999999999999979572, -50.58632486540523132 ) ) ;
#6605 = CARTESIAN_POINT ( 'NONE',  ( -5.999999999999963585, -1.487416814333745711E-14, -153.8363248654052313 ) ) ;
#6606 = ORIENTED_EDGE ( 'NONE', *, *, #23319, .F. ) ;
#6607 = CARTESIAN_POINT ( 'NONE',  ( 19.56250000000015632, 2.649519052838419153, -1.097466725451499370 ) ) ;
#6608 = EDGE_CURVE ( 'NONE', #12110, #21920, #654, .T. ) ;
#6609 = DIRECTION ( 'NONE',  ( 0.000000000000000000, -1.000000000000000000, 0.000000000000000000 ) ) ;
#6610 = CARTESIAN_POINT ( 'NONE',  ( 140.5461002691896510, -2.071067811865468400, 4.999999999999989342 ) ) ;
#6611 =( BOUNDED_CURVE ( )  B_SPLINE_CURVE ( 2, ( #5708, #25321, #10666, #24301, #20011, #3404, #17734, #27059, #6024 ),
 .UNSPECIFIED., .F., .T. ) 
 B_SPLINE_CURVE_WITH_KNOTS ( ( 3, 2, 2, 2, 3 ),
 ( 0.02941176470588236294, 0.03676470588235292158, 0.04411764705882348370, 0.05147058823529415683, 0.05882352941176471894 ),
 .UNSPECIFIED. ) 
 CURVE ( )  GEOMETRIC_REPRESENTATION_ITEM ( )  RATIONAL_B_SPLINE_CURVE ( ( 1.000000000000000000, 0.9238795325112867385, 1.000000000000000000, 0.9238795325112867385, 1.000000000000000000, 0.9238795325112867385, 1.000000000000000000, 0.9238795325112867385, 1.000000000000000000 ) ) 
 REPRESENTATION_ITEM ( '' )  );
#6612 = ORIENTED_EDGE ( 'NONE', *, *, #18715, .F. ) ;
#6613 = CARTESIAN_POINT ( 'NONE',  ( 110.3747167782375271, -5.551115123125782702E-14, -1.849990392679523588 ) ) ;
#6614 = CARTESIAN_POINT ( 'NONE',  ( -5.999999999999963585, 8.134310703387671600E-14, -129.8363248654052313 ) ) ;
#6615 = CARTESIAN_POINT ( 'NONE',  ( 113.1872167782373992, -1.849990392679441875, -0.7662911109075883909 ) ) ;
#6616 = CARTESIAN_POINT ( 'NONE',  ( 2.775557561562891351E-14, -6.250000000000061284, -115.8169872981078470 ) ) ;
#6617 = CARTESIAN_POINT ( 'NONE',  ( -5.999999999999959144, -1.607695154586739283, -176.8466878364870922 ) ) ;
#6618 = EDGE_CURVE ( 'NONE', #11567, #13346, #14657, .T. ) ;
#6619 = CARTESIAN_POINT ( 'NONE',  ( 113.5863248654051318, 1.414213562373145550, -1.414213562373145550 ) ) ;
#6620 = ORIENTED_EDGE ( 'NONE', *, *, #14087, .F. ) ;
#6621 = CARTESIAN_POINT ( 'NONE',  ( 0.000000000000000000, 0.000000000000000000, 0.000000000000000000 ) ) ;
#6622 = CARTESIAN_POINT ( 'NONE',  ( 143.4375000000000284, -4.242640687119298093, -4.242640687119298093 ) ) ;
#6623 = ORIENTED_EDGE ( 'NONE', *, *, #26599, .T. ) ;
#6624 = STYLED_ITEM ( 'NONE', ( #18725 ), #7544 ) ;
#6625 = CARTESIAN_POINT ( 'NONE',  ( 7.216878364870455975, -6.409875621278545621E-14, -148.4419872981078470 ) ) ;
#6626 = VERTEX_POINT ( 'NONE', #18817 ) ;
#6627 = DIRECTION ( 'NONE',  ( 0.000000000000000000, 5.551115123125767911E-17, -1.000000000000000000 ) ) ;
#6628 = CARTESIAN_POINT ( 'NONE',  ( 24.81250000000011724, 0.8284271247463557142, -2.000000000000091926 ) ) ;
#6629 = CYLINDRICAL_SURFACE ( 'NONE', #8825, 14.99999999999998579 ) ;
#6630 = DIRECTION ( 'NONE',  ( 1.000000000000000000, -5.551115123125773458E-17, -1.260129944081490338E-35 ) ) ;
#6631 = CARTESIAN_POINT ( 'NONE',  ( 2.775557561562891351E-14, -6.250000000000061284, -68.68301270189225249 ) ) ;
#6632 = CARTESIAN_POINT ( 'NONE',  ( 143.4226497308104342, 5.000000000000004441, 0.000000000000000000 ) ) ;
#6633 = CIRCLE ( 'NONE', #8074, 17.50000000000004619 ) ;
#6634 = DIRECTION ( 'NONE',  ( 1.000000000000000000, 0.000000000000000000, 0.000000000000000000 ) ) ;
#6635 = DIRECTION ( 'NONE',  ( -7.147005652999508048E-36, 5.642372883946980038E-36, 1.000000000000000000 ) ) ;
#6636 = DIRECTION ( 'NONE',  ( -1.000000000000000000, -1.665334536937731113E-16, 1.526556658859586792E-16 ) ) ;
#6637 = AXIS2_PLACEMENT_3D ( 'NONE', #6223, #15641, #22367 ) ;
#6638 = PLANE ( 'NONE',  #11143 ) ;
#6639 = CARTESIAN_POINT ( 'NONE',  ( -5.196152422706601826, 2.999999999999975131, -114.9613248654052171 ) ) ;
#6640 = CARTESIAN_POINT ( 'NONE',  ( 112.0624999999997868, 2.500000000000054623, 1.035533905932989551 ) ) ;
#6641 = LINE ( 'NONE', #11119, #3953 ) ;
#6642 = CARTESIAN_POINT ( 'NONE',  ( 4.763139720814407951, -2.749999999999988454, -125.0000000000000000 ) ) ;
#6643 = FACE_OUTER_BOUND ( 'NONE', #9263, .T. ) ;
#6644 = CARTESIAN_POINT ( 'NONE',  ( -7.216878364870328078, 0.000000000000000000, -144.0580127018922383 ) ) ;
#6645 = DIRECTION ( 'NONE',  ( 0.000000000000000000, 0.000000000000000000, -1.000000000000000000 ) ) ;
#6646 = ORIENTED_EDGE ( 'NONE', *, *, #6252, .F. ) ;
#6647 = EDGE_CURVE ( 'NONE', #2399, #16363, #12481, .T. ) ;
#6648 = CARTESIAN_POINT ( 'NONE',  ( -4.763139720814407951, -2.750000000000016431, -52.00000000000004263 ) ) ;
#6649 = DIRECTION ( 'NONE',  ( -7.147005652999508048E-36, 5.642372883946980038E-36, 1.000000000000000000 ) ) ;
#6650 = DIRECTION ( 'NONE',  ( -7.147005652999508048E-36, 5.642372883946980038E-36, 1.000000000000000000 ) ) ;
#6651 = DIRECTION ( 'NONE',  ( -1.000000000000000000, -1.067522139062651904E-16, 0.000000000000000000 ) ) ;
#6652 = ORIENTED_EDGE ( 'NONE', *, *, #3065, .F. ) ;
#6653 = AXIS2_PLACEMENT_3D ( 'NONE', #9838, #10446, #896 ) ;
#6654 = CARTESIAN_POINT ( 'NONE',  ( 105.9999999999998863, 2.500000000000002220, 1.110223024625156540E-13 ) ) ;
#6655 = CARTESIAN_POINT ( 'NONE',  ( 140.9062500000000284, 6.000000000000005329, -2.485281374238556218 ) ) ;
#6656 = CARTESIAN_POINT ( 'NONE',  ( 13.18750000000006750, 0.8284271247462955401, 2.000000000000031530 ) ) ;
#6657 = FACE_OUTER_BOUND ( 'NONE', #21146, .T. ) ;
#6658 = EDGE_CURVE ( 'NONE', #750, #14484, #15440, .T. ) ;
#6659 = EDGE_CURVE ( 'NONE', #13568, #11692, #23601, .T. ) ;
#6660 = CARTESIAN_POINT ( 'NONE',  ( 141.0000000000000284, 6.000000000000005329, 0.000000000000000000 ) ) ;
#6661 = DIRECTION ( 'NONE',  ( 0.000000000000000000, 0.000000000000000000, 1.000000000000000000 ) ) ;
#6662 =( BOUNDED_CURVE ( )  B_SPLINE_CURVE ( 2, ( #771, #21380, #7388, #2913, #316, #5361, #14769, #9705, #21970 ),
 .UNSPECIFIED., .F., .F. ) 
 B_SPLINE_CURVE_WITH_KNOTS ( ( 3, 2, 2, 2, 3 ),
 ( 0.4805555555555555136, 0.4814814814814814548, 0.4833333333333333370, 0.4851851851851851638, 0.4861111111111111049 ),
 .UNSPECIFIED. ) 
 CURVE ( )  GEOMETRIC_REPRESENTATION_ITEM ( )  RATIONAL_B_SPLINE_CURVE ( ( 0.9330127018922194093, 0.9330127018922174109, 1.000000000000000000, 0.8660254037844388186, 1.000000000000000000, 0.8660254037844388186, 1.000000000000000000, 0.9330127018922194093, 0.9330127018922194093 ) ) 
 REPRESENTATION_ITEM ( '' )  );
#6663 = CARTESIAN_POINT ( 'NONE',  ( -4.763139720814407951, -2.750000000000016431, -140.5000000000000000 ) ) ;
#6664 = CARTESIAN_POINT ( 'NONE',  ( 13.81249999999996980, 0.8284271247461753029, -2.000000000000091926 ) ) ;
#6665 = EDGE_LOOP ( 'NONE', ( #28506, #29885 ) ) ;
#6666 = CARTESIAN_POINT ( 'NONE',  ( -3.175426480542816510, -5.500000000000057732, -65.37500000000001421 ) ) ;
#6667 = CARTESIAN_POINT ( 'NONE',  ( 18.77382486540524908, 2.500000000000144773, 1.035533905932689347 ) ) ;
#6668 = ORIENTED_EDGE ( 'NONE', *, *, #6755, .F. ) ;
#6669 = CARTESIAN_POINT ( 'NONE',  ( 0.000000000000000000, 5.999999999999977796, -139.7886751345947971 ) ) ;
#6670 = DIRECTION ( 'NONE',  ( -7.147005652999508048E-36, 5.642372883946980038E-36, 1.000000000000000000 ) ) ;
#6671 = CARTESIAN_POINT ( 'NONE',  ( 0.000000000000000000, 0.000000000000000000, 0.000000000000000000 ) ) ;
#6672 = CARTESIAN_POINT ( 'NONE',  ( -4.763139720814407951, 2.749999999999946709, -151.2500000000000000 ) ) ;
#6673 = CARTESIAN_POINT ( 'NONE',  ( -0.5000000000000004441, -10.00000000000000888, -7.500000000000007105 ) ) ;
#6674 = CARTESIAN_POINT ( 'NONE',  ( 5.412658773652712085, -3.125000000000086153, -159.9330127018922383 ) ) ;
#6675 = CARTESIAN_POINT ( 'NONE',  ( -0.7481905315629638897, -9.503618936874122625, 4.126213593628786924 ) ) ;
#6676 = AXIS2_PLACEMENT_3D ( 'NONE', #10826, #17895, #8326 ) ;
#6677 = EDGE_CURVE ( 'NONE', #25878, #1389, #27139, .T. ) ;
#6678 = CARTESIAN_POINT ( 'NONE',  ( 0.000000000000000000, 5.499999999999991118, -76.50000000000001421 ) ) ;
#6679 = SURFACE_SIDE_STYLE ('',( #29863 ) ) ;
#6680 = CARTESIAN_POINT ( 'NONE',  ( -4.763139720814407951, -2.750000000000016431, -74.50000000000001421 ) ) ;
#6681 = DIRECTION ( 'NONE',  ( 1.000000000000000000, -5.551115123125773458E-17, -1.260129944081490338E-35 ) ) ;
#6682 = CARTESIAN_POINT ( 'NONE',  ( 160.8675748654052029, -5.500000000000012434, 2.278174593052012309 ) ) ;
#6683 = FACE_OUTER_BOUND ( 'NONE', #9105, .T. ) ;
#6684 = CARTESIAN_POINT ( 'NONE',  ( 5.196152422706629359, -2.999999999999988898, -75.78867513459486815 ) ) ;
#6685 = CARTESIAN_POINT ( 'NONE',  ( -5.999999999999963585, 8.134310703387671600E-14, -116.9136751345948539 ) ) ;
#6686 = CARTESIAN_POINT ( 'NONE',  ( 20.50000000000015632, -1.999999999999890754, -5.551115123125782702E-14 ) ) ;
#6687 = CARTESIAN_POINT ( 'NONE',  ( -3.464101615137725076, 5.999999999999979572, -55.08632486540518158 ) ) ;
#6688 = CARTESIAN_POINT ( 'NONE',  ( 116.0622167782373566, -1.849990392679381701, 0.7662911109079489913 ) ) ;
#6689 = EDGE_CURVE ( 'NONE', #24216, #14326, #14458, .T. ) ;
#6690 = CYLINDRICAL_SURFACE ( 'NONE', #7624, 5.500000000000000000 ) ;
#6691 = ORIENTED_EDGE ( 'NONE', *, *, #12855, .T. ) ;
#6692 = CARTESIAN_POINT ( 'NONE',  ( 157.1250000000000284, 0.000000000000000000, -6.000000000000005329 ) ) ;
#6693 = SURFACE_STYLE_FILL_AREA ( #18239 ) ;
#6694 = CARTESIAN_POINT ( 'NONE',  ( 5.630955349231442142, 2.071796769705314123, -180.0000000000000568 ) ) ;
#6695 = ORIENTED_EDGE ( 'NONE', *, *, #16059, .T. ) ;
#6696 = EDGE_LOOP ( 'NONE', ( #10839, #11917, #24146, #24268 ) ) ;
#6697 =( BOUNDED_CURVE ( )  B_SPLINE_CURVE ( 2, ( #2812, #5709, #28754, #29204, #19570, #7723, #5861, #5559, #12237 ),
 .UNSPECIFIED., .F., .T. ) 
 B_SPLINE_CURVE_WITH_KNOTS ( ( 3, 2, 2, 2, 3 ),
 ( 0.4083333333333333259, 0.4092592592592592116, 0.4111111111111110938, 0.4129629629629629761, 0.4138888888888888618 ),
 .UNSPECIFIED. ) 
 CURVE ( )  GEOMETRIC_REPRESENTATION_ITEM ( )  RATIONAL_B_SPLINE_CURVE ( ( 0.9330127018922194093, 0.9330127018922194093, 1.000000000000000000, 0.8660254037844388186, 1.000000000000000000, 0.8660254037844388186, 1.000000000000000000, 0.9330127018922234061, 0.9330127018922194093 ) ) 
 REPRESENTATION_ITEM ( '' )  );
#6698 = ORIENTED_EDGE ( 'NONE', *, *, #23133, .T. ) ;
#6699 = CARTESIAN_POINT ( 'NONE',  ( -4.763139720814407951, -2.750000000000016431, -92.50000000000002842 ) ) ;
#6700 = CARTESIAN_POINT ( 'NONE',  ( 3.608439182435180470, 6.249999999999982236, -108.5580127018921957 ) ) ;
#6701 =( BOUNDED_CURVE ( )  B_SPLINE_CURVE ( 2, ( #15195, #5483, #12756, #26531, #10279, #22096, #14889, #7790, #28829, #24230, #19642, #24527, #10431, #29129, #7948, #3181, #17503, #26818, #5781, #26386, #12455, #12603, #5333, #26672, #5632, #3038, #10129, #3328, #21798, #19499, #23891, #9769, #687, #14265, #232, #9616, #19144, #26178, #19444, #16564, #23461, #2834, #2398, #19296, #7446, #5281, #28618, #10072, #526, #14549, #23603, #25885, #28770, #2978, #14688, #24033, #7740, #2681, #18856, #17148, #7589, #4840, #12106, #11810, #9470, #28329, #9922, #14414, #2542, #12256, #28177, #16857, #21445, #26326, #26471, #12399, #377, #21594, #11965, #5427, #21292, #5126, #19007, #7150, #7306, #16712, #16999, #28481, #21747, #4982, #21147, #26035, #85, #23749, #24627, #10847, #8506, #22504, #17915, #3733, #10225, #8348, #20036, #7888, #6047, #20200, #26619, #5574, #12548, #1278, #971, #13004, #5880, #10372, #22035, #3273, #29550, #15464, #27231, #19727, #15138, #3419, #29383, #24181, #21891, #17755, #15302, #829, #5728, #17447, #8038, #29074, #27079, #26762, #22191, #24789, #3126, #12700, #29222, #12847, #3576, #17602, #26919, #24320, #13168, #22343, #19587, #1439, #14837, #28925, #17301, #10689, #14980, #24468, #8187, #1125, #10523, #19877, #13771, #27682, #6342, #15930, #8974, #2212, #22959, #25082, #25385, #6202, #18366, #30312, #11141, #29694, #25226, #24931, #22653, #20490, #23116, #27527, #8667, #6664, #1594, #20961, #2065, #20341, #11303, #11466, #1897, #20810, #27838, #9121, #4344, #20653, #13460, #10997, #18066, #15776, #30158, #4195, #18516, #18211, #3880, #4039, #6505, #27380, #13313, #6807, #16080, #22803, #23271, #1742, #29848, #16233, #25546, #8827, #4508, #11617, #13612, #30000, #13929, #9272, #18666, #15621, #611, #5056, #21819, #455, #10150, #9845, #28856, #17229, #27759, #24635, #25705, #20495, #18215, #1902, #16084, #4351, #13777, #9740, #28448 ),
 .UNSPECIFIED., .F., .T. ) 
 B_SPLINE_CURVE_WITH_KNOTS ( ( 3, 2, 2, 2, 2, 2, 2, 2, 2, 2, 2, 2, 2, 2, 2, 2, 2, 2, 2, 2, 2, 2, 2, 2, 2, 2, 2, 2, 2, 2, 2, 2, 2, 2, 2, 2, 2, 2, 2, 2, 2, 2, 2, 2, 2, 2, 2, 2, 2, 2, 2, 2, 2, 2, 2, 2, 2, 2, 2, 2, 2, 2, 2, 2, 2, 2, 2, 2, 2, 2, 2, 2, 2, 2, 2, 2, 2, 2, 2, 2, 2, 2, 2, 2, 2, 2, 2, 2, 2, 2, 2, 2, 2, 2, 2, 2, 2, 2, 2, 2, 2, 2, 2, 2, 2, 2, 2, 2, 2, 2, 2, 2, 2, 2, 2, 2, 2, 2, 2, 2, 3 ),
 ( 0.000000000000000000, 0.007812500000000366027, 0.01562500000000073205, 0.02343750000000109981, 0.03125000000000146411, 0.03906250000000183881, 0.04687500000000219963, 0.05468750000000256045, 0.06250000000000292821, 0.07031250000000330291, 0.07812500000000367761, 0.08593750000000402456, 0.09375000000000439926, 0.1015625000000047601, 0.1093750000000051209, 0.1171875000000054956, 0.1250000000000058564, 0.1328125000000062450, 0.1406250000000066058, 0.1484375000000069666, 0.1562500000000073552, 0.1640625000000076883, 0.1718750000000080491, 0.1796875000000084377, 0.1875000000000087985, 0.1953125000000091593, 0.2031250000000095202, 0.2109375000000098810, 0.2187500000000102418, 0.2265625000000106304, 0.2343750000000109912, 0.2421875000000113798, 0.2500000000000117129, 0.2578125000000121014, 0.2656250000000124900, 0.2734375000000128231, 0.2812500000000132117, 0.2890625000000135447, 0.2968750000000139333, 0.3046875000000142664, 0.3125000000000147105, 0.3203125000000150435, 0.3281250000000153766, 0.3359375000000157652, 0.3437500000000160982, 0.3515625000000164868, 0.3593750000000168754, 0.3671875000000172085, 0.3750000000000175970, 0.3828125000000179301, 0.3906250000000183187, 0.3984375000000187073, 0.4062500000000190403, 0.4140625000000194289, 0.4218750000000197620, 0.4296875000000201505, 0.4375000000000204836, 0.4453125000000209277, 0.4531250000000212608, 0.4609375000000215938, 0.4687500000000219824, 0.4765625000000223155, 0.4843750000000227596, 0.4921875000000230926, 0.5000000000000234257, 0.5078125000000237588, 0.5156250000000242029, 0.5234375000000245359, 0.5312500000000249800, 0.5390625000000252021, 0.5468750000000256462, 0.5546875000000260902, 0.5625000000000264233, 0.5703125000000267564, 0.5781250000000270894, 0.5859375000000274225, 0.5937500000000278666, 0.6015625000000281997, 0.6093750000000285327, 0.6171875000000288658, 0.6250000000000294209, 0.6328125000000297540, 0.6406250000000300870, 0.6484375000000304201, 0.6562500000000307532, 0.6640625000000311973, 0.6718750000000315303, 0.6796875000000318634, 0.6875000000000321965, 0.6953125000000325295, 0.7031250000000329736, 0.7109375000000334177, 0.7187500000000337508, 0.7265625000000340838, 0.7343750000000344169, 0.7421875000000348610, 0.7500000000000351941, 0.7578125000000355271, 0.7656250000000358602, 0.7734375000000361933, 0.7812500000000366374, 0.7890625000000369704, 0.7968750000000374145, 0.8046875000000377476, 0.8125000000000380806, 0.8203125000000385247, 0.8281250000000388578, 0.8359375000000391909, 0.8437500000000395239, 0.8515625000000398570, 0.8593750000000403011, 0.8671875000000406342, 0.8750000000000409672, 0.8828125000000414113, 0.8906250000000418554, 0.8984375000000421885, 0.9062500000000425215, 0.9140625000000428546, 0.9218750000000431877, 0.9296875000000436318, 0.9375000000000439648 ),
 .UNSPECIFIED. ) 
 CURVE ( )  GEOMETRIC_REPRESENTATION_ITEM ( )  RATIONAL_B_SPLINE_CURVE ( ( 1.000000000000000000, 0.9238795325112867385, 1.000000000000000000, 0.9238795325112867385, 1.000000000000000000, 0.9238795325112867385, 1.000000000000000000, 0.9238795325112867385, 1.000000000000000000, 0.9238795325112867385, 1.000000000000000000, 0.9238795325112867385, 1.000000000000000000, 0.9238795325112867385, 1.000000000000000000, 0.9238795325112867385, 1.000000000000000000, 0.9238795325112867385, 1.000000000000000000, 0.9238795325112867385, 1.000000000000000000, 0.9238795325112867385, 1.000000000000000000, 0.9238795325112867385, 1.000000000000000000, 0.9238795325112867385, 1.000000000000000000, 0.9238795325112867385, 1.000000000000000000, 0.9238795325112867385, 1.000000000000000000, 0.9238795325112867385, 1.000000000000000000, 0.9238795325112867385, 1.000000000000000000, 0.9238795325112867385, 1.000000000000000000, 0.9238795325112867385, 1.000000000000000000, 0.9238795325112867385, 1.000000000000000000, 0.9238795325112867385, 1.000000000000000000, 0.9238795325112867385, 1.000000000000000000, 0.9238795325112867385, 1.000000000000000000, 0.9238795325112867385, 1.000000000000000000, 0.9238795325112867385, 1.000000000000000000, 0.9238795325112867385, 1.000000000000000000, 0.9238795325112867385, 1.000000000000000000, 0.9238795325112867385, 1.000000000000000000, 0.9238795325112867385, 1.000000000000000000, 0.9238795325112867385, 1.000000000000000000, 0.9238795325112867385, 1.000000000000000000, 0.9238795325112867385, 1.000000000000000000, 0.9238795325112867385, 1.000000000000000000, 0.9238795325112867385, 1.000000000000000000, 0.9238795325112867385, 1.000000000000000000, 0.9238795325112867385, 1.000000000000000000, 0.9238795325112867385, 1.000000000000000000, 0.9238795325112867385, 1.000000000000000000, 0.9238795325112867385, 1.000000000000000000, 0.9238795325112867385, 1.000000000000000000, 0.9238795325112867385, 1.000000000000000000, 0.9238795325112867385, 1.000000000000000000, 0.9238795325112867385, 1.000000000000000000, 0.9238795325112867385, 1.000000000000000000, 0.9238795325112867385, 1.000000000000000000, 0.9238795325112867385, 1.000000000000000000, 0.9238795325112867385, 1.000000000000000000, 0.9238795325112867385, 1.000000000000000000, 0.9238795325112867385, 1.000000000000000000, 0.9238795325112867385, 1.000000000000000000, 0.9238795325112867385, 1.000000000000000000, 0.9238795325112867385, 1.000000000000000000, 0.9238795325112867385, 1.000000000000000000, 0.9238795325112867385, 1.000000000000000000, 0.9238795325112867385, 1.000000000000000000, 0.9238795325112867385, 1.000000000000000000, 0.9238795325112867385, 1.000000000000000000, 0.9238795325112867385, 1.000000000000000000, 0.9238795325112867385, 1.000000000000000000, 0.9238795325112867385, 1.000000000000000000, 0.9238795325112867385, 1.000000000000000000, 0.9238795325112867385, 1.000000000000000000, 0.9238795325112867385, 1.000000000000000000, 0.9238795325112867385, 1.000000000000000000, 0.9238795325112867385, 1.000000000000000000, 0.9238795325112867385, 1.000000000000000000, 0.9238795325112867385, 1.000000000000000000, 0.9238795325112867385, 1.000000000000000000, 0.9238795325112867385, 1.000000000000000000, 0.9238795325112867385, 1.000000000000000000, 0.9238795325112867385, 1.000000000000000000, 0.9238795325112867385, 1.000000000000000000, 0.9238795325112867385, 1.000000000000000000, 0.9238795325112867385, 1.000000000000000000, 0.9238795325112867385, 1.000000000000000000, 0.9238795325112867385, 1.000000000000000000, 0.9238795325112867385, 1.000000000000000000, 0.9238795325112867385, 1.000000000000000000, 0.9238795325112867385, 1.000000000000000000, 0.9238795325112867385, 1.000000000000000000, 0.9238795325112867385, 1.000000000000000000, 0.9238795325112867385, 1.000000000000000000, 0.9238795325112867385, 1.000000000000000000, 0.9238795325112867385, 1.000000000000000000, 0.9238795325112867385, 1.000000000000000000, 0.9238795325112867385, 1.000000000000000000, 0.9238795325112867385, 1.000000000000000000, 0.9238795325112867385, 1.000000000000000000, 0.9238795325112867385, 1.000000000000000000, 0.9238795325112867385, 1.000000000000000000, 0.9238795325112867385, 1.000000000000000000, 0.9238795325112867385, 1.000000000000000000, 0.9238795325112867385, 1.000000000000000000, 0.9238795325112867385, 1.000000000000000000, 0.9238795325112867385, 1.000000000000000000, 0.9238795325112867385, 1.000000000000000000, 0.9238795325112867385, 1.000000000000000000, 0.9238795325112867385, 1.000000000000000000, 0.9238795325112867385, 1.000000000000000000, 0.9238795325112867385, 1.000000000000000000, 0.9238795325112867385, 1.000000000000000000, 0.9238795325112867385, 1.000000000000000000, 0.9238795325112867385, 1.000000000000000000, 0.9238795325112867385, 1.000000000000000000, 0.9238795325112867385, 1.000000000000000000, 0.9238795325112867385, 1.000000000000000000, 0.9238795325112867385, 1.000000000000000000, 0.9238795325112867385, 1.000000000000000000, 0.9238795325112867385, 1.000000000000000000, 0.9238795325112867385, 1.000000000000000000, 0.9238795325112867385, 1.000000000000000000, 0.9238795325112867385, 1.000000000000000000, 0.9238795325112867385, 1.000000000000000000, 0.9238795325112867385, 1.000000000000000000, 0.9238795325112867385, 1.000000000000000000, 0.9238795325112867385, 1.000000000000000000, 0.9238795325112867385, 1.000000000000000000, 0.9238795325112867385, 1.000000000000000000, 0.9238795325112867385, 1.000000000000000000, 0.9238795325108584144, 1.000000000000428324 ) ) 
 REPRESENTATION_ITEM ( '' )  );
#6702 = ORIENTED_EDGE ( 'NONE', *, *, #20923, .T. ) ;
#6703 =( NAMED_UNIT ( * ) PLANE_ANGLE_UNIT ( ) SI_UNIT ( $, .RADIAN. ) );
#6704 = CARTESIAN_POINT ( 'NONE',  ( 0.8033614493835260495, -15.44729320518831805, 8.224148781931267749 ) ) ;
#6705 = CARTESIAN_POINT ( 'NONE',  ( 6.350852961086080661, -9.614813431917819062E-14, -162.3750000000000284 ) ) ;
#6706 = CARTESIAN_POINT ( 'NONE',  ( 0.000000000000000000, -5.999999999999991118, -106.0386751345948682 ) ) ;
#6707 = ORIENTED_EDGE ( 'NONE', *, *, #19452, .T. ) ;
#6708 = CARTESIAN_POINT ( 'NONE',  ( 6.000000000000000888, -1.607695154586752384, -67.65331216351302146 ) ) ;
#6709 = MECHANICAL_DESIGN_GEOMETRIC_PRESENTATION_REPRESENTATION (  '', ( #29240 ), #14131 ) ;
#6710 = CARTESIAN_POINT ( 'NONE',  ( 3.175426480543072749, -5.500000000000105693, -173.1250000000000284 ) ) ;
#6711 = FACE_OUTER_BOUND ( 'NONE', #5881, .T. ) ;
#6712 = CARTESIAN_POINT ( 'NONE',  ( 4.763139720814407951, -2.749999999999988454, -161.0000000000000284 ) ) ;
#6713 = CARTESIAN_POINT ( 'NONE',  ( 118.1874999999997158, 1.035533905932719101, 2.500000000000205169 ) ) ;
#6714 = EDGE_CURVE ( 'NONE', #18709, #13261, #6964, .T. ) ;
#6715 = FACE_OUTER_BOUND ( 'NONE', #5622, .T. ) ;
#6716 = CARTESIAN_POINT ( 'NONE',  ( 145.7738248654052313, -3.889087296526011706, 3.889087296526011706 ) ) ;
#6717 = ADVANCED_FACE ( 'NONE', ( #28890 ), #7856, .T. ) ;
#6718 = CARTESIAN_POINT ( 'NONE',  ( 4.763139720814407951, -2.749999999999988454, -93.50000000000002842 ) ) ;
#6719 = PRODUCT_DEFINITION ( 'UNKNOWN', '', #3098, #6790 ) ;
#6720 = CARTESIAN_POINT ( 'NONE',  ( 162.4836002691897079, 4.999999999999989342, -2.071067811865468400 ) ) ;
#6721 = CARTESIAN_POINT ( 'NONE',  ( 135.0000000000000284, -7.706858840103492092, 8.197103070889301790 ) ) ;
#6722 = EDGE_LOOP ( 'NONE', ( #11304, #23303, #78, #27062 ) ) ;
#6723 = CARTESIAN_POINT ( 'NONE',  ( 15.72617513459489302, -2.499999999999964473, 1.035533905932869425 ) ) ;
#6724 = CARTESIAN_POINT ( 'NONE',  ( 107.0002832217622597, -1.308140751793585022, -1.308140751793640533 ) ) ;
#6725 = DIRECTION ( 'NONE',  ( -0.000000000000000000, -0.000000000000000000, -1.000000000000000000 ) ) ;
#6726 = ORIENTED_EDGE ( 'NONE', *, *, #2712, .F. ) ;
#6727 = FILL_AREA_STYLE_COLOUR ( '', #19203 ) ;
#6728 = CARTESIAN_POINT ( 'NONE',  ( 3.608439182435180470, 6.249999999999982236, -86.69198729810781856 ) ) ;
#6729 = VECTOR ( 'NONE', #23843, 1000.000000000000000 ) ;
#6730 = DIRECTION ( 'NONE',  ( 1.000000000000000000, 0.000000000000000000, 0.000000000000000000 ) ) ;
#6731 = CARTESIAN_POINT ( 'NONE',  ( 150.3750000000000284, 0.000000000000000000, 6.000000000000005329 ) ) ;
#6732 = VERTEX_POINT ( 'NONE', #5544 ) ;
#6733 = CARTESIAN_POINT ( 'NONE',  ( -4.763139720814407951, -2.750000000000016431, -122.5000000000000568 ) ) ;
#6734 = CARTESIAN_POINT ( 'NONE',  ( 23.31250000000013500, 2.649519052838419153, -1.097466725451619718 ) ) ;
#6735 = CARTESIAN_POINT ( 'NONE',  ( -5.412658773652684552, -3.125000000000099920, -134.9330127018922383 ) ) ;
#6736 = EDGE_LOOP ( 'NONE', ( #5171, #6804, #18272, #936 ) ) ;
#6737 = SURFACE_STYLE_FILL_AREA ( #28369 ) ;
#6738 = CARTESIAN_POINT ( 'NONE',  ( 3.608439182435180470, -6.249999999999997335, -165.1919872981078186 ) ) ;
#6739 = CARTESIAN_POINT ( 'NONE',  ( 2.775557561562891351E-14, -6.250000000000061284, -180.3169872981078470 ) ) ;
#6740 = VECTOR ( 'NONE', #14599, 1000.000000000000000 ) ;
#6741 =( BOUNDED_CURVE ( )  B_SPLINE_CURVE ( 2, ( #23541, #25356, #2185, #2341, #6933, #18793, #4326, #7088, #2480 ),
 .UNSPECIFIED., .F., .F. ) 
 B_SPLINE_CURVE_WITH_KNOTS ( ( 3, 2, 2, 2, 3 ),
 ( 0.5805555555555554914, 0.5814814814814814881, 0.5833333333333332593, 0.5851851851851852526, 0.5861111111111111382 ),
 .UNSPECIFIED. ) 
 CURVE ( )  GEOMETRIC_REPRESENTATION_ITEM ( )  RATIONAL_B_SPLINE_CURVE ( ( 0.9330127018922194093, 0.9330127018922154125, 1.000000000000000000, 0.8660254037844388186, 1.000000000000000000, 0.8660254037844388186, 1.000000000000000000, 0.9330127018922194093, 0.9330127018922194093 ) ) 
 REPRESENTATION_ITEM ( '' )  );
#6742 = SURFACE_STYLE_FILL_AREA ( #27764 ) ;
#6743 = CARTESIAN_POINT ( 'NONE',  ( 6.000000000000000888, 1.607695154586715303, -147.5966878364871206 ) ) ;
#6744 = ORIENTED_EDGE ( 'NONE', *, *, #24589, .F. ) ;
#6745 = CARTESIAN_POINT ( 'NONE',  ( 13.00000000000003908, 2.000000000000112799, 0.000000000000000000 ) ) ;
#6746 = CARTESIAN_POINT ( 'NONE',  ( -3.464101615137725076, 5.999999999999979572, -54.16367513459480421 ) ) ;
#6747 = CARTESIAN_POINT ( 'NONE',  ( 3.847734726291792473, 4.353436196503639444, -180.0000000000000000 ) ) ;
#6748 = CARTESIAN_POINT ( 'NONE',  ( 3.464101615137852974, 5.999999999999884537, -136.9136751345947971 ) ) ;
#6749 = CARTESIAN_POINT ( 'NONE',  ( 22.96132486540528106, 1.665334536937734811E-13, 2.499999999999946709 ) ) ;
#6750 = CARTESIAN_POINT ( 'NONE',  ( 7.216878364870455975, -6.409875621278545621E-14, -73.44198729810783277 ) ) ;
#6751 = CARTESIAN_POINT ( 'NONE',  ( 3.608439182435180470, 6.249999999999982236, -62.69198729810783277 ) ) ;
#6752 = CARTESIAN_POINT ( 'NONE',  ( 4.763139720814407951, 2.750000000000002665, -51.25000000000001421 ) ) ;
#6753 = CARTESIAN_POINT ( 'NONE',  ( -0.6001665993698070967, -9.799666801260325855, -4.385453238887226490 ) ) ;
#6754 = CARTESIAN_POINT ( 'NONE',  ( -3.464101615137725076, 5.999999999999979572, -159.1636751345948255 ) ) ;
#6755 = EDGE_CURVE ( 'NONE', #11541, #13814, #16790, .T. ) ;
#6756 = CARTESIAN_POINT ( 'NONE',  ( -3.175426480542816510, -5.500000000000057732, -120.8750000000000284 ) ) ;
#6757 = CARTESIAN_POINT ( 'NONE',  ( 135.0000000000000284, -8.852647312720215211, -7.500000050752666958 ) ) ;
#6758 = CARTESIAN_POINT ( 'NONE',  ( -1.285375204280330350E-15, -10.49588505988223375, 1.184433945098074864E-34 ) ) ;
#6759 = EDGE_LOOP ( 'NONE', ( #11136, #27828, #27434, #15462, #5526 ) ) ;
#6760 = CARTESIAN_POINT ( 'NONE',  ( 21.06250000000011013, -2.649519052838118061, 1.097466725451439196 ) ) ;
#6761 = CARTESIAN_POINT ( 'NONE',  ( -4.999999999999886313, -70.00000000000001421, 8.000000000000007105 ) ) ;
#6762 = DIRECTION ( 'NONE',  ( 1.000000000000000000, -5.551115123125773458E-17, -1.260129944081490338E-35 ) ) ;
#6763 = ORIENTED_EDGE ( 'NONE', *, *, #7915, .T. ) ;
#6764 = CARTESIAN_POINT ( 'NONE',  ( 110.0622167782374987, -1.849990392679441875, 0.7662911109079489913 ) ) ;
#6765 = CARTESIAN_POINT ( 'NONE',  ( 150.9300748654052313, 2.278174593051795149, -5.500000000000228262 ) ) ;
#6766 = CARTESIAN_POINT ( 'NONE',  ( 112.6872167782374419, 1.849990392679621953, 0.7662911109081291805 ) ) ;
#6767 = CARTESIAN_POINT ( 'NONE',  ( 3.608439182435180470, -6.249999999999997335, -108.1919872981077901 ) ) ;
#6768 = CARTESIAN_POINT ( 'NONE',  ( 17.02382486540524553, -1.035533905932508825, 2.499999999999844569 ) ) ;
#6769 = CARTESIAN_POINT ( 'NONE',  ( 104.7401757384973280, 1.387249626875697306, 1.223929297688219897 ) ) ;
#6770 = AXIS2_PLACEMENT_3D ( 'NONE', #3480, #24691, #15200 ) ;
#6771 = ORIENTED_EDGE ( 'NONE', *, *, #2557, .T. ) ;
#6772 = ORIENTED_EDGE ( 'NONE', *, *, #1788, .F. ) ;
#6773 = CARTESIAN_POINT ( 'NONE',  ( 20.72617513459479355, -2.499999999999964473, 1.035533905932749299 ) ) ;
#6774 = CARTESIAN_POINT ( 'NONE',  ( 137.0625000000000284, -4.242640687119298093, 4.242640687119298093 ) ) ;
#6775 = EDGE_LOOP ( 'NONE', ( #21520, #2262, #6792, #1009 ) ) ;
#6776 = CARTESIAN_POINT ( 'NONE',  ( -7.216878364870328078, 0.000000000000000000, -143.1919872981078186 ) ) ;
#6777 = DIRECTION ( 'NONE',  ( 1.000000000000000000, 0.000000000000000000, 0.000000000000000000 ) ) ;
#6778 = ADVANCED_FACE ( 'NONE', ( #25047 ), #16047, .F. ) ;
#6779 = CARTESIAN_POINT ( 'NONE',  ( 15.03867513459491967, 1.665334536937734811E-13, -2.500000000000057732 ) ) ;
#6780 = CARTESIAN_POINT ( 'NONE',  ( 23.50000000000010303, -1.999999999999779732, -5.551115123125782702E-14 ) ) ;
#6781 = CARTESIAN_POINT ( 'NONE',  ( 5.412658773652739619, 3.124999999999988898, -71.18301270189225249 ) ) ;
#6782 = CARTESIAN_POINT ( 'NONE',  ( 145.3913997308104058, -2.071067811865468400, 4.999999999999989342 ) ) ;
#6783 = CARTESIAN_POINT ( 'NONE',  ( 115.2113248654050750, -1.999999999999918510, 1.110223024625156540E-13 ) ) ;
#6784 = CARTESIAN_POINT ( 'NONE',  ( -5.999999999999963585, 9.296355089585909904E-15, -164.9136751345948255 ) ) ;
#6785 = DIRECTION ( 'NONE',  ( -1.000000000000000000, -1.665334536937731113E-16, 1.526556658859586792E-16 ) ) ;
#6786 = CARTESIAN_POINT ( 'NONE',  ( 110.1874999999997584, 1.035533905932779275, 2.500000000000205169 ) ) ;
#6787 =( BOUNDED_CURVE ( )  B_SPLINE_CURVE ( 2, ( #7431, #28907, #24167, #2520, #12383, #7872, #21273, #12088, #2817 ),
 .UNSPECIFIED., .F., .T. ) 
 B_SPLINE_CURVE_WITH_KNOTS ( ( 3, 2, 2, 2, 3 ),
 ( 0.7083333333333333703, 0.7092592592592592560, 0.7111111111111111382, 0.7129629629629629095, 0.7138888888888887951 ),
 .UNSPECIFIED. ) 
 CURVE ( )  GEOMETRIC_REPRESENTATION_ITEM ( )  RATIONAL_B_SPLINE_CURVE ( ( 0.9330127018922194093, 0.9330127018922234061, 1.000000000000000000, 0.8660254037844388186, 1.000000000000000000, 0.8660254037844388186, 1.000000000000000000, 0.9330127018922234061, 0.9330127018922194093 ) ) 
 REPRESENTATION_ITEM ( '' )  );
#6788 = ADVANCED_FACE ( 'NONE', ( #25506 ), #23886, .F. ) ;
#6789 = CARTESIAN_POINT ( 'NONE',  ( 3.175426480543072749, 5.499999999999865885, -126.1250000000000426 ) ) ;
#6790 = PRODUCT_DEFINITION_CONTEXT ( 'detailed design', #22635, 'design' ) ;
#6791 =( NAMED_UNIT ( * ) PLANE_ANGLE_UNIT ( ) SI_UNIT ( $, .RADIAN. ) );
#6792 = ORIENTED_EDGE ( 'NONE', *, *, #23791, .F. ) ;
#6793 = CARTESIAN_POINT ( 'NONE',  ( -2.775557561562891351E-14, -5.500000000000115463, -51.75000000000002132 ) ) ;
#6794 = CARTESIAN_POINT ( 'NONE',  ( -6.000000000000023093, 1.607695154586625819, -123.9033121635129646 ) ) ;
#6795 = FACE_OUTER_BOUND ( 'NONE', #18964, .T. ) ;
#6796 = ORIENTED_EDGE ( 'NONE', *, *, #16874, .T. ) ;
#6797 = CARTESIAN_POINT ( 'NONE',  ( 120.5622167782374419, 1.849990392679652151, -0.7662911109075283278 ) ) ;
#6798 = CARTESIAN_POINT ( 'NONE',  ( 138.3750000000000284, 0.000000000000000000, 6.000000000000005329 ) ) ;
#6799 = CARTESIAN_POINT ( 'NONE',  ( 13.43750000000012612, -1.999999999999971800, 0.8284271247462354770 ) ) ;
#6800 = CARTESIAN_POINT ( 'NONE',  ( 3.608439182435180470, -6.249999999999997335, -100.6919872981078328 ) ) ;
#6801 = CARTESIAN_POINT ( 'NONE',  ( 6.000000000000000888, -3.330669073875464691E-16, -7.560779664488942560E-35 ) ) ;
#6802 = CARTESIAN_POINT ( 'NONE',  ( 137.1562500000000284, -6.000000000000005329, 2.485281374238555774 ) ) ;
#6803 = DIRECTION ( 'NONE',  ( -1.000000000000000000, 0.000000000000000000, 0.000000000000000000 ) ) ;
#6804 = ORIENTED_EDGE ( 'NONE', *, *, #10167, .T. ) ;
#6805 = B_SPLINE_CURVE_WITH_KNOTS ( 'NONE', 3,
 ( #22042, #5582, #17155, #7593, #3425, #21901, #26334, #14987, #5285, #980, #10379, #14694, #24040, #24326, #2986, #8044, #13465, #1903 ),
 .UNSPECIFIED., .F., .F.,
 ( 4, 2, 2, 2, 2, 2, 2, 2, 4 ),
 ( 0.000000000000000000, 0.0005121067916087861365, 0.001024213583217572273, 0.001536320374826358626, 0.002048427166435145413, 0.002560533958043931767, 0.003072640749652718120, 0.003584747541261505341, 0.004096854332870291694 ),
 .UNSPECIFIED. ) ;
#6806 = CARTESIAN_POINT ( 'NONE',  ( -4.763139720814407951, 2.749999999999946709, -137.7500000000000284 ) ) ;
#6807 = CARTESIAN_POINT ( 'NONE',  ( 12.18750000000008349, 0.8284271247463557142, 1.999999999999851674 ) ) ;
#6808 = ORIENTED_EDGE ( 'NONE', *, *, #10567, .T. ) ;
#6809 = EDGE_CURVE ( 'NONE', #22830, #4838, #9171, .T. ) ;
#6810 = CARTESIAN_POINT ( 'NONE',  ( -4.763139720814407951, 2.749999999999946709, -64.25000000000002842 ) ) ;
#6811 = CARTESIAN_POINT ( 'NONE',  ( 5.999999999999999112, 2.951592740943527306E-14, -164.1636751345948824 ) ) ;
#6812 = VECTOR ( 'NONE', #14470, 1000.000000000000000 ) ;
#6813 = CARTESIAN_POINT ( 'NONE',  ( -5.196152422706601826, 2.999999999999975131, -139.5386751345948255 ) ) ;
#6814 = CARTESIAN_POINT ( 'NONE',  ( 0.000000000000000000, 0.000000000000000000, 0.000000000000000000 ) ) ;
#6815 = CARTESIAN_POINT ( 'NONE',  ( 140.5828481527998974, -11.16569630559845017, -4.440052304731437083 ) ) ;
#6816 = CARTESIAN_POINT ( 'NONE',  ( 117.9377832217621744, -1.849990392679441875, -0.7662911109075883909 ) ) ;
#6817 = ADVANCED_FACE ( 'NONE', ( #13738 ), #29815, .F. ) ;
#6818 = CARTESIAN_POINT ( 'NONE',  ( 3.175426480543072749, 5.499999999999865885, -145.6250000000000000 ) ) ;
#6819 = CARTESIAN_POINT ( 'NONE',  ( 139.6521270721804342, -8.798545340575019580, -8.159999993250346861 ) ) ;
#6820 = CARTESIAN_POINT ( 'NONE',  ( -4.763139720814407951, -2.750000000000016431, -137.5000000000000000 ) ) ;
#6821 = CARTESIAN_POINT ( 'NONE',  ( -5.412658773652684552, -3.125000000000099920, -161.9330127018922667 ) ) ;
#6822 = CARTESIAN_POINT ( 'NONE',  ( 0.000000000000000000, 0.000000000000000000, 0.000000000000000000 ) ) ;
#6823 = CARTESIAN_POINT ( 'NONE',  ( 105.4613248654050324, 0.000000000000000000, -2.000000000000001776 ) ) ;
#6824 = CARTESIAN_POINT ( 'NONE',  ( 0.000000000000000000, 5.499999999999991118, -81.00000000000001421 ) ) ;
#6825 = CARTESIAN_POINT ( 'NONE',  ( 4.763139720814407951, 2.750000000000002665, -75.25000000000004263 ) ) ;
#6826 = CARTESIAN_POINT ( 'NONE',  ( 3.464101615137757051, -5.999999999999979572, -156.3363248654052313 ) ) ;
#6827 = CARTESIAN_POINT ( 'NONE',  ( 149.1711002691896795, 4.999999999999989342, 2.071067811865468400 ) ) ;
#6828 = CARTESIAN_POINT ( 'NONE',  ( 160.6800748654052029, -2.278174593052130881, 5.499999999999894307 ) ) ;
#6829 = DIRECTION ( 'NONE',  ( -1.000000000000000000, -1.665334536937731113E-16, 1.526556658859586792E-16 ) ) ;
#6830 = CARTESIAN_POINT ( 'NONE',  ( 155.7187500000000568, 2.485281374238556218, -6.000000000000005329 ) ) ;
#6831 = CARTESIAN_POINT ( 'NONE',  ( 6.000000000000000888, 7.762456499804234384E-14, -134.1636751345948539 ) ) ;
#6832 = CARTESIAN_POINT ( 'NONE',  ( 140.5384615384615756, -11.07692307692306777, -4.615384615384604317 ) ) ;
#6833 =( BOUNDED_SURFACE ( )  B_SPLINE_SURFACE ( 3, 2, ( 
 ( #9779, #7458, #17009 ),
 ( #17158, #16867, #26190 ),
 ( #26338, #23901, #5288 ),
 ( #26478, #5437, #24191 ) ),
 .UNSPECIFIED., .F., .F., .F. ) 
 B_SPLINE_SURFACE_WITH_KNOTS ( ( 4, 4 ),
 ( 3, 3 ),
 ( 0.000000000000000000, 0.0002125775066526910278 ),
 ( 0.000000000000000000, 1.000000000000000000 ),
 .UNSPECIFIED. ) 
 GEOMETRIC_REPRESENTATION_ITEM ( )  RATIONAL_B_SPLINE_SURFACE ( (
 ( 1.000000000000000000, 0.7071067811865475727, 1.000000000000000000),
 ( 1.000000000000000000, 0.7257758655053210273, 1.000000000000000000),
 ( 1.000000000000000000, 0.7424605758826430257, 1.000000000000000000),
 ( 1.000000000000000000, 0.7576044462920076272, 1.000000000000000000) ) ) 
 REPRESENTATION_ITEM ( '' )  SURFACE ( )  );
#6834 = MECHANICAL_DESIGN_GEOMETRIC_PRESENTATION_REPRESENTATION (  '', ( #9785 ), #12745 ) ;
#6835 = CARTESIAN_POINT ( 'NONE',  ( -5.196152422706573404, -3.000000000000002665, -147.7113248654052313 ) ) ;
#6836 = CARTESIAN_POINT ( 'NONE',  ( 119.0622167782374561, -1.849990392679381701, 0.7662911109078888172 ) ) ;
#6837 = CARTESIAN_POINT ( 'NONE',  ( 0.000000000000000000, 5.999999999999977796, -169.7886751345948255 ) ) ;
#6838 = ORIENTED_EDGE ( 'NONE', *, *, #8248, .F. ) ;
#6839 = VECTOR ( 'NONE', #21511, 1000.000000000000000 ) ;
#6840 = CARTESIAN_POINT ( 'NONE',  ( 158.1562500000000284, -6.000000000000005329, 2.485281374238555774 ) ) ;
#6841 = PRESENTATION_STYLE_ASSIGNMENT (( #9465 ) ) ;
#6842 = CARTESIAN_POINT ( 'NONE',  ( -5.999999999999963585, 1.780251999655701777E-13, -85.41367513459483973 ) ) ;
#6843 = VERTEX_POINT ( 'NONE', #8627 ) ;
#6844 = VERTEX_POINT ( 'NONE', #8944 ) ;
#6845 = ORIENTED_EDGE ( 'NONE', *, *, #18471, .T. ) ;
#6846 = EDGE_CURVE ( 'NONE', #25883, #16005, #10964, .T. ) ;
#6847 = CARTESIAN_POINT ( 'NONE',  ( 4.763139720814407951, 2.750000000000002665, -91.75000000000000000 ) ) ;
#6848 = CARTESIAN_POINT ( 'NONE',  ( -3.608439182435052128, -6.250000000000110134, -106.3080127018922667 ) ) ;
#6849 = ORIENTED_EDGE ( 'NONE', *, *, #2322, .F. ) ;
#6850 = CARTESIAN_POINT ( 'NONE',  ( 6.000000000000000888, -1.859271017917181981E-14, -68.16367513459481131 ) ) ;
#6851 = CARTESIAN_POINT ( 'NONE',  ( -0.5000000000000004441, -24.99999999999999289, 8.000000000000007105 ) ) ;
#6852 = CARTESIAN_POINT ( 'NONE',  ( 2.775557561562891351E-14, 6.250000000000033751, -48.43301270189226670 ) ) ;
#6853 = AXIS2_PLACEMENT_3D ( 'NONE', #17194, #14732, #14877 ) ;
#6854 = ORIENTED_EDGE ( 'NONE', *, *, #15664, .T. ) ;
#6855 = EDGE_CURVE ( 'NONE', #8188, #17667, #27651, .T. ) ;
#6856 = CARTESIAN_POINT ( 'NONE',  ( 13.99999999999999822, 0.000000000000000000, -16.50000000000000355 ) ) ;
#6857 = AXIS2_PLACEMENT_3D ( 'NONE', #13284, #22627, #15742 ) ;
#6858 = CARTESIAN_POINT ( 'NONE',  ( -2.775557561562891351E-14, -5.500000000000115463, -168.7500000000000000 ) ) ;
#6859 = CARTESIAN_POINT ( 'NONE',  ( -5.999999999999963585, -1.487416814333745711E-14, -80.91367513459482552 ) ) ;
#6860 = CARTESIAN_POINT ( 'NONE',  ( -3.175426480542816510, -5.500000000000057732, -161.3750000000000284 ) ) ;
#6861 = AXIS2_PLACEMENT_3D ( 'NONE', #22704, #4093, #13513 ) ;
#6862 = CARTESIAN_POINT ( 'NONE',  ( 113.6874999999998437, -1.035533905932749299, -2.499999999999904521 ) ) ;
#6863 =( GEOMETRIC_REPRESENTATION_CONTEXT ( 3 ) GLOBAL_UNCERTAINTY_ASSIGNED_CONTEXT ( ( #8387 ) ) GLOBAL_UNIT_ASSIGNED_CONTEXT ( ( #22279, #15822, #6387 ) ) REPRESENTATION_CONTEXT ( 'NONE', 'WORKASPACE' ) );
#6864 = CYLINDRICAL_SURFACE ( 'NONE', #14445, 5.500000000000000000 ) ;
#6865 = CARTESIAN_POINT ( 'NONE',  ( 0.000000000000000000, 5.999999999999977796, -87.28867513459481131 ) ) ;
#6866 = CARTESIAN_POINT ( 'NONE',  ( -4.763139720814407951, -2.750000000000016431, -98.50000000000002842 ) ) ;
#6867 = CARTESIAN_POINT ( 'NONE',  ( 24.50000000000013145, 0.6095397824029125111, -2.424553825690234365 ) ) ;
#6868 = CARTESIAN_POINT ( 'NONE',  ( 161.1711002691896795, 4.999999999999989342, 2.071067811865468400 ) ) ;
#6869 = CARTESIAN_POINT ( 'NONE',  ( -5.999999999999963585, -1.487416814333745711E-14, -143.3363248654052029 ) ) ;
#6870 = ORIENTED_EDGE ( 'NONE', *, *, #9918, .F. ) ;
#6871 = CARTESIAN_POINT ( 'NONE',  ( 12.68750000000007638, 2.649519052838538613, 1.097466725451439196 ) ) ;
#6872 = CARTESIAN_POINT ( 'NONE',  ( 113.3749999999999289, -1.767766952966293159, 1.767766952966431937 ) ) ;
#6873 = CARTESIAN_POINT ( 'NONE',  ( 12.77382486540536455, 2.500000000000084821, 1.035533905932689347 ) ) ;
#6874 = CARTESIAN_POINT ( 'NONE',  ( 106.1877832217621318, 0.7662911109077987781, -1.849990392679351725 ) ) ;
#6875 = CARTESIAN_POINT ( 'NONE',  ( -5.999999999999963585, 1.780251999655701777E-13, -86.33632486540524553 ) ) ;
#6876 =( BOUNDED_CURVE ( )  B_SPLINE_CURVE ( 2, ( #28400, #308, #23675, #7075, #28253, #6916, #11885, #16489, #4763 ),
 .UNSPECIFIED., .F., .T. ) 
 B_SPLINE_CURVE_WITH_KNOTS ( ( 3, 2, 2, 2, 3 ),
 ( 0.6875000000000002220, 0.6937500000000004219, 0.7000000000000006217, 0.7062500000000009326, 0.7125000000000011324 ),
 .UNSPECIFIED. ) 
 CURVE ( )  GEOMETRIC_REPRESENTATION_ITEM ( )  RATIONAL_B_SPLINE_CURVE ( ( 0.9999999999999973355, 0.9238795325112894030, 1.000000000000000000, 0.9238795325112867385, 1.000000000000000000, 0.9238795325112867385, 1.000000000000000000, 0.9238795325112731938, 1.000000000000013545 ) ) 
 REPRESENTATION_ITEM ( '' )  );
#6877 = ORIENTED_EDGE ( 'NONE', *, *, #29535, .T. ) ;
#6878 = EDGE_LOOP ( 'NONE', ( #29106, #24437, #11302, #25001 ) ) ;
#6879 = DIRECTION ( 'NONE',  ( 0.000000000000000000, 5.551115123125767911E-17, -1.000000000000000000 ) ) ;
#6880 = CIRCLE ( 'NONE', #12320, 1.000000000000000444 ) ;
#6881 = CARTESIAN_POINT ( 'NONE',  ( 149.4375000000000284, -4.242640687119298093, -4.242640687119298093 ) ) ;
#6882 = AXIS2_PLACEMENT_3D ( 'NONE', #8130, #10164, #17245 ) ;
#6883 = EDGE_LOOP ( 'NONE', ( #816, #17084, #14307, #5247 ) ) ;
#6884 = ADVANCED_FACE ( 'NONE', ( #23081 ), #2319, .F. ) ;
#6885 = CARTESIAN_POINT ( 'NONE',  ( -4.763139720814407951, 2.749999999999946709, -115.2500000000000142 ) ) ;
#6886 = CARTESIAN_POINT ( 'NONE',  ( 21.00000000000012790, -1.873492889144789952, -1.873492889145011997 ) ) ;
#6887 = EDGE_CURVE ( 'NONE', #24855, #10410, #12510, .T. ) ;
#6888 = CARTESIAN_POINT ( 'NONE',  ( 2.775557561562891351E-14, 6.250000000000033751, -132.4330127018922383 ) ) ;
#6889 = ORIENTED_EDGE ( 'NONE', *, *, #25003, .F. ) ;
#6890 = FILL_AREA_STYLE_COLOUR ( '', #25460 ) ;
#6891 = CARTESIAN_POINT ( 'NONE',  ( 2.775557561562891351E-14, 6.250000000000033751, -172.0669872981078186 ) ) ;
#6892 = CARTESIAN_POINT ( 'NONE',  ( -3.608439182435115633, 6.249999999999965361, -180.9419872981078186 ) ) ;
#6893 = CYLINDRICAL_SURFACE ( 'NONE', #25554, 2.499999999999999112 ) ;
#6894 = ORIENTED_EDGE ( 'NONE', *, *, #8693, .F. ) ;
#6895 = DIRECTION ( 'NONE',  ( -7.147005652999508048E-36, 5.642372883946980038E-36, 1.000000000000000000 ) ) ;
#6896 = CARTESIAN_POINT ( 'NONE',  ( 112.2738248654049471, -1.999999999999941602, -0.8284271247459952248 ) ) ;
#6897 = CARTESIAN_POINT ( 'NONE',  ( 109.3752832217621744, 1.849990392679579099, 1.110223024625156540E-13 ) ) ;
#6898 = CARTESIAN_POINT ( 'NONE',  ( 3.608439182435180470, 6.249999999999982236, -77.69198729810784698 ) ) ;
#6899 = CARTESIAN_POINT ( 'NONE',  ( -3.608439182435115633, 6.249999999999965361, -60.94198729810783277 ) ) ;
#6900 = CARTESIAN_POINT ( 'NONE',  ( 3.608439182435180470, -6.249999999999997335, -181.0580127018922099 ) ) ;
#6901 = CARTESIAN_POINT ( 'NONE',  ( -6.000000000000007105, -1.607695154586655129, -111.7693375672974270 ) ) ;
#6902 = FACE_OUTER_BOUND ( 'NONE', #28362, .T. ) ;
#6903 = COLOUR_RGB ( '', 0.09019608, 0.27058824, 0.51372549) ;
#6904 = CARTESIAN_POINT ( 'NONE',  ( 160.7244614532509672, -11.41189565439133879, -3.712099293216823970 ) ) ;
#6905 = CARTESIAN_POINT ( 'NONE',  ( -3.175426480542816510, 5.499999999999865885, -119.8750000000000284 ) ) ;
#6906 = CARTESIAN_POINT ( 'NONE',  ( 0.000000000000000000, 5.999999999999977796, -166.2113248654052313 ) ) ;
#6907 = CARTESIAN_POINT ( 'NONE',  ( 114.4761751345946266, 0.8284271247463257382, 2.000000000000271783 ) ) ;
#6908 = VERTEX_POINT ( 'NONE', #15256 ) ;
#6909 = CARTESIAN_POINT ( 'NONE',  ( 20.43750000000011369, 1.097466725451739622, -2.649519052838298805 ) ) ;
#6910 = CARTESIAN_POINT ( 'NONE',  ( -5.999999999999971578, 1.607695154586715303, -122.4033121635129930 ) ) ;
#6911 = DIRECTION ( 'NONE',  ( 1.000000000000000000, 0.000000000000000000, 0.000000000000000000 ) ) ;
#6912 = VERTEX_POINT ( 'NONE', #26880 ) ;
#6913 = CARTESIAN_POINT ( 'NONE',  ( 111.3122167782374277, -0.7662911109076785410, -1.849990392679291551 ) ) ;
#6914 = CARTESIAN_POINT ( 'NONE',  ( 3.608439182435180470, -6.249999999999997335, -111.1919872981078186 ) ) ;
#6915 = FACE_BOUND ( 'NONE', #5874, .T. ) ;
#6916 = CARTESIAN_POINT ( 'NONE',  ( 140.6175748654052313, 5.500000000000012434, -2.278174593052012309 ) ) ;
#6917 = ORIENTED_EDGE ( 'NONE', *, *, #5725, .F. ) ;
#6918 = VERTEX_POINT ( 'NONE', #12655 ) ;
#6919 = CARTESIAN_POINT ( 'NONE',  ( 152.1488248654052029, -3.889087296526011706, -3.889087296526011706 ) ) ;
#6920 =( REPRESENTATION_RELATIONSHIP ('NONE','NONE', #103, #7189 ) REPRESENTATION_RELATIONSHIP_WITH_TRANSFORMATION ( #23725 )SHAPE_REPRESENTATION_RELATIONSHIP( ) );
#6921 = CARTESIAN_POINT ( 'NONE',  ( 133.5937500000000284, 6.000000000000005329, 2.485281374238585972 ) ) ;
#6922 = EDGE_CURVE ( 'NONE', #18576, #3582, #23845, .T. ) ;
#6923 = EDGE_CURVE ( 'NONE', #6626, #9180, #4759, .T. ) ;
#6924 = CARTESIAN_POINT ( 'NONE',  ( -3.608439182435052128, -6.250000000000110134, -142.9419872981078470 ) ) ;
#6925 = VECTOR ( 'NONE', #29911, 1000.000000000000000 ) ;
#6926 = CARTESIAN_POINT ( 'NONE',  ( 10.37500000000007816, 2.649519052838555933, -5.551115123125782702E-14 ) ) ;
#6927 = CARTESIAN_POINT ( 'NONE',  ( 142.4136751345948539, 0.000000000000000000, -5.500000000000005329 ) ) ;
#6928 = CARTESIAN_POINT ( 'NONE',  ( 23.43750000000010303, -1.999999999999851674, 0.8284271247462955401 ) ) ;
#6929 = DIRECTION ( 'NONE',  ( -7.147005652999508048E-36, 5.642372883946980038E-36, 1.000000000000000000 ) ) ;
#6930 = CARTESIAN_POINT ( 'NONE',  ( -5.412658773652684552, -3.125000000000099920, -61.43301270189221697 ) ) ;
#6931 = CARTESIAN_POINT ( 'NONE',  ( 135.0000273856246622, -6.966962943893147298, -8.502862253537376347 ) ) ;
#6932 = CARTESIAN_POINT ( 'NONE',  ( 143.5163997308104058, 4.999999999999989342, 2.071067811865468400 ) ) ;
#6933 = CARTESIAN_POINT ( 'NONE',  ( 0.000000000000000000, -5.999999999999991118, -124.9613248654052313 ) ) ;
#6934 = COLOUR_RGB ( '', 0.09019608, 0.27058824, 0.51372549) ;
#6935 = CARTESIAN_POINT ( 'NONE',  ( -5.999999999999919176, 1.607695154586804565, -73.48066243270262987 ) ) ;
#6936 = DIRECTION ( 'NONE',  ( -1.000000000000000000, 0.000000000000000000, 0.000000000000000000 ) ) ;
#6937 = CIRCLE ( 'NONE', #1049, 12.00000000000000178 ) ;
#6938 = DIRECTION ( 'NONE',  ( 0.000000000000000000, 1.000000000000000000, 0.000000000000000000 ) ) ;
#6939 = CARTESIAN_POINT ( 'NONE',  ( 3.464101615137757051, -5.999999999999979572, -66.91367513459479710 ) ) ;
#6940 = CARTESIAN_POINT ( 'NONE',  ( 111.5624999999997584, -2.499999999999964473, -1.035533905932689347 ) ) ;
#6941 = FACE_OUTER_BOUND ( 'NONE', #26754, .T. ) ;
#6942 = CARTESIAN_POINT ( 'NONE',  ( 115.1011751345945981, 0.8284271247463257382, -1.999999999999791278 ) ) ;
#6943 =( NAMED_UNIT ( * ) PLANE_ANGLE_UNIT ( ) SI_UNIT ( $, .RADIAN. ) );
#6944 = VERTEX_POINT ( 'NONE', #5537 ) ;
#6945 = AXIS2_PLACEMENT_3D ( 'NONE', #20896, #1832, #11236 ) ;
#6946 = CARTESIAN_POINT ( 'NONE',  ( 3.175426480543072749, 5.499999999999865885, -51.12500000000001421 ) ) ;
#6947 = CARTESIAN_POINT ( 'NONE',  ( -5.196152422706601826, 2.999999999999975131, -78.96132486540518869 ) ) ;
#6948 = CARTESIAN_POINT ( 'NONE',  ( 116.0000000000000142, 6.735557395310442023E-16, 5.500000000000000000 ) ) ;
#6949 = ORIENTED_EDGE ( 'NONE', *, *, #5471, .T. ) ;
#6950 = CARTESIAN_POINT ( 'NONE',  ( 104.6249999999999005, -1.767766952966376426, -1.767766952966320915 ) ) ;
#6951 = CARTESIAN_POINT ( 'NONE',  ( 141.4687500000000853, -2.485281374238585972, 6.000000000000005329 ) ) ;
#6952 = CARTESIAN_POINT ( 'NONE',  ( -7.216878364870328078, 0.000000000000000000, -105.6919872981078470 ) ) ;
#6953 = CARTESIAN_POINT ( 'NONE',  ( 142.6949251345948539, 5.500000000000012434, -2.278174593052012309 ) ) ;
#6954 = CARTESIAN_POINT ( 'NONE',  ( 132.2812500000000000, 2.485281374238585972, 6.000000000000005329 ) ) ;
#6955 = DIRECTION ( 'NONE',  ( -7.147005652999508048E-36, 5.642372883946980038E-36, 1.000000000000000000 ) ) ;
#6956 = MECHANICAL_DESIGN_GEOMETRIC_PRESENTATION_REPRESENTATION (  '', ( #28035 ), #24121 ) ;
#6957 = ORIENTED_EDGE ( 'NONE', *, *, #13213, .T. ) ;
#6958 = CARTESIAN_POINT ( 'NONE',  ( 6.350852961086080661, -9.614813431917819062E-14, -141.3750000000000568 ) ) ;
#6959 = EDGE_CURVE ( 'NONE', #16005, #10874, #21463, .T. ) ;
#6960 = ORIENTED_EDGE ( 'NONE', *, *, #23349, .T. ) ;
#6961 = CARTESIAN_POINT ( 'NONE',  ( -3.175426480542816510, 5.499999999999865885, -64.37500000000001421 ) ) ;
#6962 = LINE ( 'NONE', #2069, #5717 ) ;
#6963 = CARTESIAN_POINT ( 'NONE',  ( 0.000000000000000000, -5.999999999999991118, -124.0386751345948824 ) ) ;
#6964 =( BOUNDED_CURVE ( )  B_SPLINE_CURVE ( 2, ( #19556, #19700, #3092, #26442, #29189, #14805, #12519, #8150, #10187 ),
 .UNSPECIFIED., .F., .T. ) 
 B_SPLINE_CURVE_WITH_KNOTS ( ( 3, 2, 2, 2, 3 ),
 ( 0.2694444444444443754, 0.2703703703703703720, 0.2722222222222222543, 0.2740740740740740256, 0.2750000000000000222 ),
 .UNSPECIFIED. ) 
 CURVE ( )  GEOMETRIC_REPRESENTATION_ITEM ( )  RATIONAL_B_SPLINE_CURVE ( ( 0.9330127018922194093, 0.9330127018922154125, 1.000000000000000000, 0.8660254037844388186, 1.000000000000000000, 0.8660254037844388186, 1.000000000000000000, 0.9330127018922154125, 0.9330127018922194093 ) ) 
 REPRESENTATION_ITEM ( '' )  );
#6965 = ORIENTED_EDGE ( 'NONE', *, *, #4426, .T. ) ;
#6966 = CARTESIAN_POINT ( 'NONE',  ( -4.999999999999920952, -65.50000000000001421, -7.500000000000007105 ) ) ;
#6967 = CARTESIAN_POINT ( 'NONE',  ( 107.1247167782375556, -1.849990392679301543, 2.220446049250313081E-13 ) ) ;
#6968 = DIRECTION ( 'NONE',  ( 1.000000000000000000, -5.551115123125773458E-17, 0.000000000000000000 ) ) ;
#6969 = FACE_OUTER_BOUND ( 'NONE', #7371, .T. ) ;
#6970 = CARTESIAN_POINT ( 'NONE',  ( 117.4377832217621602, 1.849990392679562001, 0.7662911109079489913 ) ) ;
#6971 = CARTESIAN_POINT ( 'NONE',  ( 4.763139720814407951, -2.749999999999988454, -146.0000000000000284 ) ) ;
#6972 = CARTESIAN_POINT ( 'NONE',  ( 19.47617513459484329, 1.035533905932689347, 2.499999999999964473 ) ) ;
#6973 = CARTESIAN_POINT ( 'NONE',  ( 6.350852961086080661, -9.614813431917819062E-14, -133.8750000000000284 ) ) ;
#6974 = CARTESIAN_POINT ( 'NONE',  ( 2.775557561562891351E-14, -6.250000000000061284, -163.1830127018922383 ) ) ;
#6975 = CARTESIAN_POINT ( 'NONE',  ( 6.000000000000052403, -1.607695154586662678, -148.6533121635129930 ) ) ;
#6976 = CARTESIAN_POINT ( 'NONE',  ( 6.000000000000000888, 1.743066579297358182E-13, -90.08632486540521711 ) ) ;
#6977 = AXIS2_PLACEMENT_3D ( 'NONE', #21735, #7729, #26462 ) ;
#6978 = PRODUCT ( 'Rod base', 'Rod base', '', ( #1604 ) ) ;
#6979 = CARTESIAN_POINT ( 'NONE',  ( -2.775557561562891351E-14, -5.500000000000115463, -75.75000000000004263 ) ) ;
#6980 =( NAMED_UNIT ( * ) PLANE_ANGLE_UNIT ( ) SI_UNIT ( $, .RADIAN. ) );
#6981 = CARTESIAN_POINT ( 'NONE',  ( -4.763139720814407951, -2.750000000000016431, -65.50000000000000000 ) ) ;
#6982 = CYLINDRICAL_SURFACE ( 'NONE', #11669, 5.500000000000000000 ) ;
#6983 = CARTESIAN_POINT ( 'NONE',  ( 5.196152422706629359, -2.999999999999988898, -114.2113248654051887 ) ) ;
#6984 = ADVANCED_FACE ( 'NONE', ( #3535 ), #12966, .T. ) ;
#6985 = CARTESIAN_POINT ( 'NONE',  ( 157.8750000000000568, 0.000000000000000000, 6.000000000000005329 ) ) ;
#6986 = CARTESIAN_POINT ( 'NONE',  ( 20.00000000000004619, 2.000000000000057288, -5.551115123125782702E-14 ) ) ;
#6987 = EDGE_CURVE ( 'NONE', #13194, #15054, #10120, .T. ) ;
#6988 = CARTESIAN_POINT ( 'NONE',  ( 139.0386751345948255, -5.500000000000005329, 0.000000000000000000 ) ) ;
#6989 = CARTESIAN_POINT ( 'NONE',  ( -3.464101615137757051, -5.999999999999979572, -98.66367513459481131 ) ) ;
#6990 = CARTESIAN_POINT ( 'NONE',  ( 116.3122167782374845, -0.7662911109077388261, -1.849990392679351725 ) ) ;
#6991 = CARTESIAN_POINT ( 'NONE',  ( 3.464101615137757051, -5.999999999999979572, -97.83632486540517448 ) ) ;
#6992 = ORIENTED_EDGE ( 'NONE', *, *, #3538, .F. ) ;
#6993 = CARTESIAN_POINT ( 'NONE',  ( 148.3125000000000284, 4.242640687119298093, -4.242640687119298093 ) ) ;
#6994 = CARTESIAN_POINT ( 'NONE',  ( 10.00000000000012079, -0.6095397824213422133, -2.424553825687569830 ) ) ;
#6995 = CARTESIAN_POINT ( 'NONE',  ( 113.1252832217622029, -1.110223024625156540E-13, -1.849990392679523588 ) ) ;
#6996 = CARTESIAN_POINT ( 'NONE',  ( 11.96132486540524198, 1.110223024625156540E-13, 2.499999999999835687 ) ) ;
#6997 = EDGE_LOOP ( 'NONE', ( #22027, #8571, #1181, #20265 ) ) ;
#6998 = ORIENTED_EDGE ( 'NONE', *, *, #10508, .F. ) ;
#6999 = EDGE_CURVE ( 'NONE', #5282, #24822, #10487, .T. ) ;
#7000 = ORIENTED_EDGE ( 'NONE', *, *, #19257, .F. ) ;
#7001 = CARTESIAN_POINT ( 'NONE',  ( 6.350852961086080661, -9.614813431917819062E-14, -90.37500000000000000 ) ) ;
#7002 = CARTESIAN_POINT ( 'NONE',  ( 7.216878364870455975, -6.409875621278545621E-14, -108.8080127018922667 ) ) ;
#7003 = ORIENTED_EDGE ( 'NONE', *, *, #28612, .F. ) ;
#7004 = CARTESIAN_POINT ( 'NONE',  ( 5.687368478358042267, 9.417270245429904207, -26.95189157943837444 ) ) ;
#7005 = CARTESIAN_POINT ( 'NONE',  ( 154.9538997308104058, -2.071067811865468400, -4.999999999999989342 ) ) ;
#7006 = CARTESIAN_POINT ( 'NONE',  ( 2.775557561562891351E-14, -11.00000000000001066, -31.00000000000002842 ) ) ;
#7007 = VERTEX_POINT ( 'NONE', #5390 ) ;
#7008 = CARTESIAN_POINT ( 'NONE',  ( 6.000000000000000888, 1.607695154586715303, -93.59668783648702117 ) ) ;
#7009 =( NAMED_UNIT ( * ) SI_UNIT ( $, .STERADIAN. ) SOLID_ANGLE_UNIT ( ) );
#7010 = MECHANICAL_DESIGN_GEOMETRIC_PRESENTATION_REPRESENTATION (  '', ( #26143 ), #14873 ) ;
#7011 = CARTESIAN_POINT ( 'NONE',  ( 4.763139720814407951, -2.749999999999988454, -174.5000000000000000 ) ) ;
#7012 = CARTESIAN_POINT ( 'NONE',  ( -4.999999999999886313, -10.50000000000000888, -8.000000000000007105 ) ) ;
#7013 = CARTESIAN_POINT ( 'NONE',  ( 4.763139720814407951, -2.749999999999988454, -152.0000000000000284 ) ) ;
#7014 = CARTESIAN_POINT ( 'NONE',  ( 111.6249999999998153, -1.767766952966376426, -1.767766952966431937 ) ) ;
#7015 =( BOUNDED_CURVE ( )  B_SPLINE_CURVE ( 2, ( #1243, #19703, #19559, #10191, #28894, #26733, #22161, #7859, #22468 ),
 .UNSPECIFIED., .F., .F. ) 
 B_SPLINE_CURVE_WITH_KNOTS ( ( 3, 2, 2, 2, 3 ),
 ( 0.3472222222222222099, 0.3481481481481481510, 0.3499999999999999778, 0.3518518518518518601, 0.3527777777777778012 ),
 .UNSPECIFIED. ) 
 CURVE ( )  GEOMETRIC_REPRESENTATION_ITEM ( )  RATIONAL_B_SPLINE_CURVE ( ( 0.9330127018922194093, 0.9330127018922194093, 1.000000000000000000, 0.8660254037844388186, 1.000000000000000000, 0.8660254037844388186, 1.000000000000000000, 0.9330127018922174109, 0.9330127018922194093 ) ) 
 REPRESENTATION_ITEM ( '' )  );
#7016 = CARTESIAN_POINT ( 'NONE',  ( -4.763139720814407951, 2.749999999999946709, -101.7500000000000000 ) ) ;
#7017 = DIRECTION ( 'NONE',  ( 1.000000000000000000, -5.551115123125773458E-17, -1.260129944081490338E-35 ) ) ;
#7018 = CARTESIAN_POINT ( 'NONE',  ( 6.000000000000000888, -3.330669073875464691E-16, -7.560779664488942560E-35 ) ) ;
#7019 = CARTESIAN_POINT ( 'NONE',  ( 4.763139720814407951, 2.750000000000002665, -90.25000000000005684 ) ) ;
#7020 =( GEOMETRIC_REPRESENTATION_CONTEXT ( 3 ) GLOBAL_UNCERTAINTY_ASSIGNED_CONTEXT ( ( #21415 ) ) GLOBAL_UNIT_ASSIGNED_CONTEXT ( ( #21905, #10083, #26628 ) ) REPRESENTATION_CONTEXT ( 'NONE', 'WORKASPACE' ) );
#7021 = CARTESIAN_POINT ( 'NONE',  ( 135.0581880922677556, -7.766452621457742289, 8.294963418928750443 ) ) ;
#7022 = VERTEX_POINT ( 'NONE', #3382 ) ;
#7023 = CARTESIAN_POINT ( 'NONE',  ( 10.50000000000014744, 1.873492889145123019, -1.873492889144956486 ) ) ;
#7024 = CARTESIAN_POINT ( 'NONE',  ( 111.5624999999997584, -2.499999999999964473, -1.035533905932689347 ) ) ;
#7025 = EDGE_CURVE ( 'NONE', #11375, #18429, #8691, .T. ) ;
#7026 = CARTESIAN_POINT ( 'NONE',  ( 10.00000000000002309, -5.999999999999914735, 1.056932319443149026E-13 ) ) ;
#7027 = CARTESIAN_POINT ( 'NONE',  ( 107.8752832217621602, -1.849990392679329299, 3.330669073875469621E-13 ) ) ;
#7028 = CARTESIAN_POINT ( 'NONE',  ( 23.85117513459495697, -2.499999999999964473, -1.035533905932869425 ) ) ;
#7029 = VERTEX_POINT ( 'NONE', #17261 ) ;
#7030 = CYLINDRICAL_SURFACE ( 'NONE', #5277, 2.000000000000003109 ) ;
#7031 = DIRECTION ( 'NONE',  ( 1.000000000000000000, -5.551115123125773458E-17, -1.260129944081490338E-35 ) ) ;
#7032 = CARTESIAN_POINT ( 'NONE',  ( 105.3122167782374277, -0.7662911109076785410, -1.849990392679231599 ) ) ;
#7033 = ORIENTED_EDGE ( 'NONE', *, *, #13180, .F. ) ;
#7034 = EDGE_CURVE ( 'NONE', #278, #18461, #19837, .T. ) ;
#7035 = CARTESIAN_POINT ( 'NONE',  ( 3.464101615137757051, -5.999999999999979572, -141.3363248654052029 ) ) ;
#7036 = VECTOR ( 'NONE', #2124, 1000.000000000000000 ) ;
#7037 = EDGE_CURVE ( 'NONE', #11685, #4790, #13652, .T. ) ;
#7038 = MECHANICAL_DESIGN_GEOMETRIC_PRESENTATION_REPRESENTATION (  '', ( #7531 ), #4082 ) ;
#7039 = EDGE_LOOP ( 'NONE', ( #21815, #7936, #29112, #12594 ) ) ;
#7040 = CARTESIAN_POINT ( 'NONE',  ( 153.3750000000000284, 0.000000000000000000, 6.000000000000005329 ) ) ;
#7041 = ORIENTED_EDGE ( 'NONE', *, *, #13078, .T. ) ;
#7042 = CARTESIAN_POINT ( 'NONE',  ( -4.763139720814407951, -2.750000000000016431, -110.5000000000000426 ) ) ;
#7043 = CARTESIAN_POINT ( 'NONE',  ( 21.93750000000006395, -2.649519052838178457, -1.097466725451439196 ) ) ;
#7044 = AXIS2_PLACEMENT_3D ( 'NONE', #16090, #8516, #27539 ) ;
#7045 = CARTESIAN_POINT ( 'NONE',  ( -5.412658773652739619, 3.124999999999975131, -133.6830127018922667 ) ) ;
#7046 = VERTEX_POINT ( 'NONE', #10254 ) ;
#7047 = CARTESIAN_POINT ( 'NONE',  ( 141.0000000000000284, -11.31370849898477537, -4.000000000000003553 ) ) ;
#7048 = CARTESIAN_POINT ( 'NONE',  ( -3.608439182435115633, 6.249999999999965361, -171.9419872981078470 ) ) ;
#7049 = CARTESIAN_POINT ( 'NONE',  ( 107.2499999999999147, 0.000000000000000000, 2.499999999999946709 ) ) ;
#7050 = VERTEX_POINT ( 'NONE', #24502 ) ;
#7051 = CARTESIAN_POINT ( 'NONE',  ( -0.07773410149728489371, -14.92045216308241073, -8.102832156385545659 ) ) ;
#7052 = CARTESIAN_POINT ( 'NONE',  ( 5.061300234018967004, 3.091548682352961208, -180.0000000000001421 ) ) ;
#7053 = CARTESIAN_POINT ( 'NONE',  ( 0.000000000000000000, 5.499999999999991118, -181.5000000000000000 ) ) ;
#7054 = CARTESIAN_POINT ( 'NONE',  ( 109.9377832217622029, -1.849990392679472073, -0.7662911109076485650 ) ) ;
#7055 = CARTESIAN_POINT ( 'NONE',  ( -7.216878364870328078, 0.000000000000000000, -180.0580127018922667 ) ) ;
#7056 = CARTESIAN_POINT ( 'NONE',  ( -3.464101615137757051, -5.999999999999979572, -111.5863248654051887 ) ) ;
#7057 = CARTESIAN_POINT ( 'NONE',  ( -5.999999999999971578, 1.607695154586715303, -122.9806624327025872 ) ) ;
#7058 =( BOUNDED_CURVE ( )  B_SPLINE_CURVE ( 2, ( #25759, #253, #7606, #2854, #12418, #12273, #28792, #9636, #550 ),
 .UNSPECIFIED., .F., .T. ) 
 B_SPLINE_CURVE_WITH_KNOTS ( ( 3, 2, 2, 2, 3 ),
 ( 0.4124999999999989786, 0.4187499999999991784, 0.4249999999999994893, 0.4312499999999997446, 0.4374999999999999445 ),
 .UNSPECIFIED. ) 
 CURVE ( )  GEOMETRIC_REPRESENTATION_ITEM ( )  RATIONAL_B_SPLINE_CURVE ( ( 1.000000000000012212, 0.9238795325112745260, 1.000000000000000000, 0.9238795325112867385, 1.000000000000000000, 0.9238795325112867385, 1.000000000000000000, 0.9238795325112874046, 0.9999999999999993339 ) ) 
 REPRESENTATION_ITEM ( '' )  );
#7059 = CARTESIAN_POINT ( 'NONE',  ( -3.175426480542816510, -5.500000000000057732, -123.8749999999999716 ) ) ;
#7060 = CARTESIAN_POINT ( 'NONE',  ( -9.999999999999772626, -90.00000000000001421, 4.000000000000003553 ) ) ;
#7061 = CARTESIAN_POINT ( 'NONE',  ( 154.0238248654052313, 3.889087296526011706, -3.889087296526011706 ) ) ;
#7062 = ORIENTED_EDGE ( 'NONE', *, *, #11589, .F. ) ;
#7063 = CARTESIAN_POINT ( 'NONE',  ( 20.12500000000000355, -2.649519052838167354, -1.665334536937734811E-13 ) ) ;
#7064 = FACE_OUTER_BOUND ( 'NONE', #20449, .T. ) ;
#7065 = ADVANCED_FACE ( 'NONE', ( #1464 ), #13037, .F. ) ;
#7066 = CARTESIAN_POINT ( 'NONE',  ( 135.5000000000000000, -54.99999999999993605, 8.000000000000007105 ) ) ;
#7067 = CARTESIAN_POINT ( 'NONE',  ( 115.7113248654050466, 2.000000000000112799, 0.000000000000000000 ) ) ;
#7068 = VERTEX_POINT ( 'NONE', #17476 ) ;
#7069 = CARTESIAN_POINT ( 'NONE',  ( 111.4372167782375271, 0.7662911109078888172, -1.849990392679231599 ) ) ;
#7070 = CARTESIAN_POINT ( 'NONE',  ( 10.00000000000014744, 1.110223024625156540E-13, -5.551115123125782702E-14 ) ) ;
#7071 = CARTESIAN_POINT ( 'NONE',  ( 5.412658773652712085, -3.125000000000086153, -111.0669872981078186 ) ) ;
#7072 = DIRECTION ( 'NONE',  ( -1.000000000000000000, 0.000000000000000000, 0.000000000000000000 ) ) ;
#7073 = ORIENTED_EDGE ( 'NONE', *, *, #22255, .F. ) ;
#7074 = ADVANCED_FACE ( 'NONE', ( #3765 ), #30114, .T. ) ;
#7075 = CARTESIAN_POINT ( 'NONE',  ( 140.8050748654052029, 5.500000000000012434, 2.278174593052012309 ) ) ;
#7076 = ORIENTED_EDGE ( 'NONE', *, *, #6618, .T. ) ;
#7077 = ORIENTED_EDGE ( 'NONE', *, *, #17946, .T. ) ;
#7078 = CARTESIAN_POINT ( 'NONE',  ( 6.000000000000000888, -1.607695154586752384, -141.7306624327026157 ) ) ;
#7079 = CARTESIAN_POINT ( 'NONE',  ( 138.8437500000000568, -6.000000000000005329, -2.485281374238555774 ) ) ;
#7080 = CARTESIAN_POINT ( 'NONE',  ( -3.608439182435115633, 6.249999999999965361, -137.4419872981078186 ) ) ;
#7081 = FILL_AREA_STYLE_COLOUR ( '', #26960 ) ;
#7082 = CARTESIAN_POINT ( 'NONE',  ( 12.81250000000010303, -2.649519052838178457, 1.097466725451499370 ) ) ;
#7083 = CARTESIAN_POINT ( 'NONE',  ( 18.96132486540530593, 1.110223024625156540E-13, 2.499999999999724665 ) ) ;
#7084 = CARTESIAN_POINT ( 'NONE',  ( 17.81250000000015277, 0.8284271247463557142, -2.000000000000091926 ) ) ;
#7085 = CARTESIAN_POINT ( 'NONE',  ( -3.464101615137757051, -5.999999999999979572, -171.5863248654051745 ) ) ;
#7086 = CARTESIAN_POINT ( 'NONE',  ( 5.412658773652712085, -3.125000000000086153, -59.43301270189227381 ) ) ;
#7087 = CARTESIAN_POINT ( 'NONE',  ( 145.2038997308104342, 2.071067811865468400, 4.999999999999989342 ) ) ;
#7088 = CARTESIAN_POINT ( 'NONE',  ( -5.999999999999956479, -1.607695154586745057, -125.2693375672974128 ) ) ;
#7089 = CYLINDRICAL_SURFACE ( 'NONE', #22656, 6.000000000000000888 ) ;
#7090 = CARTESIAN_POINT ( 'NONE',  ( 3.464101615137757051, -5.999999999999979572, -146.4136751345947971 ) ) ;
#7091 = CARTESIAN_POINT ( 'NONE',  ( 0.000000000000000000, 0.000000000000000000, 0.000000000000000000 ) ) ;
#7092 = CARTESIAN_POINT ( 'NONE',  ( 112.1874999999998153, 1.035533905932719101, 2.500000000000205169 ) ) ;
#7093 = SURFACE_SIDE_STYLE ('',( #28125 ) ) ;
#7094 = CARTESIAN_POINT ( 'NONE',  ( 156.0863248654052597, 0.000000000000000000, 5.500000000000005329 ) ) ;
#7095 = EDGE_LOOP ( 'NONE', ( #11410, #16379, #22344, #9621 ) ) ;
#7096 = EDGE_CURVE ( 'NONE', #25843, #19300, #18753, .T. ) ;
#7097 = CARTESIAN_POINT ( 'NONE',  ( -4.763139720814407951, 2.749999999999946709, -53.75000000000002132 ) ) ;
#7098 = CARTESIAN_POINT ( 'NONE',  ( -3.464101615137725076, 5.999999999999979572, -79.08632486540516027 ) ) ;
#7099 = EDGE_CURVE ( 'NONE', #4040, #21072, #17043, .T. ) ;
#7100 = CARTESIAN_POINT ( 'NONE',  ( 4.000000000000006217, -2.220446049250313081E-16, -200.0000000000000000 ) ) ;
#7101 = ORIENTED_EDGE ( 'NONE', *, *, #23170, .T. ) ;
#7102 = CARTESIAN_POINT ( 'NONE',  ( 106.5624999999998295, -2.499999999999874767, -1.035533905932629173 ) ) ;
#7103 = CARTESIAN_POINT ( 'NONE',  ( 140.6250000000000284, 0.000000000000000000, -6.000000000000005329 ) ) ;
#7104 = CARTESIAN_POINT ( 'NONE',  ( 2.775557561562891351E-14, 6.250000000000033751, -101.5669872981078186 ) ) ;
#7105 =( GEOMETRIC_REPRESENTATION_CONTEXT ( 3 ) GLOBAL_UNCERTAINTY_ASSIGNED_CONTEXT ( ( #20074 ) ) GLOBAL_UNIT_ASSIGNED_CONTEXT ( ( #1701, #27034, #24744 ) ) REPRESENTATION_CONTEXT ( 'NONE', 'WORKASPACE' ) );
#7106 = CARTESIAN_POINT ( 'NONE',  ( 112.2113248654051176, -1.999999999999946265, 0.000000000000000000 ) ) ;
#7107 = CARTESIAN_POINT ( 'NONE',  ( 159.6413997308104058, 2.071067811865468400, -4.999999999999989342 ) ) ;
#7108 = CARTESIAN_POINT ( 'NONE',  ( -4.763139720814407951, 2.749999999999946709, -140.7500000000000284 ) ) ;
#7109 = ORIENTED_EDGE ( 'NONE', *, *, #12342, .F. ) ;
#7110 = CARTESIAN_POINT ( 'NONE',  ( 0.000000000000000000, 0.000000000000000000, 0.000000000000000000 ) ) ;
#7111 = VECTOR ( 'NONE', #4218, 1000.000000000000000 ) ;
#7112 = CARTESIAN_POINT ( 'NONE',  ( 6.350852961086080661, -9.614813431917819062E-14, -64.87500000000002842 ) ) ;
#7113 = CARTESIAN_POINT ( 'NONE',  ( 6.000000000000000888, 1.743066579297358182E-13, -73.58632486540520290 ) ) ;
#7114 = LINE ( 'NONE', #14660, #16210 ) ;
#7115 = CARTESIAN_POINT ( 'NONE',  ( -7.216878364870328078, 0.000000000000000000, -85.55801270189222407 ) ) ;
#7116 = CARTESIAN_POINT ( 'NONE',  ( -5.999999999999963585, -1.487416814333745711E-14, -101.3363248654052171 ) ) ;
#7117 = CARTESIAN_POINT ( 'NONE',  ( -5.196152422706573404, -3.000000000000002665, -113.7886751345948397 ) ) ;
#7118 = CARTESIAN_POINT ( 'NONE',  ( 107.1872167782375840, -1.849990392679441875, -0.7662911109076485650 ) ) ;
#7119 = DIRECTION ( 'NONE',  ( -7.147005652999508048E-36, 5.642372883946980038E-36, 1.000000000000000000 ) ) ;
#7120 = CARTESIAN_POINT ( 'NONE',  ( 1.000000000000000888, 0.000000000000000000, 0.000000000000000000 ) ) ;
#7121 = CARTESIAN_POINT ( 'NONE',  ( 118.2502832217622739, 1.308140751793640533, -1.308140751793418488 ) ) ;
#7122 = CARTESIAN_POINT ( 'NONE',  ( -4.763139720814407951, 2.749999999999946709, -149.7500000000000568 ) ) ;
#7123 = CARTESIAN_POINT ( 'NONE',  ( -2.775557561562891351E-14, 6.000000000000088818, 1.110223024625156540E-13 ) ) ;
#7124 = CIRCLE ( 'NONE', #2688, 5.000000000000004441 ) ;
#7125 = CARTESIAN_POINT ( 'NONE',  ( -5.412658773652739619, 3.124999999999975131, -160.6830127018922383 ) ) ;
#7126 = CARTESIAN_POINT ( 'NONE',  ( -3.464101615137757051, -5.999999999999979572, -149.0863248654052313 ) ) ;
#7127 = CARTESIAN_POINT ( 'NONE',  ( 105.2738248654049329, -1.999999999999941602, -0.8284271247460553989 ) ) ;
#7128 = CARTESIAN_POINT ( 'NONE',  ( 4.763139720814407951, 2.750000000000002665, -82.74999999999998579 ) ) ;
#7129 = DIRECTION ( 'NONE',  ( 0.000000000000000000, -5.551115123125767911E-17, 1.000000000000000000 ) ) ;
#7130 = CARTESIAN_POINT ( 'NONE',  ( 3.175426480543072749, -5.500000000000105693, -62.12500000000000711 ) ) ;
#7131 = ADVANCED_FACE ( 'NONE', ( #4880 ), #7177, .T. ) ;
#7132 = PRESENTATION_STYLE_ASSIGNMENT (( #28162 ) ) ;
#7133 = CARTESIAN_POINT ( 'NONE',  ( 143.8273502691896510, -5.000000000000004441, 0.000000000000000000 ) ) ;
#7134 = CARTESIAN_POINT ( 'NONE',  ( 160.5863248654052597, 0.000000000000000000, 5.500000000000005329 ) ) ;
#7135 = CARTESIAN_POINT ( 'NONE',  ( -5.999999999999963585, 8.134310703387671600E-14, -144.8363248654052029 ) ) ;
#7136 = CARTESIAN_POINT ( 'NONE',  ( 156.4687500000000568, -2.485281374238585972, 6.000000000000005329 ) ) ;
#7137 = FILL_AREA_STYLE_COLOUR ( '', #28092 ) ;
#7138 = DIRECTION ( 'NONE',  ( 1.000000000000000000, -5.551115123125773458E-17, -1.260129944081490338E-35 ) ) ;
#7139 = CARTESIAN_POINT ( 'NONE',  ( 119.2497167782374987, -1.308140751793557266, -1.308140751793640533 ) ) ;
#7140 = CARTESIAN_POINT ( 'NONE',  ( 5.196152422706629359, 3.000000000000002665, -170.0386751345947971 ) ) ;
#7141 =( BOUNDED_CURVE ( )  B_SPLINE_CURVE ( 2, ( #222, #11796, #21137, #7299, #4972, #74, #14406, #9459, #18844 ),
 .UNSPECIFIED., .F., .F. ) 
 B_SPLINE_CURVE_WITH_KNOTS ( ( 3, 2, 2, 2, 3 ),
 ( 0.02499999999999991118, 0.02592592592592590783, 0.02777777777777779011, 0.02962962962962967239, 0.03055555555555555802 ),
 .UNSPECIFIED. ) 
 CURVE ( )  GEOMETRIC_REPRESENTATION_ITEM ( )  RATIONAL_B_SPLINE_CURVE ( ( 0.9330127018922194093, 0.9330127018922154125, 1.000000000000000000, 0.8660254037844388186, 1.000000000000000000, 0.8660254037844388186, 1.000000000000000000, 0.9330127018922194093, 0.9330127018922194093 ) ) 
 REPRESENTATION_ITEM ( '' )  );
#7142 = ORIENTED_EDGE ( 'NONE', *, *, #20882, .T. ) ;
#7143 = CARTESIAN_POINT ( 'NONE',  ( 147.4687500000000853, -2.485281374238585972, 6.000000000000005329 ) ) ;
#7144 = DIRECTION ( 'NONE',  ( -0.000000000000000000, -0.000000000000000000, -1.000000000000000000 ) ) ;
#7145 = CARTESIAN_POINT ( 'NONE',  ( 115.3127832217621886, 1.849990392679562001, -0.7662911109076485650 ) ) ;
#7146 = DIRECTION ( 'NONE',  ( 0.000000000000000000, 0.000000000000000000, -1.000000000000000000 ) ) ;
#7147 = ORIENTED_EDGE ( 'NONE', *, *, #10130, .T. ) ;
#7148 =( BOUNDED_CURVE ( )  B_SPLINE_CURVE ( 2, ( #21858, #12665, #22467, #19558, #26732, #28893, #7858, #17270, #22002 ),
 .UNSPECIFIED., .F., .T. ) 
 B_SPLINE_CURVE_WITH_KNOTS ( ( 3, 2, 2, 2, 3 ),
 ( 0.8305555555555556024, 0.8314814814814814881, 0.8333333333333333703, 0.8351851851851851416, 0.8361111111111110272 ),
 .UNSPECIFIED. ) 
 CURVE ( )  GEOMETRIC_REPRESENTATION_ITEM ( )  RATIONAL_B_SPLINE_CURVE ( ( 0.9330127018922194093, 0.9330127018922234061, 1.000000000000000000, 0.8660254037844388186, 1.000000000000000000, 0.8660254037844388186, 1.000000000000000000, 0.9330127018922234061, 0.9330127018922194093 ) ) 
 REPRESENTATION_ITEM ( '' )  );
#7149 = VECTOR ( 'NONE', #20855, 1000.000000000000000 ) ;
#7150 = CARTESIAN_POINT ( 'NONE',  ( 19.81250000000009237, 0.8284271247463557142, -2.000000000000091926 ) ) ;
#7151 = CARTESIAN_POINT ( 'NONE',  ( -5.412658773652739619, 3.124999999999975131, -152.3169872981078186 ) ) ;
#7152 = ORIENTED_EDGE ( 'NONE', *, *, #5521, .F. ) ;
#7153 = CARTESIAN_POINT ( 'NONE',  ( -2.775557561562891351E-14, -5.500000000000115463, -89.25000000000005684 ) ) ;
#7154 = VERTEX_POINT ( 'NONE', #282 ) ;
#7155 = FILL_AREA_STYLE_COLOUR ( '', #28437 ) ;
#7156 = CARTESIAN_POINT ( 'NONE',  ( 158.9851497308104058, -3.535533905932725318, 3.535533905932725318 ) ) ;
#7157 = EDGE_CURVE ( 'NONE', #18709, #750, #10737, .T. ) ;
#7158 = CARTESIAN_POINT ( 'NONE',  ( 0.000000000000000000, 5.499999999999991118, -166.4999999999999716 ) ) ;
#7159 = CARTESIAN_POINT ( 'NONE',  ( 159.3675748654052029, -5.500000000000012434, 2.278174593052012309 ) ) ;
#7160 = DIRECTION ( 'NONE',  ( -0.000000000000000000, 1.000000000000000000, -0.000000000000000000 ) ) ;
#7161 = CARTESIAN_POINT ( 'NONE',  ( 0.000000000000000000, 0.000000000000000000, 0.000000000000000000 ) ) ;
#7162 =( LENGTH_UNIT ( ) NAMED_UNIT ( * ) SI_UNIT ( .MILLI., .METRE. ) );
#7163 = CARTESIAN_POINT ( 'NONE',  ( 3.175426480543072749, -5.500000000000105693, -170.1250000000000000 ) ) ;
#7164 = CARTESIAN_POINT ( 'NONE',  ( 23.16367513459499605, 1.767766952966598470, -1.767766952966542959 ) ) ;
#7165 = CARTESIAN_POINT ( 'NONE',  ( 4.763139720814407951, -2.749999999999988454, -153.5000000000000284 ) ) ;
#7166 = CARTESIAN_POINT ( 'NONE',  ( 110.5624999999998295, -2.499999999999994671, -1.035533905932568777 ) ) ;
#7167 = CARTESIAN_POINT ( 'NONE',  ( 6.350852961086080661, -9.614813431917819062E-14, -103.8750000000000142 ) ) ;
#7168 = CARTESIAN_POINT ( 'NONE',  ( 21.27382486540515316, -2.499999999999904521, -1.035533905932809473 ) ) ;
#7169 = CARTESIAN_POINT ( 'NONE',  ( 6.000000000000000888, -1.859271017917181981E-14, -84.66367513459482552 ) ) ;
#7171 = CARTESIAN_POINT ( 'NONE',  ( 6.350852961086080661, -9.614813431917819062E-14, -88.87500000000000000 ) ) ;
#7170 = CARTESIAN_POINT ( 'NONE',  ( 3.175426480543072749, 5.499999999999865885, -157.6250000000000000 ) ) ;
#7172 = EDGE_CURVE ( 'NONE', #12287, #16041, #18573, .T. ) ;
#7173 = CARTESIAN_POINT ( 'NONE',  ( 157.9836002691896226, 4.999999999999989342, -2.071067811865468400 ) ) ;
#7174 = CARTESIAN_POINT ( 'NONE',  ( -5.196152422706573404, -3.000000000000002665, -136.2886751345947971 ) ) ;
#7175 = ORIENTED_EDGE ( 'NONE', *, *, #399, .T. ) ;
#7176 = CARTESIAN_POINT ( 'NONE',  ( 23.06250000000011013, 2.000000000000151879, 0.8284271247462354770 ) ) ;
#7177 = TOROIDAL_SURFACE ( 'NONE', #27741, 11.00000000000000355, 1.000000000000000000 ) ;
#7178 = UNCERTAINTY_MEASURE_WITH_UNIT (LENGTH_MEASURE( 1.000000000000000082E-05 ), #3707, 'distance_accuracy_value', 'NONE');
#7179 = CARTESIAN_POINT ( 'NONE',  ( 112.3124999999997726, -1.035533905932598975, 2.500000000000265121 ) ) ;
#7180 = CARTESIAN_POINT ( 'NONE',  ( 139.5000000000000284, -54.99999999999990763, -8.000000000000007105 ) ) ;
#7181 = CARTESIAN_POINT ( 'NONE',  ( 108.5627832217621886, 0.7662911109077987781, 1.849990392679652151 ) ) ;
#7182 = VECTOR ( 'NONE', #28151, 1000.000000000000000 ) ;
#7183 = PRESENTATION_LAYER_ASSIGNMENT (  '', '', ( #8651 ) ) ;
#7184 = ORIENTED_EDGE ( 'NONE', *, *, #23390, .T. ) ;
#7185 = DIRECTION ( 'NONE',  ( -7.147005652999508048E-36, 5.642372883946980038E-36, 1.000000000000000000 ) ) ;
#7186 = CYLINDRICAL_SURFACE ( 'NONE', #23612, 2.499999999999999112 ) ;
#7187 = ORIENTED_EDGE ( 'NONE', *, *, #14160, .T. ) ;
#7188 = CARTESIAN_POINT ( 'NONE',  ( 6.000000000000052403, -1.607695154586662678, -141.1533121635129646 ) ) ;
#7189 = SHAPE_REPRESENTATION ( 'Rod base', ( #18805 ), #12447 ) ;
#7190 = ORIENTED_EDGE ( 'NONE', *, *, #16445, .F. ) ;
#7191 = CARTESIAN_POINT ( 'NONE',  ( 149.6250000000000284, 0.000000000000000000, -6.000000000000005329 ) ) ;
#7192 = VERTEX_POINT ( 'NONE', #24515 ) ;
#7193 = CARTESIAN_POINT ( 'NONE',  ( 4.763139720814407951, -2.749999999999988454, -112.9999999999999858 ) ) ;
#7194 = CARTESIAN_POINT ( 'NONE',  ( 23.87500000000017408, -2.649519052838111843, 0.000000000000000000 ) ) ;
#7195 = CARTESIAN_POINT ( 'NONE',  ( 3.608439182435180470, -6.249999999999997335, -128.5580127018922383 ) ) ;
#7196 = ORIENTED_EDGE ( 'NONE', *, *, #18260, .F. ) ;
#7197 = CARTESIAN_POINT ( 'NONE',  ( 151.5863248654052313, 0.000000000000000000, 5.500000000000005329 ) ) ;
#7198 = CARTESIAN_POINT ( 'NONE',  ( -7.216878364870328078, 0.000000000000000000, -167.1919872981078186 ) ) ;
#7199 = CARTESIAN_POINT ( 'NONE',  ( 108.2499999999998863, 5.551115123125782702E-14, 2.499999999999946709 ) ) ;
#7200 = CARTESIAN_POINT ( 'NONE',  ( -2.081668171172168020E-16, -5.204170427930420051E-17, 2.499999999999999112 ) ) ;
#7201 = EDGE_CURVE ( 'NONE', #22266, #1192, #26519, .T. ) ;
#7202 =( BOUNDED_CURVE ( )  B_SPLINE_CURVE ( 2, ( #29164, #29484, #1379, #21980, #10623, #20136, #19972, #6146, #7983 ),
 .UNSPECIFIED., .F., .F. ) 
 B_SPLINE_CURVE_WITH_KNOTS ( ( 3, 2, 2, 2, 3 ),
 ( 0.8694444444444443532, 0.8703703703703703498, 0.8722222222222222321, 0.8740740740740741144, 0.8750000000000000000 ),
 .UNSPECIFIED. ) 
 CURVE ( )  GEOMETRIC_REPRESENTATION_ITEM ( )  RATIONAL_B_SPLINE_CURVE ( ( 0.9330127018922194093, 0.9330127018922154125, 1.000000000000000000, 0.8660254037844388186, 1.000000000000000000, 0.8660254037844388186, 1.000000000000000000, 0.9330127018922194093, 0.9330127018922194093 ) ) 
 REPRESENTATION_ITEM ( '' )  );
#7203 = CARTESIAN_POINT ( 'NONE',  ( 109.4761751345945839, 0.8284271247462654530, 2.000000000000271783 ) ) ;
#7204 = FACE_OUTER_BOUND ( 'NONE', #22588, .T. ) ;
#7205 = CARTESIAN_POINT ( 'NONE',  ( -3.175426480542816510, 5.499999999999865885, -181.3750000000000000 ) ) ;
#7206 = CARTESIAN_POINT ( 'NONE',  ( 107.2502832217623450, 1.308140751793640533, -1.308140751793640533 ) ) ;
#7207 = CARTESIAN_POINT ( 'NONE',  ( 2.775557561562891351E-14, -6.250000000000061284, -176.6830127018922383 ) ) ;
#7208 = CARTESIAN_POINT ( 'NONE',  ( 119.6011751345946692, -0.8284271247462354770, 2.000000000000212275 ) ) ;
#7209 = FILL_AREA_STYLE ('',( #25941 ) ) ;
#7210 = EDGE_CURVE ( 'NONE', #21073, #3256, #25988, .T. ) ;
#7211 = UNCERTAINTY_MEASURE_WITH_UNIT (LENGTH_MEASURE( 1.000000000000000082E-05 ), #22543, 'distance_accuracy_value', 'NONE');
#7212 = CARTESIAN_POINT ( 'NONE',  ( 0.000000000000000000, 5.499999999999991118, -110.9999999999999858 ) ) ;
#7213 = CARTESIAN_POINT ( 'NONE',  ( 159.0000000000000284, -59.99999999999980105, -4.000000000000003553 ) ) ;
#7214 = CARTESIAN_POINT ( 'NONE',  ( 114.6011751345946692, -0.8284271247461453269, 2.000000000000271783 ) ) ;
#7215 = EDGE_LOOP ( 'NONE', ( #17748, #26509, #21257, #29756 ) ) ;
#7216 = CARTESIAN_POINT ( 'NONE',  ( 20.31250000000006040, -1.097466725451379244, -2.649519052838419153 ) ) ;
#7217 = CARTESIAN_POINT ( 'NONE',  ( 1.000000000000000888, -16.43939393939395188, 5.999693900976774685 ) ) ;
#7218 = CARTESIAN_POINT ( 'NONE',  ( 0.000000000000000000, 0.000000000000000000, 0.000000000000000000 ) ) ;
#7219 = CARTESIAN_POINT ( 'NONE',  ( 0.9564710672350417164, -15.26172842777273964, 8.566785667046460162 ) ) ;
#7220 = VECTOR ( 'NONE', #23593, 1000.000000000000000 ) ;
#7221 = VECTOR ( 'NONE', #28539, 1000.000000000000000 ) ;
#7222 = EDGE_LOOP ( 'NONE', ( #27147, #27902, #10951, #791 ) ) ;
#7223 = MECHANICAL_DESIGN_GEOMETRIC_PRESENTATION_REPRESENTATION (  '', ( #17548 ), #11166 ) ;
#7224 = SURFACE_STYLE_USAGE ( .BOTH. , #12177 ) ;
#7225 = DIRECTION ( 'NONE',  ( 1.000000000000000000, -0.000000000000000000, -0.000000000000000000 ) ) ;
#7226 = CARTESIAN_POINT ( 'NONE',  ( 110.3747167782375271, -5.551115123125782702E-14, -1.849990392679523588 ) ) ;
#7227 = DIRECTION ( 'NONE',  ( 1.000000000000000000, -5.551115123125773458E-17, -1.260129944081490338E-35 ) ) ;
#7228 = CYLINDRICAL_SURFACE ( 'NONE', #2709, 6.000000000000000888 ) ;
#7229 = CARTESIAN_POINT ( 'NONE',  ( 6.000000000000000888, -3.330669073875464691E-16, -7.560779664488942560E-35 ) ) ;
#7230 = AXIS2_PLACEMENT_3D ( 'NONE', #9308, #18850, #25736 ) ;
#7231 = ORIENTED_EDGE ( 'NONE', *, *, #23751, .T. ) ;
#7232 = ORIENTED_EDGE ( 'NONE', *, *, #23, .F. ) ;
#7233 = CYLINDRICAL_SURFACE ( 'NONE', #1207, 9.999999999999998224 ) ;
#7234 = CARTESIAN_POINT ( 'NONE',  ( 133.7812500000000284, 2.485281374238585972, 6.000000000000005329 ) ) ;
#7235 = ORIENTED_EDGE ( 'NONE', *, *, #14496, .T. ) ;
#7236 = CARTESIAN_POINT ( 'NONE',  ( -5.412658773652739619, 3.124999999999975131, -143.3169872981078186 ) ) ;
#7237 = CARTESIAN_POINT ( 'NONE',  ( 23.96132486540522422, 5.551115123125782702E-14, 2.500000000000002220 ) ) ;
#7238 = VECTOR ( 'NONE', #1158, 1000.000000000000000 ) ;
#7239 = CYLINDRICAL_SURFACE ( 'NONE', #30275, 6.000000000000000888 ) ;
#7240 = CARTESIAN_POINT ( 'NONE',  ( 144.5699251345947687, 2.278174593052290753, 5.499999999999732658 ) ) ;
#7241 = EDGE_CURVE ( 'NONE', #28373, #22535, #8230, .T. ) ;
#7242 = CARTESIAN_POINT ( 'NONE',  ( 0.9562047175114668507, -15.26206247212127209, 8.566170523763496192 ) ) ;
#7243 = DIRECTION ( 'NONE',  ( -1.000000000000000000, 5.551115123125774690E-17, 0.000000000000000000 ) ) ;
#7244 =( BOUNDED_CURVE ( )  B_SPLINE_CURVE ( 2, ( #27016, #24723, #3970, #3663, #22435, #15706, #24871, #20129, #27168 ),
 .UNSPECIFIED., .F., .T. ) 
 B_SPLINE_CURVE_WITH_KNOTS ( ( 3, 2, 2, 2, 3 ),
 ( 0.5249999999999999112, 0.5259259259259259078, 0.5277777777777777901, 0.5296296296296296724, 0.5305555555555555580 ),
 .UNSPECIFIED. ) 
 CURVE ( )  GEOMETRIC_REPRESENTATION_ITEM ( )  RATIONAL_B_SPLINE_CURVE ( ( 0.9330127018922194093, 0.9330127018922114157, 1.000000000000000000, 0.8660254037844388186, 1.000000000000000000, 0.8660254037844388186, 1.000000000000000000, 0.9330127018922194093, 0.9330127018922194093 ) ) 
 REPRESENTATION_ITEM ( '' )  );
#7245 = CARTESIAN_POINT ( 'NONE',  ( 146.7038997308104342, 2.071067811865468400, 4.999999999999989342 ) ) ;
#7246 = DIRECTION ( 'NONE',  ( 1.000000000000000000, -5.551115123125773458E-17, -1.260129944081490338E-35 ) ) ;
#7247 = CARTESIAN_POINT ( 'NONE',  ( -6.000000000000007105, -1.607695154586655129, -70.34668783648702117 ) ) ;
#7248 = CARTESIAN_POINT ( 'NONE',  ( 24.82780942950758529, -0.3038553683458247168, -2.156145084836660342 ) ) ;
#7249 = CARTESIAN_POINT ( 'NONE',  ( 108.8988248654050608, 0.8284271247462354770, 2.000000000000212275 ) ) ;
#7250 = CARTESIAN_POINT ( 'NONE',  ( 109.1874999999997584, 1.035533905932839227, 2.500000000000205169 ) ) ;
#7251 = EDGE_CURVE ( 'NONE', #22616, #5051, #19883, .T. ) ;
#7252 = CARTESIAN_POINT ( 'NONE',  ( 135.0000000000000284, -54.99999999999993605, 8.000000000000007105 ) ) ;
#7253 = ORIENTED_EDGE ( 'NONE', *, *, #12748, .T. ) ;
#7254 = CARTESIAN_POINT ( 'NONE',  ( 5.196152422706629359, -2.999999999999988898, -106.7113248654052455 ) ) ;
#7255 = CARTESIAN_POINT ( 'NONE',  ( 5.196152422706629359, -2.999999999999988898, -132.7886751345947971 ) ) ;
#7256 = FACE_OUTER_BOUND ( 'NONE', #12432, .T. ) ;
#7257 = CARTESIAN_POINT ( 'NONE',  ( 3.464101615137757051, -5.999999999999979572, -163.8363248654052597 ) ) ;
#7258 = EDGE_LOOP ( 'NONE', ( #21068, #10798, #2570, #19326, #29223 ) ) ;
#7259 = CARTESIAN_POINT ( 'NONE',  ( 119.0622167782374561, -1.849990392679381701, 0.7662911109078888172 ) ) ;
#7260 = VECTOR ( 'NONE', #20841, 1000.000000000000000 ) ;
#7261 = CARTESIAN_POINT ( 'NONE',  ( 138.9375000000000568, -4.242640687119298093, -4.242640687119298093 ) ) ;
#7262 = CARTESIAN_POINT ( 'NONE',  ( 3.608439182435180470, 6.249999999999982236, -104.6919872981078328 ) ) ;
#7263 = PRESENTATION_LAYER_ASSIGNMENT (  '', '', ( #20501 ) ) ;
#7264 = CARTESIAN_POINT ( 'NONE',  ( 142.8824251345948824, 5.500000000000012434, 2.278174593052012309 ) ) ;
#7265 =( GEOMETRIC_REPRESENTATION_CONTEXT ( 3 ) GLOBAL_UNCERTAINTY_ASSIGNED_CONTEXT ( ( #5123 ) ) GLOBAL_UNIT_ASSIGNED_CONTEXT ( ( #21918, #558, #26354 ) ) REPRESENTATION_CONTEXT ( 'NONE', 'WORKASPACE' ) );
#7266 = TOROIDAL_SURFACE ( 'NONE', #12697, 10.49999999999999645, 0.5000000000000000000 ) ;
#7267 = CARTESIAN_POINT ( 'NONE',  ( 133.0312500000000568, -2.485281374238555774, -6.000000000000005329 ) ) ;
#7268 = CARTESIAN_POINT ( 'NONE',  ( 119.5624999999998153, -2.499999999999874767, -1.035533905932629173 ) ) ;
#7269 = CARTESIAN_POINT ( 'NONE',  ( 4.763139720814407951, 2.750000000000002665, -130.7500000000000284 ) ) ;
#7270 = ORIENTED_EDGE ( 'NONE', *, *, #9650, .T. ) ;
#7271 = AXIS2_PLACEMENT_3D ( 'NONE', #18685, #26016, #28160 ) ;
#7272 = VERTEX_POINT ( 'NONE', #15180 ) ;
#7273 = FACE_OUTER_BOUND ( 'NONE', #13050, .T. ) ;
#7274 = CARTESIAN_POINT ( 'NONE',  ( -4.763139720814407951, 2.749999999999946709, -62.75000000000002842 ) ) ;
#7275 = EDGE_CURVE ( 'NONE', #22336, #26257, #29722, .T. ) ;
#7276 = DIRECTION ( 'NONE',  ( 0.000000000000000000, 0.000000000000000000, -1.000000000000000000 ) ) ;
#7277 = CARTESIAN_POINT ( 'NONE',  ( -6.000000000000000888, 1.067854986875958443E-15, 7.560779664488942560E-35 ) ) ;
#7278 = EDGE_CURVE ( 'NONE', #5282, #886, #23161, .T. ) ;
#7279 = CARTESIAN_POINT ( 'NONE',  ( -7.216878364870328078, 0.000000000000000000, -87.05801270189222407 ) ) ;
#7280 = CARTESIAN_POINT ( 'NONE',  ( 6.000000000000000888, 1.743066579297358182E-13, -65.16367513459479710 ) ) ;
#7281 = CARTESIAN_POINT ( 'NONE',  ( 104.3747167782376124, -5.551115123125782702E-14, -1.849990392679523588 ) ) ;
#7282 = CARTESIAN_POINT ( 'NONE',  ( -5.196152422706573404, -3.000000000000002665, -176.2113248654052597 ) ) ;
#7283 = CYLINDRICAL_SURFACE ( 'NONE', #20170, 6.000000000000000888 ) ;
#7284 = CARTESIAN_POINT ( 'NONE',  ( 118.4377832217621034, 1.849990392679591977, 0.7662911109080090544 ) ) ;
#7285 = CARTESIAN_POINT ( 'NONE',  ( -6.350852961085760029, -1.281975124255709124E-13, -142.1250000000000000 ) ) ;
#7286 = CARTESIAN_POINT ( 'NONE',  ( 139.9650691573131098, -9.167294735415024931, 7.745767522440335284 ) ) ;
#7287 = CARTESIAN_POINT ( 'NONE',  ( -3.608439182435052128, -6.250000000000110134, -155.8080127018922383 ) ) ;
#7288 = FILL_AREA_STYLE_COLOUR ( '', #10195 ) ;
#7289 = CARTESIAN_POINT ( 'NONE',  ( -6.000000000000007105, -1.607695154586655129, -73.34668783648702117 ) ) ;
#7290 = CARTESIAN_POINT ( 'NONE',  ( 3.175426480543072749, 5.499999999999865885, -78.12500000000001421 ) ) ;
#7291 = DIRECTION ( 'NONE',  ( 1.000000000000000000, -0.000000000000000000, -0.000000000000000000 ) ) ;
#7292 = CARTESIAN_POINT ( 'NONE',  ( 3.175426480543072749, 5.499999999999865885, -63.12500000000001421 ) ) ;
#7293 = CARTESIAN_POINT ( 'NONE',  ( 139.5000000000000000, -9.165151389911669000, 8.000000000000007105 ) ) ;
#7294 = CARTESIAN_POINT ( 'NONE',  ( 144.3898502691896510, 3.535533905932725318, -3.535533905932725318 ) ) ;
#7295 = CARTESIAN_POINT ( 'NONE',  ( 108.3511751345945981, 2.000000000000122125, 0.8284271247464157772 ) ) ;
#7296 = CARTESIAN_POINT ( 'NONE',  ( 160.1250000000000568, 0.000000000000000000, -6.000000000000005329 ) ) ;
#7297 = CARTESIAN_POINT ( 'NONE',  ( 144.3675748654052597, -5.500000000000012434, 2.278174593052012309 ) ) ;
#7298 = B_SPLINE_CURVE_WITH_KNOTS ( 'NONE', 1,
 ( #10503, #24768 ),
 .UNSPECIFIED., .F., .F.,
 ( 2, 2 ),
 ( 0.1800073590160146952, 1.000000000000000000 ),
 .UNSPECIFIED. ) ;
#7299 = CARTESIAN_POINT ( 'NONE',  ( 3.464101615137757051, -5.999999999999979572, -49.83632486540522422 ) ) ;
#7300 = CARTESIAN_POINT ( 'NONE',  ( -15.49999999999999289, -54.99999999999990763, 7.500000000000007105 ) ) ;
#7301 = CARTESIAN_POINT ( 'NONE',  ( 0.000000000000000000, 0.000000000000000000, 0.000000000000000000 ) ) ;
#7302 = VERTEX_POINT ( 'NONE', #4390 ) ;
#7303 = CARTESIAN_POINT ( 'NONE',  ( 151.4062500000000000, 6.000000000000005329, -2.485281374238555774 ) ) ;
#7304 = CARTESIAN_POINT ( 'NONE',  ( 118.7886751345946692, -1.999999999999918510, 2.220446049250313081E-13 ) ) ;
#7305 = CARTESIAN_POINT ( 'NONE',  ( 115.3752832217622881, 1.849990392679579099, 0.000000000000000000 ) ) ;
#7306 = CARTESIAN_POINT ( 'NONE',  ( 19.75000000000009948, 1.665334536937734811E-13, -2.000000000000001776 ) ) ;
#7307 = ORIENTED_EDGE ( 'NONE', *, *, #9780, .F. ) ;
#7308 = VERTEX_POINT ( 'NONE', #11033 ) ;
#7309 = CARTESIAN_POINT ( 'NONE',  ( -2.775557561562891351E-14, -5.500000000000115463, -90.75000000000000000 ) ) ;
#7310 = CARTESIAN_POINT ( 'NONE',  ( 15.75000000000006928, -1.873492889144900975, 1.873492889144900975 ) ) ;
#7311 = ADVANCED_FACE ( 'NONE', ( #13815 ), #27724, .F. ) ;
#7312 = ORIENTED_EDGE ( 'NONE', *, *, #28854, .F. ) ;
#7313 = CARTESIAN_POINT ( 'NONE',  ( 154.3913997308104342, -2.071067811865468400, 4.999999999999989342 ) ) ;
#7314 = CARTESIAN_POINT ( 'NONE',  ( 1.000000000000000888, -14.14213562373095634, 8.500000000000007105 ) ) ;
#7315 = CARTESIAN_POINT ( 'NONE',  ( 6.000000000000000888, 1.607695154586715303, -59.09668783648705670 ) ) ;
#7316 = CARTESIAN_POINT ( 'NONE',  ( 3.175426480543072749, 5.499999999999865885, -175.6250000000000284 ) ) ;
#7317 = CARTESIAN_POINT ( 'NONE',  ( 160.8824251345948824, 5.500000000000012434, 2.278174593052012309 ) ) ;
#7318 = CARTESIAN_POINT ( 'NONE',  ( -4.763139720814407951, 2.749999999999946709, -155.7500000000000568 ) ) ;
#7319 = CARTESIAN_POINT ( 'NONE',  ( 112.7499999999998579, -5.551115123125782702E-14, -2.499999999999946709 ) ) ;
#7320 = CARTESIAN_POINT ( 'NONE',  ( 6.000000000000000888, 1.743066579297358182E-13, -51.66367513459483263 ) ) ;
#7321 = VECTOR ( 'NONE', #10816, 1000.000000000000000 ) ;
#7322 = CARTESIAN_POINT ( 'NONE',  ( 5.196152422706629359, 3.000000000000002665, -59.96132486540523132 ) ) ;
#7323 =( BOUNDED_CURVE ( )  B_SPLINE_CURVE ( 2, ( #27536, #1751, #2222, #1905, #8983, #8833, #29854, #25707, #11626 ),
 .UNSPECIFIED., .F., .F. ) 
 B_SPLINE_CURVE_WITH_KNOTS ( ( 3, 2, 2, 2, 3 ),
 ( 0.4705882352941176405, 0.4779411764705882026, 0.4852941176470588203, 0.4926470588235293824, 0.5000000000000000000 ),
 .UNSPECIFIED. ) 
 CURVE ( )  GEOMETRIC_REPRESENTATION_ITEM ( )  RATIONAL_B_SPLINE_CURVE ( ( 1.000000000000000000, 0.9238795325112867385, 1.000000000000000000, 0.9238795325112867385, 1.000000000000000000, 0.9238795325112867385, 1.000000000000000000, 0.9238795325112867385, 1.000000000000000000 ) ) 
 REPRESENTATION_ITEM ( '' )  );
#7324 = CARTESIAN_POINT ( 'NONE',  ( 4.763139720814407951, -2.749999999999988454, -86.00000000000001421 ) ) ;
#7325 = CARTESIAN_POINT ( 'NONE',  ( 155.6398502691896510, -3.535533905932752852, 3.535533905932725318 ) ) ;
#7326 = ORIENTED_EDGE ( 'NONE', *, *, #18079, .T. ) ;
#7327 = CARTESIAN_POINT ( 'NONE',  ( 22.87500000000000711, 1.414213562373312083, -1.414213562373090038 ) ) ;
#7328 = APPLICATION_CONTEXT ( 'automotive_design' ) ;
#7329 = CARTESIAN_POINT ( 'NONE',  ( 111.7499999999998010, 0.000000000000000000, -2.499999999999946709 ) ) ;
#7330 = CARTESIAN_POINT ( 'NONE',  ( 116.0000000000000142, 6.735557395310442023E-16, 5.500000000000000000 ) ) ;
#7331 = CARTESIAN_POINT ( 'NONE',  ( 108.0627832217621034, -0.7662911109077388261, -1.849990392679351725 ) ) ;
#7332 = CARTESIAN_POINT ( 'NONE',  ( 112.7738248654049755, 2.000000000000091926, 0.8284271247462955401 ) ) ;
#7333 =( BOUNDED_CURVE ( )  B_SPLINE_CURVE ( 2, ( #23860, #16680, #9889, #9435, #14659, #494, #16533, #19114, #26002 ),
 .UNSPECIFIED., .F., .T. ) 
 B_SPLINE_CURVE_WITH_KNOTS ( ( 3, 2, 2, 2, 3 ),
 ( 0.01388888888888888465, 0.01481481481481481538, 0.01666666666666666644, 0.01851851851851851749, 0.01944444444444445169 ),
 .UNSPECIFIED. ) 
 CURVE ( )  GEOMETRIC_REPRESENTATION_ITEM ( )  RATIONAL_B_SPLINE_CURVE ( ( 0.9330127018922194093, 0.9330127018922190762, 1.000000000000000000, 0.8660254037844388186, 1.000000000000000000, 0.8660254037844388186, 1.000000000000000000, 0.9330127018922189652, 0.9330127018922194093 ) ) 
 REPRESENTATION_ITEM ( '' )  );
#7334 = ORIENTED_EDGE ( 'NONE', *, *, #25239, .T. ) ;
#7335 = CARTESIAN_POINT ( 'NONE',  ( -5.999999999999965361, 1.607695154586723518, -178.4806624327025872 ) ) ;
#7336 = CARTESIAN_POINT ( 'NONE',  ( -19.99999999999998224, -25.00000000000010658, -7.500000000000007105 ) ) ;
#7337 = CARTESIAN_POINT ( 'NONE',  ( 107.4372167782373850, 0.7662911109078287542, -1.849990392679351725 ) ) ;
#7338 = EDGE_CURVE ( 'NONE', #6732, #29422, #13353, .T. ) ;
#7339 = CARTESIAN_POINT ( 'NONE',  ( 110.8363248654051034, 1.414213562373117794, 1.414213562373034527 ) ) ;
#7340 = ORIENTED_EDGE ( 'NONE', *, *, #26796, .T. ) ;
#7341 = EDGE_LOOP ( 'NONE', ( #16774, #11058, #22995, #17067 ) ) ;
#7342 = VERTEX_POINT ( 'NONE', #1943 ) ;
#7343 = CARTESIAN_POINT ( 'NONE',  ( 6.350852961086080661, -9.614813431917819062E-14, -114.3750000000000000 ) ) ;
#7344 = CARTESIAN_POINT ( 'NONE',  ( 17.75000000000015632, -1.873492889144845464, 1.873492889144845464 ) ) ;
#7345 = EDGE_CURVE ( 'NONE', #14802, #21664, #11503, .T. ) ;
#7346 = CARTESIAN_POINT ( 'NONE',  ( -3.608439182435115633, 6.249999999999965361, -120.3080127018922667 ) ) ;
#7347 = ORIENTED_EDGE ( 'NONE', *, *, #16469, .F. ) ;
#7348 = CARTESIAN_POINT ( 'NONE',  ( 159.0863248654052597, 0.000000000000000000, 5.500000000000005329 ) ) ;
#7349 = AXIS2_PLACEMENT_3D ( 'NONE', #25726, #29353, #6630 ) ;
#7350 = CARTESIAN_POINT ( 'NONE',  ( 5.412658773652712085, -3.125000000000086153, -162.0669872981078186 ) ) ;
#7351 = CARTESIAN_POINT ( 'NONE',  ( 109.1249999999999289, 1.767766952966265404, 1.767766952966431937 ) ) ;
#7352 = CIRCLE ( 'NONE', #26467, 12.00000000000000178 ) ;
#7353 =( NAMED_UNIT ( * ) SI_UNIT ( $, .STERADIAN. ) SOLID_ANGLE_UNIT ( ) );
#7354 = ORIENTED_EDGE ( 'NONE', *, *, #14919, .F. ) ;
#7355 = DIRECTION ( 'NONE',  ( 0.000000000000000000, 0.000000000000000000, 1.000000000000000000 ) ) ;
#7356 =( NAMED_UNIT ( * ) PLANE_ANGLE_UNIT ( ) SI_UNIT ( $, .RADIAN. ) );
#7357 = CARTESIAN_POINT ( 'NONE',  ( 3.175426480543072749, 5.499999999999865885, -177.1250000000000284 ) ) ;
#7358 = CARTESIAN_POINT ( 'NONE',  ( 106.8752832217622739, -1.849990392679301543, 2.220446049250313081E-13 ) ) ;
#7359 = CARTESIAN_POINT ( 'NONE',  ( 3.608439182435180470, 6.249999999999982236, -173.0580127018922667 ) ) ;
#7360 = CARTESIAN_POINT ( 'NONE',  ( 119.6636751345947687, -1.414213562373173305, 1.414213562373145550 ) ) ;
#7361 = CARTESIAN_POINT ( 'NONE',  ( 6.000000000000000888, -1.607695154586752384, -101.2306624327026157 ) ) ;
#7362 = CARTESIAN_POINT ( 'NONE',  ( 0.000000000000000000, 5.499999999999991118, -126.0000000000000000 ) ) ;
#7363 = CARTESIAN_POINT ( 'NONE',  ( 3.464101615137757051, -5.999999999999979572, -53.41367513459480421 ) ) ;
#7364 = CARTESIAN_POINT ( 'NONE',  ( 6.350852961086080661, -9.614813431917819062E-14, -117.3750000000000142 ) ) ;
#7365 = DIRECTION ( 'NONE',  ( 0.000000000000000000, -1.000000000000000000, 0.000000000000000000 ) ) ;
#7366 = DIRECTION ( 'NONE',  ( 0.000000000000000000, 0.000000000000000000, 1.000000000000000000 ) ) ;
#7367 = ORIENTED_EDGE ( 'NONE', *, *, #29347, .F. ) ;
#7368 = CARTESIAN_POINT ( 'NONE',  ( -6.000000000000000888, 1.067854986875958443E-15, 7.560779664488942560E-35 ) ) ;
#7369 = CARTESIAN_POINT ( 'NONE',  ( 3.464101615137852974, 5.999999999999884537, -168.4136751345948255 ) ) ;
#7370 = FACE_OUTER_BOUND ( 'NONE', #30006, .T. ) ;
#7371 = EDGE_LOOP ( 'NONE', ( #26911, #8889, #6239, #14577 ) ) ;
#7372 = CARTESIAN_POINT ( 'NONE',  ( -20.99999999999998224, -19.99999999999998934, 4.000000000000003553 ) ) ;
#7373 = EDGE_CURVE ( 'NONE', #15059, #13602, #21796, .T. ) ;
#7374 = CARTESIAN_POINT ( 'NONE',  ( 6.350852961086080661, -9.614813431917819062E-14, -177.3750000000000284 ) ) ;
#7375 = EDGE_CURVE ( 'NONE', #15286, #12915, #25264, .T. ) ;
#7376 = VERTEX_POINT ( 'NONE', #25119 ) ;
#7377 = CARTESIAN_POINT ( 'NONE',  ( -5.999999999999982236, -1.607695154586700426, -125.8466878364870638 ) ) ;
#7378 = CARTESIAN_POINT ( 'NONE',  ( 1.110223024625164183E-16, -2.000000000000012879, -1.776356839400262692E-15 ) ) ;
#7379 = VERTEX_POINT ( 'NONE', #27882 ) ;
#7380 = ORIENTED_EDGE ( 'NONE', *, *, #7251, .T. ) ;
#7381 = CARTESIAN_POINT ( 'NONE',  ( -5.999999999999963585, 8.134310703387671600E-14, -140.9136751345947971 ) ) ;
#7382 = CARTESIAN_POINT ( 'NONE',  ( 133.6875000000000284, 4.242640687119269671, 4.242640687119298093 ) ) ;
#7383 = EDGE_CURVE ( 'NONE', #6328, #20568, #25426, .T. ) ;
#7384 = ORIENTED_EDGE ( 'NONE', *, *, #5104, .F. ) ;
#7385 = CARTESIAN_POINT ( 'NONE',  ( 5.412658773652739619, 3.124999999999988898, -139.3169872981078186 ) ) ;
#7386 = PLANE ( 'NONE',  #14753 ) ;
#7387 = CARTESIAN_POINT ( 'NONE',  ( 12.87500000000016342, -2.649519052838111843, 5.551115123125782702E-14 ) ) ;
#7388 = CARTESIAN_POINT ( 'NONE',  ( -5.196152422706573404, -3.000000000000002665, -116.7886751345948397 ) ) ;
#7389 = AXIS2_PLACEMENT_3D ( 'NONE', #16648, #12487, #24114 ) ;
#7390 = CARTESIAN_POINT ( 'NONE',  ( 17.56250000000009592, -1.999999999999851674, -0.8284271247461753029 ) ) ;
#7391 = CARTESIAN_POINT ( 'NONE',  ( 0.9999999945711265381, -15.13437201258503606, 8.790312755061723493 ) ) ;
#7392 = CARTESIAN_POINT ( 'NONE',  ( 6.000000000000000888, 1.743066579297358182E-13, -91.58632486540523132 ) ) ;
#7393 = VECTOR ( 'NONE', #25816, 1000.000000000000000 ) ;
#7394 = CARTESIAN_POINT ( 'NONE',  ( 135.9226497308104058, 5.000000000000004441, 0.000000000000000000 ) ) ;
#7395 = CARTESIAN_POINT ( 'NONE',  ( 22.91367513459488592, -1.767766952966265404, -1.767766952966598470 ) ) ;
#7396 = CARTESIAN_POINT ( 'NONE',  ( -5.999999999999963585, -1.487416814333745711E-14, -92.33632486540518869 ) ) ;
#7397 = CARTESIAN_POINT ( 'NONE',  ( -5.999999999999963585, 8.134310703387671600E-14, -146.3363248654052313 ) ) ;
#7398 =( GEOMETRIC_REPRESENTATION_CONTEXT ( 3 ) GLOBAL_UNCERTAINTY_ASSIGNED_CONTEXT ( ( #5919 ) ) GLOBAL_UNIT_ASSIGNED_CONTEXT ( ( #21653, #14022, #12014 ) ) REPRESENTATION_CONTEXT ( 'NONE', 'WORKASPACE' ) );
#7399 = CARTESIAN_POINT ( 'NONE',  ( 150.0863248654052313, 0.000000000000000000, 5.500000000000005329 ) ) ;
#7400 = CARTESIAN_POINT ( 'NONE',  ( 105.6874999999997584, -1.035533905932659149, -2.499999999999724221 ) ) ;
#7401 = VECTOR ( 'NONE', #7225, 1000.000000000000000 ) ;
#7402 = ORIENTED_EDGE ( 'NONE', *, *, #17451, .T. ) ;
#7403 = CARTESIAN_POINT ( 'NONE',  ( 4.763139720814407951, -2.749999999999988454, -50.00000000000004263 ) ) ;
#7404 = CARTESIAN_POINT ( 'NONE',  ( -5.196152422706601826, 2.999999999999975131, -52.53867513459481131 ) ) ;
#7405 = CARTESIAN_POINT ( 'NONE',  ( 6.000000000000000888, -1.859271017917181981E-14, -79.58632486540520290 ) ) ;
#7406 = ORIENTED_EDGE ( 'NONE', *, *, #13180, .T. ) ;
#7407 = CARTESIAN_POINT ( 'NONE',  ( 117.9997167782376266, -1.308140751793696044, 1.308140751793751555 ) ) ;
#7408 = CARTESIAN_POINT ( 'NONE',  ( 135.0000000000000284, 6.000000000000005329, 0.000000000000000000 ) ) ;
#7409 = EDGE_CURVE ( 'NONE', #27076, #8039, #2275, .T. ) ;
#7410 = CARTESIAN_POINT ( 'NONE',  ( 5.412658773652712085, -3.125000000000086153, -103.5669872981078186 ) ) ;
#7411 = CARTESIAN_POINT ( 'NONE',  ( -5.999999999999963585, -2.788906526875773208E-15, -176.3363248654052029 ) ) ;
#7412 = CARTESIAN_POINT ( 'NONE',  ( 160.2038997308104911, 2.071067811865468400, 4.999999999999989342 ) ) ;
#7413 = CARTESIAN_POINT ( 'NONE',  ( 119.0624999999998295, 2.500000000000024425, 1.035533905932809473 ) ) ;
#7414 = EDGE_CURVE ( 'NONE', #21999, #605, #4201, .T. ) ;
#7415 = CARTESIAN_POINT ( 'NONE',  ( -6.350852961085760029, -1.281975124255709124E-13, -128.6250000000000000 ) ) ;
#7416 =( BOUNDED_CURVE ( )  B_SPLINE_CURVE ( 2, ( #16779, #26104, #5047, #14478, #7511, #5200, #2901, #12322, #21665 ),
 .UNSPECIFIED., .F., .T. ) 
 B_SPLINE_CURVE_WITH_KNOTS ( ( 3, 2, 2, 2, 3 ),
 ( 0.5916666666666666741, 0.5925925925925925597, 0.5944444444444444420, 0.5962962962962963243, 0.5972222222222222099 ),
 .UNSPECIFIED. ) 
 CURVE ( )  GEOMETRIC_REPRESENTATION_ITEM ( )  RATIONAL_B_SPLINE_CURVE ( ( 0.9330127018922194093, 0.9330127018922194093, 1.000000000000000000, 0.8660254037844388186, 1.000000000000000000, 0.8660254037844388186, 1.000000000000000000, 0.9330127018922194093, 0.9330127018922194093 ) ) 
 REPRESENTATION_ITEM ( '' )  );
#7417 = EDGE_CURVE ( 'NONE', #24851, #17475, #23047, .T. ) ;
#7418 = ORIENTED_EDGE ( 'NONE', *, *, #25279, .T. ) ;
#7419 = CARTESIAN_POINT ( 'NONE',  ( 3.175426480543072749, -5.500000000000105693, -56.12500000000004263 ) ) ;
#7420 = CARTESIAN_POINT ( 'NONE',  ( 140.5000000000000284, -11.02592621076652790, -4.736429266082377687 ) ) ;
#7421 = CARTESIAN_POINT ( 'NONE',  ( 3.608439182435180470, 6.249999999999982236, -84.55801270189220986 ) ) ;
#7422 = DIRECTION ( 'NONE',  ( 0.000000000000000000, 0.000000000000000000, 1.000000000000000000 ) ) ;
#7423 = CARTESIAN_POINT ( 'NONE',  ( 106.6247167782375840, 1.849990392679523588, 0.000000000000000000 ) ) ;
#7424 = DIRECTION ( 'NONE',  ( 1.000000000000000000, -0.000000000000000000, 0.000000000000000000 ) ) ;
#7425 = CARTESIAN_POINT ( 'NONE',  ( 3.175426480543072749, 5.499999999999865885, -138.1250000000000568 ) ) ;
#7426 = DIRECTION ( 'NONE',  ( -1.000000000000000000, -0.000000000000000000, -0.000000000000000000 ) ) ;
#7427 = VECTOR ( 'NONE', #20322, 1000.000000000000000 ) ;
#7428 = CARTESIAN_POINT ( 'NONE',  ( -5.412658773652739619, 3.124999999999975131, -153.1830127018922667 ) ) ;
#7429 = CARTESIAN_POINT ( 'NONE',  ( -5.999999999999971578, 1.607695154586715303, -116.4033121635130072 ) ) ;
#7430 = CARTESIAN_POINT ( 'NONE',  ( -4.763139720814407951, -2.750000000000016431, -74.50000000000001421 ) ) ;
#7431 = CARTESIAN_POINT ( 'NONE',  ( 6.000000000000000888, 1.743066579297358182E-13, -86.16367513459481131 ) ) ;
#7432 = CARTESIAN_POINT ( 'NONE',  ( -6.350852961085760029, -1.281975124255709124E-13, -68.62500000000004263 ) ) ;
#7433 = CARTESIAN_POINT ( 'NONE',  ( 154.9687500000000568, -2.485281374238585972, 6.000000000000005329 ) ) ;
#7434 = CARTESIAN_POINT ( 'NONE',  ( 161.0000000000000284, 6.735557395310442023E-16, 5.500000000000000000 ) ) ;
#7435 = EDGE_CURVE ( 'NONE', #15258, #11662, #20538, .T. ) ;
#7436 = DIRECTION ( 'NONE',  ( 0.000000000000000000, 0.000000000000000000, 1.000000000000000000 ) ) ;
#7437 = CARTESIAN_POINT ( 'NONE',  ( 5.196152422706629359, 3.000000000000002665, -82.46132486540524553 ) ) ;
#7438 = ORIENTED_EDGE ( 'NONE', *, *, #14704, .T. ) ;
#7439 = CARTESIAN_POINT ( 'NONE',  ( 147.7500000000000284, -6.000000000000005329, 0.000000000000000000 ) ) ;
#7440 = VECTOR ( 'NONE', #11833, 1000.000000000000000 ) ;
#7441 = AXIS2_PLACEMENT_3D ( 'NONE', #3783, #17497, #5776 ) ;
#7442 =( NAMED_UNIT ( * ) SI_UNIT ( $, .STERADIAN. ) SOLID_ANGLE_UNIT ( ) );
#7443 = ADVANCED_FACE ( 'NONE', ( #27567 ), #8413, .F. ) ;
#7444 = CARTESIAN_POINT ( 'NONE',  ( 104.7401757384973280, 1.387249626875697306, 1.223929297688219897 ) ) ;
#7445 = CARTESIAN_POINT ( 'NONE',  ( -4.763139720814407951, -2.750000000000016431, -179.5000000000000000 ) ) ;
#7446 = CARTESIAN_POINT ( 'NONE',  ( 22.25000000000010303, 1.110223024625156540E-13, 1.999999999999946265 ) ) ;
#7447 = CARTESIAN_POINT ( 'NONE',  ( -7.216878364870328078, 0.000000000000000000, -153.6919872981078186 ) ) ;
#7448 = ORIENTED_EDGE ( 'NONE', *, *, #22570, .T. ) ;
#7449 = CARTESIAN_POINT ( 'NONE',  ( -4.763139720814407951, 2.749999999999946709, -85.25000000000004263 ) ) ;
#7450 = CARTESIAN_POINT ( 'NONE',  ( 3.608439182435180470, -6.249999999999997335, -100.0580127018922383 ) ) ;
#7451 = ORIENTED_EDGE ( 'NONE', *, *, #10027, .T. ) ;
#7452 = CARTESIAN_POINT ( 'NONE',  ( -1.110223024625164676E-16, 2.000000000000012879, 2.021286199229734960E-15 ) ) ;
#7453 = CARTESIAN_POINT ( 'NONE',  ( 158.0476497308104342, 0.000000000000000000, -5.000000000000004441 ) ) ;
#7454 = VECTOR ( 'NONE', #25809, 1000.000000000000000 ) ;
#7455 =( BOUNDED_CURVE ( )  B_SPLINE_CURVE ( 2, ( #10608, #15394, #10778, #22430, #1368, #20126, #8440, #14556, #30086 ),
 .UNSPECIFIED., .F., .F. ) 
 B_SPLINE_CURVE_WITH_KNOTS ( ( 3, 2, 2, 2, 3 ),
 ( 0.1470588235294117974, 0.1544117647058823595, 0.1617647058823529216, 0.1691176470588234837, 0.1764705882352941568 ),
 .UNSPECIFIED. ) 
 CURVE ( )  GEOMETRIC_REPRESENTATION_ITEM ( )  RATIONAL_B_SPLINE_CURVE ( ( 1.000000000000000000, 0.9238795325112867385, 1.000000000000000000, 0.9238795325112867385, 1.000000000000000000, 0.9238795325112867385, 1.000000000000000000, 0.9238795325112867385, 1.000000000000000000 ) ) 
 REPRESENTATION_ITEM ( '' )  );
#7456 = DIRECTION ( 'NONE',  ( 5.551115123125785167E-17, -1.000000000000000000, -8.881784197001256268E-16 ) ) ;
#7457 = DIRECTION ( 'NONE',  ( 5.551115123125785167E-17, -1.000000000000000000, -8.881784197001256268E-16 ) ) ;
#7458 = CARTESIAN_POINT ( 'NONE',  ( 140.0000000000000284, -10.99818166789400919, 4.800000000000004263 ) ) ;
#7459 = CARTESIAN_POINT ( 'NONE',  ( -6.350852961085760029, -1.281975124255709124E-13, -166.1249999999999716 ) ) ;
#7460 = CARTESIAN_POINT ( 'NONE',  ( 160.6949251345948539, 5.500000000000012434, -2.278174593052012309 ) ) ;
#7461 = CARTESIAN_POINT ( 'NONE',  ( 4.763139720814407951, -2.749999999999988454, -158.0000000000000284 ) ) ;
#7462 = CARTESIAN_POINT ( 'NONE',  ( 111.5624999999997584, -2.499999999999964473, -1.035533905932689347 ) ) ;
#7463 = CARTESIAN_POINT ( 'NONE',  ( 4.763139720814407951, 2.750000000000002665, -91.75000000000000000 ) ) ;
#7464 = CARTESIAN_POINT ( 'NONE',  ( 142.1175748654052029, 5.500000000000012434, -2.278174593052012309 ) ) ;
#7465 = CARTESIAN_POINT ( 'NONE',  ( 24.10117513459489302, 1.035533905932809473, -2.499999999999904521 ) ) ;
#7466 = CARTESIAN_POINT ( 'NONE',  ( 0.000000000000000000, 5.499999999999991118, -85.50000000000001421 ) ) ;
#7467 = CARTESIAN_POINT ( 'NONE',  ( 13.71132486540530060, 2.500000000000113243, -1.665334536937734811E-13 ) ) ;
#7468 = CARTESIAN_POINT ( 'NONE',  ( 109.6488248654050466, 2.000000000000061728, -0.8284271247459952248 ) ) ;
#7469 = CARTESIAN_POINT ( 'NONE',  ( 24.50000000000015987, -1.999999999999835243, -5.551115123125782702E-14 ) ) ;
#7470 = CARTESIAN_POINT ( 'NONE',  ( 114.3749999999998010, -1.767766952966154381, 1.767766952966653982 ) ) ;
#7471 = ADVANCED_FACE ( 'NONE', ( #11048, #1491 ), #26821, .F. ) ;
#7472 = SURFACE_SIDE_STYLE ('',( #19172 ) ) ;
#7473 = DIRECTION ( 'NONE',  ( -7.147005652999508048E-36, 5.642372883946980038E-36, 1.000000000000000000 ) ) ;
#7474 = EDGE_CURVE ( 'NONE', #13496, #6372, #13464, .T. ) ;
#7475 = VERTEX_POINT ( 'NONE', #19939 ) ;
#7476 = LINE ( 'NONE', #14863, #10222 ) ;
#7477 = CARTESIAN_POINT ( 'NONE',  ( 6.000000000000000888, -3.330669073875464691E-16, -7.560779664488942560E-35 ) ) ;
#7478 = CARTESIAN_POINT ( 'NONE',  ( 106.7497167782375129, 1.308140751793612777, 1.308140751793529510 ) ) ;
#7479 = ORIENTED_EDGE ( 'NONE', *, *, #8184, .T. ) ;
#7480 = ORIENTED_EDGE ( 'NONE', *, *, #28701, .F. ) ;
#7481 = CARTESIAN_POINT ( 'NONE',  ( -2.775557561562891351E-14, -5.500000000000115463, -114.7500000000000142 ) ) ;
#7482 = CARTESIAN_POINT ( 'NONE',  ( 17.68750000000000355, -1.097466725451499370, 2.649519052838298805 ) ) ;
#7483 = CARTESIAN_POINT ( 'NONE',  ( 2.775557561562891351E-14, 6.250000000000033751, -126.4330127018922241 ) ) ;
#7484 = UNCERTAINTY_MEASURE_WITH_UNIT (LENGTH_MEASURE( 1.000000000000000082E-05 ), #13423, 'distance_accuracy_value', 'NONE');
#7485 = VECTOR ( 'NONE', #6936, 1000.000000000000000 ) ;
#7486 = ORIENTED_EDGE ( 'NONE', *, *, #13440, .T. ) ;
#7487 = CARTESIAN_POINT ( 'NONE',  ( 5.196152422706629359, -2.999999999999988898, -68.28867513459479710 ) ) ;
#7488 = CARTESIAN_POINT ( 'NONE',  ( -3.608439182435052128, -6.250000000000110134, -160.9419872981077901 ) ) ;
#7489 = CARTESIAN_POINT ( 'NONE',  ( 107.6874999999997726, -1.035533905932659149, -2.499999999999724221 ) ) ;
#7490 = ORIENTED_EDGE ( 'NONE', *, *, #9039, .T. ) ;
#7491 =( BOUNDED_CURVE ( )  B_SPLINE_CURVE ( 2, ( #16402, #4672, #14107, #27400, #6365, #8847, #15797, #25104, #22823 ),
 .UNSPECIFIED., .F., .T. ) 
 B_SPLINE_CURVE_WITH_KNOTS ( ( 3, 2, 2, 2, 3 ),
 ( 0.04722222222222221405, 0.04814814814814814825, 0.05000000000000000278, 0.05185185185185185036, 0.05277777777777778456 ),
 .UNSPECIFIED. ) 
 CURVE ( )  GEOMETRIC_REPRESENTATION_ITEM ( )  RATIONAL_B_SPLINE_CURVE ( ( 0.9330127018922194093, 0.9330127018922189652, 1.000000000000000000, 0.8660254037844388186, 1.000000000000000000, 0.8660254037844388186, 1.000000000000000000, 0.9330127018922189652, 0.9330127018922194093 ) ) 
 REPRESENTATION_ITEM ( '' )  );
#7492 = CARTESIAN_POINT ( 'NONE',  ( -5.999999999999904965, -1.607695154586834541, -132.7693375672974696 ) ) ;
#7493 = CARTESIAN_POINT ( 'NONE',  ( 107.0627832217620892, -0.7662911109076184779, -1.849990392679351725 ) ) ;
#7494 = DIRECTION ( 'NONE',  ( -1.000000000000000000, -0.000000000000000000, -0.000000000000000000 ) ) ;
#7495 = CARTESIAN_POINT ( 'NONE',  ( 2.775557561562891351E-14, 6.250000000000033751, -178.9330127018922099 ) ) ;
#7496 = CARTESIAN_POINT ( 'NONE',  ( 113.3511751345947403, 2.000000000000001776, 0.8284271247464157772 ) ) ;
#7497 = DIRECTION ( 'NONE',  ( 0.000000000000000000, 0.000000000000000000, 1.000000000000000000 ) ) ;
#7498 = CARTESIAN_POINT ( 'NONE',  ( 6.350852961086080661, -9.614813431917819062E-14, -126.3749999999999858 ) ) ;
#7499 = DIRECTION ( 'NONE',  ( 1.000000000000000000, -0.000000000000000000, -0.000000000000000000 ) ) ;
#7500 = CARTESIAN_POINT ( 'NONE',  ( 4.763139720814407951, -2.749999999999988454, -109.9999999999999858 ) ) ;
#7501 =( BOUNDED_CURVE ( )  B_SPLINE_CURVE ( 2, ( #20759, #11877, #23809, #2898, #21213, #28683, #16920, #14754, #7657 ),
 .UNSPECIFIED., .F., .T. ) 
 B_SPLINE_CURVE_WITH_KNOTS ( ( 3, 2, 2, 2, 3 ),
 ( 0.06944444444444441977, 0.07037037037037041642, 0.07222222222222218768, 0.07407407407407406996, 0.07500000000000006661 ),
 .UNSPECIFIED. ) 
 CURVE ( )  GEOMETRIC_REPRESENTATION_ITEM ( )  RATIONAL_B_SPLINE_CURVE ( ( 0.9330127018922194093, 0.9330127018922154125, 1.000000000000000000, 0.8660254037844388186, 1.000000000000000000, 0.8660254037844388186, 1.000000000000000000, 0.9330127018922154125, 0.9330127018922194093 ) ) 
 REPRESENTATION_ITEM ( '' )  );
#7502 = CARTESIAN_POINT ( 'NONE',  ( -0.5000000000000004441, -14.50000000000001243, -7.500000000000007105 ) ) ;
#7503 = ORIENTED_EDGE ( 'NONE', *, *, #21545, .F. ) ;
#7504 = CARTESIAN_POINT ( 'NONE',  ( 17.37500000000011369, 1.665334536937734811E-13, -2.649519052838444910 ) ) ;
#7505 = CARTESIAN_POINT ( 'NONE',  ( 0.8617483151293284793, -15.74632760175659740, 7.643625642394846764 ) ) ;
#7506 = CARTESIAN_POINT ( 'NONE',  ( 5.999999999999949374, -1.607695154586841868, -136.6533121635129930 ) ) ;
#7507 = CARTESIAN_POINT ( 'NONE',  ( 0.000000000000000000, 0.000000000000000000, 0.000000000000000000 ) ) ;
#7508 = EDGE_CURVE ( 'NONE', #20807, #18212, #21700, .T. ) ;
#7509 = AXIS2_PLACEMENT_3D ( 'NONE', #28427, #21398, #26133 ) ;
#7510 = ORIENTED_EDGE ( 'NONE', *, *, #20517, .F. ) ;
#7511 = CARTESIAN_POINT ( 'NONE',  ( 0.000000000000000000, -5.999999999999991118, -126.4613248654052313 ) ) ;
#7512 = CARTESIAN_POINT ( 'NONE',  ( -2.775557561562891351E-14, -5.500000000000115463, -176.2500000000000284 ) ) ;
#7513 =( NAMED_UNIT ( * ) PLANE_ANGLE_UNIT ( ) SI_UNIT ( $, .RADIAN. ) );
#7514 = ORIENTED_EDGE ( 'NONE', *, *, #21167, .T. ) ;
#7515 = CARTESIAN_POINT ( 'NONE',  ( 22.16367513459488592, 1.767766952966487448, -1.767766952966598470 ) ) ;
#7516 = ORIENTED_EDGE ( 'NONE', *, *, #17878, .F. ) ;
#7517 = VERTEX_POINT ( 'NONE', #19786 ) ;
#7518 = LINE ( 'NONE', #2907, #6140 ) ;
#7519 = CARTESIAN_POINT ( 'NONE',  ( 161.4375000000000284, -4.242640687119298093, -4.242640687119298093 ) ) ;
#7520 = ORIENTED_EDGE ( 'NONE', *, *, #16411, .T. ) ;
#7521 = CARTESIAN_POINT ( 'NONE',  ( -5.412658773652739619, 3.124999999999975131, -131.3169872981078186 ) ) ;
#7522 = PRESENTATION_STYLE_ASSIGNMENT (( #23826 ) ) ;
#7523 = CARTESIAN_POINT ( 'NONE',  ( 10.93750000000009948, -2.649519052838238409, -1.097466725451439196 ) ) ;
#7524 = DIRECTION ( 'NONE',  ( -1.000000000000000000, -0.000000000000000000, -0.000000000000000000 ) ) ;
#7525 = ORIENTED_EDGE ( 'NONE', *, *, #7844, .F. ) ;
#7526 = CARTESIAN_POINT ( 'NONE',  ( 20.50000000000015632, -1.999999999999890754, -5.551115123125782702E-14 ) ) ;
#7527 = DIRECTION ( 'NONE',  ( 1.000000000000000000, -5.551115123125773458E-17, -1.260129944081490338E-35 ) ) ;
#7528 = CARTESIAN_POINT ( 'NONE',  ( 6.000000000000000888, -3.330669073875464691E-16, -7.560779664488942560E-35 ) ) ;
#7529 = CARTESIAN_POINT ( 'NONE',  ( 140.4226497308104342, 5.000000000000004441, 0.000000000000000000 ) ) ;
#7530 = CARTESIAN_POINT ( 'NONE',  ( 137.4300748654051745, 2.278174593051640162, -5.500000000000382805 ) ) ;
#7531 = STYLED_ITEM ( 'NONE', ( #23012 ), #10296 ) ;
#7532 = EDGE_CURVE ( 'NONE', #18704, #16190, #24815, .T. ) ;
#7533 = CARTESIAN_POINT ( 'NONE',  ( 116.0000000000000142, 0.000000000000000000, 0.000000000000000000 ) ) ;
#7534 = CARTESIAN_POINT ( 'NONE',  ( 104.9999999999998579, 2.500000000000002220, 0.000000000000000000 ) ) ;
#7535 = CARTESIAN_POINT ( 'NONE',  ( 0.000000000000000000, -5.999999999999991118, -142.9613248654052597 ) ) ;
#7536 = CARTESIAN_POINT ( 'NONE',  ( 6.350852961086080661, -9.614813431917819062E-14, -135.3750000000000284 ) ) ;
#7537 = CARTESIAN_POINT ( 'NONE',  ( 114.8511751345945981, -2.000000000000001776, -0.8284271247460553989 ) ) ;
#7538 =( BOUNDED_CURVE ( )  B_SPLINE_CURVE ( 2, ( #7587, #23747, #12397, #19726, #28479, #7738, #16854, #2679, #14686 ),
 .UNSPECIFIED., .F., .F. ) 
 B_SPLINE_CURVE_WITH_KNOTS ( ( 3, 2, 2, 2, 3 ),
 ( 0.1305555555555556468, 0.1314814814814815325, 0.1333333333333333037, 0.1351851851851851860, 0.1361111111111110716 ),
 .UNSPECIFIED. ) 
 CURVE ( )  GEOMETRIC_REPRESENTATION_ITEM ( )  RATIONAL_B_SPLINE_CURVE ( ( 0.9330127018922194093, 0.9330127018922234061, 1.000000000000000000, 0.8660254037844388186, 1.000000000000000000, 0.8660254037844388186, 1.000000000000000000, 0.9330127018922234061, 0.9330127018922194093 ) ) 
 REPRESENTATION_ITEM ( '' )  );
#7539 = ORIENTED_EDGE ( 'NONE', *, *, #13768, .T. ) ;
#7540 =( BOUNDED_CURVE ( )  B_SPLINE_CURVE ( 2, ( #21387, #19235, #9861, #14499, #12494, #16941, #5665, #7824, #23836 ),
 .UNSPECIFIED., .F., .F. ) 
 B_SPLINE_CURVE_WITH_KNOTS ( ( 3, 2, 2, 2, 3 ),
 ( 0.7656250000000000000, 0.7734375000000000000, 0.7812500000000000000, 0.7890625000000000000, 0.7968750000000000000 ),
 .UNSPECIFIED. ) 
 CURVE ( )  GEOMETRIC_REPRESENTATION_ITEM ( )  RATIONAL_B_SPLINE_CURVE ( ( 1.000000000000000000, 0.9238795325112867385, 1.000000000000000000, 0.9238795325112867385, 1.000000000000000000, 0.9238795325112867385, 1.000000000000000000, 0.9238795325112867385, 1.000000000000000000 ) ) 
 REPRESENTATION_ITEM ( '' )  );
#7541 = CARTESIAN_POINT ( 'NONE',  ( -5.999999999999963585, 1.780251999655701777E-13, -107.3363248654052455 ) ) ;
#7542 = CARTESIAN_POINT ( 'NONE',  ( 0.000000000000000000, 5.999999999999977796, -88.21132486540523132 ) ) ;
#7543 = CARTESIAN_POINT ( 'NONE',  ( 117.8511751345945129, -1.999999999999941602, -0.8284271247459952248 ) ) ;
#7544 = ADVANCED_FACE ( 'NONE', ( #15368 ), #16614, .T. ) ;
#7545 = EDGE_LOOP ( 'NONE', ( #10436, #14069, #22073, #21409 ) ) ;
#7546 = CARTESIAN_POINT ( 'NONE',  ( 118.9372167782374277, -0.7662911109077686911, 1.849990392679652151 ) ) ;
#7547 = CARTESIAN_POINT ( 'NONE',  ( 118.4136751345946834, 1.414213562373173305, 1.414213562373034527 ) ) ;
#7548 = CARTESIAN_POINT ( 'NONE',  ( 12.43750000000010836, -1.999999999999851674, 0.8284271247462955401 ) ) ;
#7549 = CARTESIAN_POINT ( 'NONE',  ( 3.608439182435180470, -6.249999999999997335, -93.19198729810779014 ) ) ;
#7550 = CARTESIAN_POINT ( 'NONE',  ( 134.5312500000000568, -2.485281374238555774, -6.000000000000005329 ) ) ;
#7551 = CARTESIAN_POINT ( 'NONE',  ( 118.1249999999999147, 1.767766952966320915, 1.767766952966431937 ) ) ;
#7552 = CARTESIAN_POINT ( 'NONE',  ( 3.175426480543072749, -5.500000000000105693, -126.6250000000000000 ) ) ;
#7553 = EDGE_LOOP ( 'NONE', ( #6646, #1152, #1593, #23403 ) ) ;
#7554 = FACE_BOUND ( 'NONE', #7591, .T. ) ;
#7555 = CARTESIAN_POINT ( 'NONE',  ( -3.175426480542816510, 5.499999999999865885, -58.37500000000004974 ) ) ;
#7556 = FACE_OUTER_BOUND ( 'NONE', #22946, .T. ) ;
#7557 = CARTESIAN_POINT ( 'NONE',  ( -3.608439182435115633, 6.249999999999965361, -85.80801270189222407 ) ) ;
#7558 = UNCERTAINTY_MEASURE_WITH_UNIT (LENGTH_MEASURE( 1.000000000000000082E-05 ), #7899, 'distance_accuracy_value', 'NONE');
#7559 = CARTESIAN_POINT ( 'NONE',  ( -4.999999999999886313, -69.50000000000001421, -7.500000000000007105 ) ) ;
#7560 = LINE ( 'NONE', #808, #2511 ) ;
#7561 = EDGE_CURVE ( 'NONE', #26173, #4711, #26155, .T. ) ;
#7562 = CARTESIAN_POINT ( 'NONE',  ( 140.6083823193137903, -11.80419115965732502, -4.059228028636178820 ) ) ;
#7563 = CARTESIAN_POINT ( 'NONE',  ( 114.8752832217623165, -1.849990392679523588, 0.000000000000000000 ) ) ;
#7564 = CARTESIAN_POINT ( 'NONE',  ( 0.000000000000000000, 5.499999999999991118, -139.5000000000000000 ) ) ;
#7565 = CARTESIAN_POINT ( 'NONE',  ( 110.7113248654050182, 2.000000000000057288, 0.000000000000000000 ) ) ;
#7566 = CARTESIAN_POINT ( 'NONE',  ( -7.216878364870328078, 0.000000000000000000, -154.5580127018922383 ) ) ;
#7567 = CARTESIAN_POINT ( 'NONE',  ( 3.464101615137852974, 5.999999999999884537, -158.8363248654052313 ) ) ;
#7568 = CARTESIAN_POINT ( 'NONE',  ( -5.999999999999963585, -1.487416814333745711E-14, -50.91367513459483973 ) ) ;
#7569 = CIRCLE ( 'NONE', #24753, 0.5000000000000000000 ) ;
#7570 = VECTOR ( 'NONE', #11785, 1000.000000000000000 ) ;
#7571 = CARTESIAN_POINT ( 'NONE',  ( -6.350852961085760029, -1.281975124255709124E-13, -70.12500000000004263 ) ) ;
#7572 = ADVANCED_FACE ( 'NONE', ( #608 ), #28208, .T. ) ;
#7573 = CARTESIAN_POINT ( 'NONE',  ( 3.175426480543072749, 5.499999999999865885, -66.12500000000002842 ) ) ;
#7574 = DIRECTION ( 'NONE',  ( 1.000000000000000000, 0.000000000000000000, -0.000000000000000000 ) ) ;
#7575 = CARTESIAN_POINT ( 'NONE',  ( 143.2648502691896510, 3.535533905932725318, 3.535533905932752852 ) ) ;
#7576 = CARTESIAN_POINT ( 'NONE',  ( 154.8750000000000284, 0.000000000000000000, 6.000000000000005329 ) ) ;
#7577 = CARTESIAN_POINT ( 'NONE',  ( 149.1636751345948255, 0.000000000000000000, 5.500000000000005329 ) ) ;
#7578 = CARTESIAN_POINT ( 'NONE',  ( 17.81250000000015277, 0.8284271247463557142, -2.000000000000091926 ) ) ;
#7579 = CARTESIAN_POINT ( 'NONE',  ( -6.000000000000007105, -1.607695154586655129, -89.26933756729744118 ) ) ;
#7580 = CARTESIAN_POINT ( 'NONE',  ( 115.4372167782374561, 0.7662911109078287542, -1.849990392679231599 ) ) ;
#7581 = CARTESIAN_POINT ( 'NONE',  ( -5.999999999999963585, 8.134310703387671600E-14, -145.4136751345948539 ) ) ;
#7582 =( BOUNDED_CURVE ( )  B_SPLINE_CURVE ( 2, ( #1193, #10600, #19953, #23028, #11532, #13687, #27905, #8742, #30072 ),
 .UNSPECIFIED., .F., .T. ) 
 B_SPLINE_CURVE_WITH_KNOTS ( ( 3, 2, 2, 2, 3 ),
 ( 0.7941176470588234837, 0.8014705882352941568, 0.8088235294117647189, 0.8161764705882352811, 0.8235294117647058432 ),
 .UNSPECIFIED. ) 
 CURVE ( )  GEOMETRIC_REPRESENTATION_ITEM ( )  RATIONAL_B_SPLINE_CURVE ( ( 1.000000000000000000, 0.9238795325112867385, 1.000000000000000000, 0.9238795325112867385, 1.000000000000000000, 0.9238795325112867385, 1.000000000000000000, 0.9238795325112867385, 1.000000000000000000 ) ) 
 REPRESENTATION_ITEM ( '' )  );
#7583 = EDGE_LOOP ( 'NONE', ( #14735, #19057, #25588, #7147 ) ) ;
#7584 = CARTESIAN_POINT ( 'NONE',  ( 152.6250000000000284, 0.000000000000000000, -6.000000000000005329 ) ) ;
#7585 = CARTESIAN_POINT ( 'NONE',  ( 161.5000000000000853, -2.984449860524901688, -5.205099329504969674 ) ) ;
#7586 = UNCERTAINTY_MEASURE_WITH_UNIT (LENGTH_MEASURE( 1.000000000000000082E-05 ), #27666, 'distance_accuracy_value', 'NONE');
#7587 = CARTESIAN_POINT ( 'NONE',  ( -5.999999999999963585, 1.780251999655701777E-13, -63.83632486540523132 ) ) ;
#7588 = CARTESIAN_POINT ( 'NONE',  ( 4.763139720814407951, 2.750000000000002665, -178.7500000000000284 ) ) ;
#7589 = CARTESIAN_POINT ( 'NONE',  ( 21.25000000000015632, 0.000000000000000000, 2.000000000000057288 ) ) ;
#7590 = CARTESIAN_POINT ( 'NONE',  ( 3.608439182435180470, 6.249999999999982236, -155.6919872981078186 ) ) ;
#7591 = EDGE_LOOP ( 'NONE', ( #20472, #15837 ) ) ;
#7592 = CARTESIAN_POINT ( 'NONE',  ( -3.175426480542816510, 5.499999999999865885, -82.37500000000002842 ) ) ;
#7593 = CARTESIAN_POINT ( 'NONE',  ( 119.9999999999998295, 2.338294422934558803, 0.6637900606655252611 ) ) ;
#7594 = CARTESIAN_POINT ( 'NONE',  ( 4.763139720814407951, 2.750000000000002665, -168.2500000000000000 ) ) ;
#7595 = EDGE_CURVE ( 'NONE', #14551, #3730, #7518, .T. ) ;
#7596 = DIRECTION ( 'NONE',  ( -0.000000000000000000, -0.000000000000000000, -1.000000000000000000 ) ) ;
#7597 = DIRECTION ( 'NONE',  ( 1.000000000000000000, -5.551115123125773458E-17, -1.260129944081490338E-35 ) ) ;
#7598 =( NAMED_UNIT ( * ) PLANE_ANGLE_UNIT ( ) SI_UNIT ( $, .RADIAN. ) );
#7599 = CARTESIAN_POINT ( 'NONE',  ( 3.175426480543072749, 5.499999999999865885, -162.1250000000000284 ) ) ;
#7600 = CARTESIAN_POINT ( 'NONE',  ( 4.763139720814407951, 2.750000000000002665, -154.7500000000000568 ) ) ;
#7601 = FACE_OUTER_BOUND ( 'NONE', #14455, .T. ) ;
#7602 = CARTESIAN_POINT ( 'NONE',  ( -5.196152422706573404, -3.000000000000002665, -104.2113248654051887 ) ) ;
#7603 = VECTOR ( 'NONE', #21770, 1000.000000000000000 ) ;
#7604 = CARTESIAN_POINT ( 'NONE',  ( -2.775557561562891351E-14, -5.500000000000115463, -98.25000000000000000 ) ) ;
#7605 = CARTESIAN_POINT ( 'NONE',  ( 5.196152422706629359, 3.000000000000002665, -125.9613248654052313 ) ) ;
#7606 = CARTESIAN_POINT ( 'NONE',  ( 144.8511751345948255, -3.889087296526011706, 3.889087296526011706 ) ) ;
#7607 = EDGE_CURVE ( 'NONE', #28323, #1437, #17075, .T. ) ;
#7608 = CARTESIAN_POINT ( 'NONE',  ( -6.350852961085760029, -1.281975124255709124E-13, -89.62500000000000000 ) ) ;
#7609 = CYLINDRICAL_SURFACE ( 'NONE', #22165, 6.000000000000000888 ) ;
#7610 = CARTESIAN_POINT ( 'NONE',  ( 156.3898502691896510, 3.535533905932725318, -3.535533905932725318 ) ) ;
#7611 = CARTESIAN_POINT ( 'NONE',  ( -3.464101615137757051, -5.999999999999979572, -72.58632486540520290 ) ) ;
#7612 = CARTESIAN_POINT ( 'NONE',  ( 109.2113248654051745, -1.999999999999946265, 0.000000000000000000 ) ) ;
#7613 = CARTESIAN_POINT ( 'NONE',  ( 23.18750000000004619, 0.8284271247462955401, 1.999999999999851674 ) ) ;
#7614 = CARTESIAN_POINT ( 'NONE',  ( 109.6874999999997868, -1.035533905932659149, -2.499999999999724221 ) ) ;
#7615 = DIRECTION ( 'NONE',  ( 1.000000000000000000, -5.551115123125773458E-17, -1.260129944081490338E-35 ) ) ;
#7616 = CARTESIAN_POINT ( 'NONE',  ( 162.0000000000000284, 0.000000000000000000, 0.000000000000000000 ) ) ;
#7617 = CYLINDRICAL_SURFACE ( 'NONE', #1222, 6.000000000000000888 ) ;
#7618 = ORIENTED_EDGE ( 'NONE', *, *, #27114, .T. ) ;
#7619 = AXIS2_PLACEMENT_3D ( 'NONE', #24246, #10291, #19657 ) ;
#7620 = CARTESIAN_POINT ( 'NONE',  ( -0.07769256095283699759, -15.23231281889969679, -7.500000000000007105 ) ) ;
#7621 = CARTESIAN_POINT ( 'NONE',  ( 120.5002832217621886, 1.308140751793723799, 1.308140751793751555 ) ) ;
#7622 = EDGE_LOOP ( 'NONE', ( #12193, #7623, #19248, #2779 ) ) ;
#7623 = ORIENTED_EDGE ( 'NONE', *, *, #27984, .F. ) ;
#7624 = AXIS2_PLACEMENT_3D ( 'NONE', #14542, #2673, #4832 ) ;
#7625 = CARTESIAN_POINT ( 'NONE',  ( -2.775557561562891351E-14, -5.500000000000115463, -107.2500000000000142 ) ) ;
#7626 = CARTESIAN_POINT ( 'NONE',  ( 17.87500000000005684, -2.649519052838167354, -5.551115123125782702E-14 ) ) ;
#7627 = CARTESIAN_POINT ( 'NONE',  ( -3.175426480542816510, 5.499999999999865885, -149.8750000000000568 ) ) ;
#7628 = CARTESIAN_POINT ( 'NONE',  ( 3.608439182435180470, 6.249999999999982236, -123.5580127018922099 ) ) ;
#7629 = EDGE_LOOP ( 'NONE', ( #10256, #8663, #9468, #2202 ) ) ;
#7630 = CARTESIAN_POINT ( 'NONE',  ( -6.000000000000007105, -1.607695154586655129, -61.34668783648706381 ) ) ;
#7631 = CARTESIAN_POINT ( 'NONE',  ( 3.608439182435180470, -6.249999999999997335, -157.6919872981078470 ) ) ;
#7632 = CARTESIAN_POINT ( 'NONE',  ( 108.6874999999998010, -1.035533905932749299, -2.499999999999844569 ) ) ;
#7633 = CARTESIAN_POINT ( 'NONE',  ( 133.7663997308104342, -4.999999999999989342, -2.071067811865468400 ) ) ;
#7634 = ADVANCED_FACE ( 'NONE', ( #14764 ), #20892, .F. ) ;
#7635 = CARTESIAN_POINT ( 'NONE',  ( 5.412658773652712085, -3.125000000000086153, -62.43301270189222407 ) ) ;
#7636 = ORIENTED_EDGE ( 'NONE', *, *, #27252, .T. ) ;
#7637 = CARTESIAN_POINT ( 'NONE',  ( 0.7909681984462132442, -15.46453874178244980, -8.191422655757447657 ) ) ;
#7638 = EDGE_CURVE ( 'NONE', #8771, #3609, #26882, .T. ) ;
#7639 = CARTESIAN_POINT ( 'NONE',  ( -5.999999999999963585, -1.487416814333745711E-14, -132.8363248654052597 ) ) ;
#7640 = CARTESIAN_POINT ( 'NONE',  ( 141.5550748654052313, -5.500000000000012434, -2.278174593052012309 ) ) ;
#7641 = DIRECTION ( 'NONE',  ( -7.147005652999508048E-36, 5.642372883946980038E-36, 1.000000000000000000 ) ) ;
#7642 = CARTESIAN_POINT ( 'NONE',  ( 105.6877832217623023, -0.7662911109077987781, 1.849990392679532247 ) ) ;
#7643 = PRESENTATION_LAYER_ASSIGNMENT (  '', '', ( #9128 ) ) ;
#7644 = CARTESIAN_POINT ( 'NONE',  ( 3.464101615137757051, -5.999999999999979572, -168.9136751345948255 ) ) ;
#7645 = CARTESIAN_POINT ( 'NONE',  ( -7.216878364870328078, 0.000000000000000000, -171.0580127018922383 ) ) ;
#7646 = CARTESIAN_POINT ( 'NONE',  ( 2.000000000000003109, -1.110223024625156540E-16, -185.0000000000000000 ) ) ;
#7647 = SURFACE_STYLE_FILL_AREA ( #7209 ) ;
#7648 = CARTESIAN_POINT ( 'NONE',  ( 4.763139720814407951, -2.749999999999988454, -119.0000000000000000 ) ) ;
#7649 = FILL_AREA_STYLE ('',( #5783 ) ) ;
#7650 = CARTESIAN_POINT ( 'NONE',  ( 3.175426480543072749, 5.499999999999865885, -112.6249999999999858 ) ) ;
#7651 = LINE ( 'NONE', #5637, #3814 ) ;
#7652 = CARTESIAN_POINT ( 'NONE',  ( 110.2113248654050608, -1.999999999999946265, 0.000000000000000000 ) ) ;
#7653 = CARTESIAN_POINT ( 'NONE',  ( 124.9999999999999432, -69.50000000000000000, -7.500000000000007105 ) ) ;
#7654 = ORIENTED_EDGE ( 'NONE', *, *, #25589, .F. ) ;
#7655 = CARTESIAN_POINT ( 'NONE',  ( 19.06250000000011013, -2.649519052838238409, 1.097466725451439196 ) ) ;
#7656 = DIRECTION ( 'NONE',  ( -7.147005652999508048E-36, 5.642372883946980038E-36, 1.000000000000000000 ) ) ;
#7657 = CARTESIAN_POINT ( 'NONE',  ( -5.999999999999963585, 1.780251999655701777E-13, -56.33632486540525264 ) ) ;
#7658 = FILL_AREA_STYLE_COLOUR ( '', #23130 ) ;
#7659 = CARTESIAN_POINT ( 'NONE',  ( 17.28867513459492145, 2.500000000000113243, -1.110223024625156540E-13 ) ) ;
#7660 = FACE_OUTER_BOUND ( 'NONE', #6562, .T. ) ;
#7661 = VERTEX_POINT ( 'NONE', #21998 ) ;
#7662 = CARTESIAN_POINT ( 'NONE',  ( -6.000000000000007105, -1.607695154586655129, -95.84668783648702117 ) ) ;
#7663 = ORIENTED_EDGE ( 'NONE', *, *, #22890, .T. ) ;
#7664 = ORIENTED_EDGE ( 'NONE', *, *, #27810, .T. ) ;
#7665 = AXIS2_PLACEMENT_3D ( 'NONE', #29018, #26568, #5370 ) ;
#7666 = CARTESIAN_POINT ( 'NONE',  ( -4.999999999999990230, -24.99999999999999289, -7.500000000000007105 ) ) ;
#7667 = CARTESIAN_POINT ( 'NONE',  ( 160.4062500000000284, 6.000000000000005329, -2.485281374238555774 ) ) ;
#7668 =( BOUNDED_CURVE ( )  B_SPLINE_CURVE ( 2, ( #15443, #29675, #29983, #3712, #22323, #6185, #8643, #3557, #4020 ),
 .UNSPECIFIED., .F., .T. ) 
 B_SPLINE_CURVE_WITH_KNOTS ( ( 3, 2, 2, 2, 3 ),
 ( 0.3906250000000000000, 0.3984375000000000000, 0.4062500000000000000, 0.4140625000000000000, 0.4218750000000000000 ),
 .UNSPECIFIED. ) 
 CURVE ( )  GEOMETRIC_REPRESENTATION_ITEM ( )  RATIONAL_B_SPLINE_CURVE ( ( 1.000000000000000000, 0.9238795325112867385, 1.000000000000000000, 0.9238795325112867385, 1.000000000000000000, 0.9238795325112867385, 1.000000000000000000, 0.9238795325112867385, 1.000000000000000000 ) ) 
 REPRESENTATION_ITEM ( '' )  );
#7669 = ORIENTED_EDGE ( 'NONE', *, *, #27746, .T. ) ;
#7670 = CARTESIAN_POINT ( 'NONE',  ( 2.775557561562891351E-14, -6.250000000000061284, -127.8169872981078043 ) ) ;
#7671 = DIRECTION ( 'NONE',  ( 1.000000000000000000, -0.000000000000000000, -0.000000000000000000 ) ) ;
#7672 = CARTESIAN_POINT ( 'NONE',  ( -0.5000000000000004441, -10.00000000000000888, 7.500000000000007105 ) ) ;
#7673 = DIRECTION ( 'NONE',  ( 0.000000000000000000, 0.000000000000000000, -1.000000000000000000 ) ) ;
#7674 = EDGE_LOOP ( 'NONE', ( #5307, #23610, #25821, #1469 ) ) ;
#7675 = CARTESIAN_POINT ( 'NONE',  ( 19.37500000000019895, -1.414213562372979016, 1.414213562373034527 ) ) ;
#7676 = CARTESIAN_POINT ( 'NONE',  ( 8.673617379884035472E-16, -16.43939393939395188, -5.999693900976774685 ) ) ;
#7677 = CARTESIAN_POINT ( 'NONE',  ( -3.464101615137757051, -5.999999999999979572, -92.08632486540523132 ) ) ;
#7678 = EDGE_CURVE ( 'NONE', #29837, #26645, #24013, .T. ) ;
#7679 = CARTESIAN_POINT ( 'NONE',  ( 6.000000000000000888, -3.330669073875464691E-16, -7.560779664488942560E-35 ) ) ;
#7680 =( BOUNDED_CURVE ( )  B_SPLINE_CURVE ( 2, ( #26463, #3566, #10217, #26315, #5272, #24025, #10062, #19439, #26613 ),
 .UNSPECIFIED., .F., .T. ) 
 B_SPLINE_CURVE_WITH_KNOTS ( ( 3, 2, 2, 2, 3 ),
 ( 0.5694444444444444198, 0.5703703703703704164, 0.5722222222222221877, 0.5740740740740740700, 0.5750000000000000666 ),
 .UNSPECIFIED. ) 
 CURVE ( )  GEOMETRIC_REPRESENTATION_ITEM ( )  RATIONAL_B_SPLINE_CURVE ( ( 0.9330127018922194093, 0.9330127018922154125, 1.000000000000000000, 0.8660254037844388186, 1.000000000000000000, 0.8660254037844388186, 1.000000000000000000, 0.9330127018922154125, 0.9330127018922194093 ) ) 
 REPRESENTATION_ITEM ( '' )  );
#7681 = CARTESIAN_POINT ( 'NONE',  ( 138.1726497308104342, -5.000000000000004441, 0.000000000000000000 ) ) ;
#7682 = CARTESIAN_POINT ( 'NONE',  ( -5.999999999999963585, 1.780251999655701777E-13, -99.83632486540521711 ) ) ;
#7683 = CARTESIAN_POINT ( 'NONE',  ( 3.464101615137757051, -5.999999999999979572, -139.8363248654052597 ) ) ;
#7684 = CARTESIAN_POINT ( 'NONE',  ( -3.464101615137757051, -5.999999999999979572, -69.58632486540518869 ) ) ;
#7685 = CARTESIAN_POINT ( 'NONE',  ( 106.4999999999999147, -2.499999999999946709, 1.110223024625156540E-13 ) ) ;
#7686 = AXIS2_PLACEMENT_3D ( 'NONE', #955, #7574, #24306 ) ;
#7687 = CARTESIAN_POINT ( 'NONE',  ( -3.175426480542816510, -5.500000000000057732, -134.3750000000000284 ) ) ;
#7688 = CARTESIAN_POINT ( 'NONE',  ( 154.2261751345948539, -3.889087296526011706, -3.889087296526011706 ) ) ;
#7689 = ORIENTED_EDGE ( 'NONE', *, *, #4930, .F. ) ;
#7690 = CARTESIAN_POINT ( 'NONE',  ( -6.350852961085760029, -1.281975124255709124E-13, -47.62500000000000000 ) ) ;
#7691 = CARTESIAN_POINT ( 'NONE',  ( -5.999999999999963585, 1.780251999655701777E-13, -93.83632486540518869 ) ) ;
#7692 = CARTESIAN_POINT ( 'NONE',  ( -5.999999999999963585, 1.780251999655701777E-13, -100.4136751345948255 ) ) ;
#7693 = VERTEX_POINT ( 'NONE', #17111 ) ;
#7694 = VECTOR ( 'NONE', #6955, 1000.000000000000000 ) ;
#7695 = CARTESIAN_POINT ( 'NONE',  ( 117.3747167782375271, 0.000000000000000000, -1.849990392679301543 ) ) ;
#7696 = CARTESIAN_POINT ( 'NONE',  ( 136.0312500000000284, -2.485281374238556218, -6.000000000000005329 ) ) ;
#7697 = CARTESIAN_POINT ( 'NONE',  ( 5.412658773652739619, 3.124999999999988898, -95.81698729810783277 ) ) ;
#7698 = DIRECTION ( 'NONE',  ( 0.000000000000000000, 0.000000000000000000, -1.000000000000000000 ) ) ;
#7699 = DIRECTION ( 'NONE',  ( 1.000000000000000000, -6.938893903907222067E-15, 0.000000000000000000 ) ) ;
#7700 = CARTESIAN_POINT ( 'NONE',  ( 117.7499999999998721, 1.387778780781445676E-13, -2.499999999999835687 ) ) ;
#7701 = ORIENTED_EDGE ( 'NONE', *, *, #933, .F. ) ;
#7702 = AXIS2_PLACEMENT_3D ( 'NONE', #3613, #11029, #13205 ) ;
#7703 = DIRECTION ( 'NONE',  ( -2.220446049250313574E-16, -1.010643099614860775E-15, 1.000000000000000000 ) ) ;
#7704 = ADVANCED_FACE ( 'NONE', ( #1095 ), #5843, .T. ) ;
#7705 = CARTESIAN_POINT ( 'NONE',  ( 4.763139720814407951, -2.749999999999988454, -126.5000000000000568 ) ) ;
#7706 = ORIENTED_EDGE ( 'NONE', *, *, #13077, .F. ) ;
#7707 = CARTESIAN_POINT ( 'NONE',  ( 10.12500000000007816, 1.414213562373201061, 1.414213562373145550 ) ) ;
#7708 = ORIENTED_EDGE ( 'NONE', *, *, #22539, .F. ) ;
#7709 = CARTESIAN_POINT ( 'NONE',  ( 5.196152422706629359, -2.999999999999988898, -138.2113248654052029 ) ) ;
#7710 = CARTESIAN_POINT ( 'NONE',  ( -3.175426480542816510, -5.500000000000057732, -60.87500000000000000 ) ) ;
#7711 = CARTESIAN_POINT ( 'NONE',  ( 135.0000000000000284, 0.000000000000000000, 0.000000000000000000 ) ) ;
#7712 = CARTESIAN_POINT ( 'NONE',  ( 4.520081486476311028, 10.03271082534597269, -28.96438617129775395 ) ) ;
#7713 = CARTESIAN_POINT ( 'NONE',  ( 2.775557561562891351E-14, -6.250000000000061284, -80.68301270189226670 ) ) ;
#7714 = ADVANCED_FACE ( 'NONE', ( #5541 ), #1236, .F. ) ;
#7715 = CARTESIAN_POINT ( 'NONE',  ( -3.464101615137757051, -5.999999999999979572, -101.0863248654051887 ) ) ;
#7716 = CARTESIAN_POINT ( 'NONE',  ( 0.000000000000000000, 0.000000000000000000, 0.000000000000000000 ) ) ;
#7717 = CARTESIAN_POINT ( 'NONE',  ( 0.000000000000000000, -5.999999999999991118, -152.5386751345948539 ) ) ;
#7718 = CARTESIAN_POINT ( 'NONE',  ( 141.0000000000000284, -12.00000000000001066, -4.000000000000003553 ) ) ;
#7719 = CARTESIAN_POINT ( 'NONE',  ( 116.8127832217622597, -1.849990392679441875, 0.7662911109078888172 ) ) ;
#7720 = CARTESIAN_POINT ( 'NONE',  ( 6.350852961086080661, -9.614813431917819062E-14, -136.8750000000000568 ) ) ;
#7721 = CARTESIAN_POINT ( 'NONE',  ( 139.7459307364638050, -9.280942085683948406, 7.936758083481400661 ) ) ;
#7722 = CARTESIAN_POINT ( 'NONE',  ( -7.216878364870328078, 0.000000000000000000, -150.0580127018922667 ) ) ;
#7723 = CARTESIAN_POINT ( 'NONE',  ( 3.464101615137852974, 5.999999999999884537, -101.8363248654052029 ) ) ;
#7724 = CARTESIAN_POINT ( 'NONE',  ( 3.464101615137852974, 5.999999999999884537, -67.33632486540523132 ) ) ;
#7725 = CARTESIAN_POINT ( 'NONE',  ( -3.175426480542816066, 5.499999999999865885, -68.87500000000002842 ) ) ;
#7726 = CARTESIAN_POINT ( 'NONE',  ( 0.000000000000000000, 5.499999999999991118, -54.00000000000004974 ) ) ;
#7727 = PRESENTATION_STYLE_ASSIGNMENT (( #26312 ) ) ;
#7728 = CARTESIAN_POINT ( 'NONE',  ( 149.5312500000000284, -2.485281374238556218, -6.000000000000005329 ) ) ;
#7729 = DIRECTION ( 'NONE',  ( 7.147005652999508048E-36, -5.642372883946980038E-36, -1.000000000000000000 ) ) ;
#7730 = CARTESIAN_POINT ( 'NONE',  ( 17.06250000000001421, 2.000000000000151879, 0.8284271247461753029 ) ) ;
#7731 = CYLINDRICAL_SURFACE ( 'NONE', #9686, 6.000000000000000888 ) ;
#7732 = CARTESIAN_POINT ( 'NONE',  ( 115.1872167782374987, -1.849990392679441875, -0.7662911109075283278 ) ) ;
#7733 = CARTESIAN_POINT ( 'NONE',  ( -5.999999999999963585, 1.780251999655701777E-13, -81.83632486540521711 ) ) ;
#7734 = ORIENTED_EDGE ( 'NONE', *, *, #30129, .F. ) ;
#7735 = CARTESIAN_POINT ( 'NONE',  ( 146.1562500000000853, -6.000000000000005329, 2.485281374238555774 ) ) ;
#7736 = AXIS2_PLACEMENT_3D ( 'NONE', #29174, #10793, #1384 ) ;
#7737 = ADVANCED_FACE ( 'NONE', ( #3385 ), #2941, .F. ) ;
#7738 = CARTESIAN_POINT ( 'NONE',  ( 3.464101615137852974, 5.999999999999884537, -64.33632486540521711 ) ) ;
#7739 = CARTESIAN_POINT ( 'NONE',  ( -2.775557561562891351E-14, -5.500000000000115463, -179.2500000000000284 ) ) ;
#7740 = CARTESIAN_POINT ( 'NONE',  ( 21.50000000000004619, -1.999999999999890754, -1.665334536937734811E-13 ) ) ;
#7741 = CARTESIAN_POINT ( 'NONE',  ( 2.775557561562891351E-14, -6.250000000000061284, -153.3169872981078186 ) ) ;
#7742 = ORIENTED_EDGE ( 'NONE', *, *, #23552, .T. ) ;
#7743 = CARTESIAN_POINT ( 'NONE',  ( -4.763139720814407951, 2.749999999999946709, -79.25000000000004263 ) ) ;
#7744 = ADVANCED_FACE ( 'NONE', ( #12811 ), #21708, .T. ) ;
#7745 = CARTESIAN_POINT ( 'NONE',  ( -3.608439182435052128, -6.250000000000110134, -98.80801270189222407 ) ) ;
#7746 = DIRECTION ( 'NONE',  ( 1.000000000000000000, -5.551115123125773458E-17, -1.260129944081490338E-35 ) ) ;
#7747 = CARTESIAN_POINT ( 'NONE',  ( 5.380303083296117173, -9.596003543682449788, -22.31547897336681174 ) ) ;
#7748 = SHAPE_REPRESENTATION_RELATIONSHIP ( 'NONE' , 'NONE' ,  #4035, #24617 ) ;
#7749 = CARTESIAN_POINT ( 'NONE',  ( -3.175426480542816066, 5.499999999999865885, -161.8750000000000000 ) ) ;
#7750 = CARTESIAN_POINT ( 'NONE',  ( 5.999999999999999112, 2.951592740943527306E-14, -162.0863248654052029 ) ) ;
#7751 = CARTESIAN_POINT ( 'NONE',  ( 3.175426480543072749, -5.500000000000105693, -150.6250000000000284 ) ) ;
#7752 = CARTESIAN_POINT ( 'NONE',  ( 0.000000000000000000, 0.000000000000000000, 0.000000000000000000 ) ) ;
#7753 = CARTESIAN_POINT ( 'NONE',  ( -4.763139720814407951, -2.750000000000016431, -97.00000000000002842 ) ) ;
#7754 = CARTESIAN_POINT ( 'NONE',  ( 1.110223024625164183E-16, -2.000000000000012879, -1.776356839400262692E-15 ) ) ;
#7755 = CARTESIAN_POINT ( 'NONE',  ( 3.175426480543072749, 5.499999999999865885, -79.62500000000002842 ) ) ;
#7756 =( BOUNDED_CURVE ( )  B_SPLINE_CURVE ( 2, ( #9968, #738, #10121, #12155, #427, #5326, #582, #9816, #17199 ),
 .UNSPECIFIED., .F., .T. ) 
 B_SPLINE_CURVE_WITH_KNOTS ( ( 3, 2, 2, 2, 3 ),
 ( 0.8624999999999993783, 0.8687499999999996891, 0.8749999999999998890, 0.8812500000000000888, 0.8875000000000003997 ),
 .UNSPECIFIED. ) 
 CURVE ( )  GEOMETRIC_REPRESENTATION_ITEM ( )  RATIONAL_B_SPLINE_CURVE ( ( 1.000000000000008216, 0.9238795325112786339, 1.000000000000000000, 0.9238795325112867385, 1.000000000000000000, 0.9238795325112867385, 1.000000000000000000, 0.9238795325112812984, 1.000000000000005329 ) ) 
 REPRESENTATION_ITEM ( '' )  );
#7757 = FACE_OUTER_BOUND ( 'NONE', #23337, .T. ) ;
#7758 = CARTESIAN_POINT ( 'NONE',  ( 9.562500000000028422, 2.649519052838298805, -1.097466725451559322 ) ) ;
#7759 = CARTESIAN_POINT ( 'NONE',  ( 110.9999999999999147, 2.500000000000057732, 0.000000000000000000 ) ) ;
#7760 = CARTESIAN_POINT ( 'NONE',  ( 6.000000000000052403, -1.607695154586662678, -66.15331216351299304 ) ) ;
#7761 = CARTESIAN_POINT ( 'NONE',  ( 6.000000000000000888, -3.330669073875464691E-16, -7.560779664488942560E-35 ) ) ;
#7762 = ORIENTED_EDGE ( 'NONE', *, *, #19625, .T. ) ;
#7763 = CARTESIAN_POINT ( 'NONE',  ( 0.000000000000000000, 5.999999999999977796, -91.21132486540523132 ) ) ;
#7764 = CARTESIAN_POINT ( 'NONE',  ( -5.999999999999963585, 3.021315404115420679E-15, -178.4136751345947971 ) ) ;
#7765 = CARTESIAN_POINT ( 'NONE',  ( 129.9999999999998010, -89.00000000000001421, 4.000000000000003553 ) ) ;
#7766 = CARTESIAN_POINT ( 'NONE',  ( 121.1877832217620750, 0.7662911109077987781, -1.849990392679291551 ) ) ;
#7767 = EDGE_CURVE ( 'NONE', #24100, #13876, #7124, .T. ) ;
#7768 = EDGE_LOOP ( 'NONE', ( #6540, #9827, #9192, #29555 ) ) ;
#7769 = ORIENTED_EDGE ( 'NONE', *, *, #22745, .T. ) ;
#7770 = CARTESIAN_POINT ( 'NONE',  ( -3.175426480542816510, -5.500000000000057732, -107.3750000000000284 ) ) ;
#7771 = CARTESIAN_POINT ( 'NONE',  ( 19.12500000000014211, 1.110223024625156540E-13, -2.649519052838444910 ) ) ;
#7772 = EDGE_CURVE ( 'NONE', #6031, #27584, #21869, .T. ) ;
#7773 = CARTESIAN_POINT ( 'NONE',  ( 3.608439182435180470, 6.249999999999982236, -122.0580127018922667 ) ) ;
#7774 = EDGE_CURVE ( 'NONE', #26402, #25744, #29959, .T. ) ;
#7775 = ORIENTED_EDGE ( 'NONE', *, *, #8154, .T. ) ;
#7776 = CARTESIAN_POINT ( 'NONE',  ( -5.999999999999963585, 1.780251999655701777E-13, -110.9136751345948255 ) ) ;
#7777 = CARTESIAN_POINT ( 'NONE',  ( 3.608439182435180470, 6.249999999999982236, -158.6919872981078470 ) ) ;
#7778 = LINE ( 'NONE', #26518, #24024 ) ;
#7779 = CARTESIAN_POINT ( 'NONE',  ( -5.412658773652739619, 3.124999999999975131, -60.18301270189224539 ) ) ;
#7780 = VERTEX_POINT ( 'NONE', #17716 ) ;
#7781 = CARTESIAN_POINT ( 'NONE',  ( 0.8631338372297805428, -15.37878787878787534, -8.351220472436786224 ) ) ;
#7782 = AXIS2_PLACEMENT_3D ( 'NONE', #27625, #20435, #3982 ) ;
#7783 = DIRECTION ( 'NONE',  ( 0.000000000000000000, 1.000000000000000000, 0.000000000000000000 ) ) ;
#7784 = CARTESIAN_POINT ( 'NONE',  ( 24.99999999999999289, 5.550594706083218745E-14, 1.999999999999776179 ) ) ;
#7785 = CARTESIAN_POINT ( 'NONE',  ( 0.000000000000000000, 5.499999999999991118, -171.0000000000000284 ) ) ;
#7786 = CARTESIAN_POINT ( 'NONE',  ( 105.8752832217621602, -1.849990392679412565, 2.220446049250313081E-13 ) ) ;
#7787 = CARTESIAN_POINT ( 'NONE',  ( 3.464101615137757051, -5.999999999999979572, -112.8363248654051887 ) ) ;
#7788 = CARTESIAN_POINT ( 'NONE',  ( -5.412658773652684552, -3.125000000000099920, -166.4330127018922667 ) ) ;
#7789 = CARTESIAN_POINT ( 'NONE',  ( 113.6636751345946408, -1.414213562373034527, 1.414213562373034527 ) ) ;
#7790 = CARTESIAN_POINT ( 'NONE',  ( 24.56250000000017764, -1.999999999999911626, -0.8284271247462354770 ) ) ;
#7791 = CARTESIAN_POINT ( 'NONE',  ( -3.175426480542816066, -5.500000000000057732, -116.3749999999999858 ) ) ;
#7792 = CARTESIAN_POINT ( 'NONE',  ( 3.175426480543072749, 5.499999999999865885, -114.1249999999999858 ) ) ;
#7793 = DIRECTION ( 'NONE',  ( 0.000000000000000000, 0.000000000000000000, -1.000000000000000000 ) ) ;
#7794 = CARTESIAN_POINT ( 'NONE',  ( 11.10117513459493033, 1.035533905932929599, -2.500000000000024425 ) ) ;
#7795 = CARTESIAN_POINT ( 'NONE',  ( 24.50000000000013145, 0.6095397824029125111, -2.424553825690234365 ) ) ;
#7796 = EDGE_LOOP ( 'NONE', ( #14786, #13575, #4800, #25046 ) ) ;
#7797 = CARTESIAN_POINT ( 'NONE',  ( 17.87500000000014211, 1.665334536937734811E-13, 2.649519052838167354 ) ) ;
#7798 = CARTESIAN_POINT ( 'NONE',  ( 0.000000000000000000, 5.999999999999977796, -168.2886751345948255 ) ) ;
#7799 = CARTESIAN_POINT ( 'NONE',  ( 5.196152422706629359, -2.999999999999988898, -145.7113248654052313 ) ) ;
#7800 = VERTEX_POINT ( 'NONE', #17877 ) ;
#7801 = CARTESIAN_POINT ( 'NONE',  ( 6.350852961086080661, -9.614813431917819062E-14, -178.8750000000000284 ) ) ;
#7802 = CARTESIAN_POINT ( 'NONE',  ( 2.775557561562891351E-14, 6.250000000000033751, -79.06698729810779014 ) ) ;
#7803 = EDGE_CURVE ( 'NONE', #20342, #22235, #23002, .T. ) ;
#7804 = CARTESIAN_POINT ( 'NONE',  ( -3.464101615137725076, 5.999999999999979572, -109.6636751345947971 ) ) ;
#7805 = ORIENTED_EDGE ( 'NONE', *, *, #13913, .F. ) ;
#7806 = CARTESIAN_POINT ( 'NONE',  ( -5.999999999999971578, 1.607695154586715303, -143.9806624327026441 ) ) ;
#7807 = ADVANCED_FACE ( 'NONE', ( #3692 ), #2018, .T. ) ;
#7808 = AXIS2_PLACEMENT_3D ( 'NONE', #18338, #13587, #20002 ) ;
#7809 = ORIENTED_EDGE ( 'NONE', *, *, #27468, .F. ) ;
#7810 = EDGE_LOOP ( 'NONE', ( #7232, #12925, #272, #16419 ) ) ;
#7811 = CARTESIAN_POINT ( 'NONE',  ( 132.7500000000000284, -6.000000000000005329, 0.000000000000000000 ) ) ;
#7812 = CARTESIAN_POINT ( 'NONE',  ( 159.9375000000000284, -4.242640687119298093, -4.242640687119298093 ) ) ;
#7813 = VECTOR ( 'NONE', #7160, 1000.000000000000000 ) ;
#7814 = ORIENTED_EDGE ( 'NONE', *, *, #4940, .T. ) ;
#7815 = CARTESIAN_POINT ( 'NONE',  ( 2.775557561562891351E-14, 6.250000000000033751, -133.0669872981078470 ) ) ;
#7816 = DIRECTION ( 'NONE',  ( -1.000000000000000000, -1.665334536937736783E-16, -2.220446049250315546E-16 ) ) ;
#7817 = LINE ( 'NONE', #26559, #5240 ) ;
#7818 = DIRECTION ( 'NONE',  ( -7.147005652999508048E-36, 5.642372883946980038E-36, 1.000000000000000000 ) ) ;
#7819 = ORIENTED_EDGE ( 'NONE', *, *, #25616, .F. ) ;
#7820 = CARTESIAN_POINT ( 'NONE',  ( 14.12500000000013678, 1.414213562373201061, 1.414213562373034527 ) ) ;
#7821 = CARTESIAN_POINT ( 'NONE',  ( 3.464101615137852974, 5.999999999999884537, -135.4136751345947971 ) ) ;
#7822 = CARTESIAN_POINT ( 'NONE',  ( -3.464101615137757051, -5.999999999999979572, -139.1636751345948824 ) ) ;
#7823 = CARTESIAN_POINT ( 'NONE',  ( 140.0476497308104058, 0.000000000000000000, -5.000000000000004441 ) ) ;
#7824 = CARTESIAN_POINT ( 'NONE',  ( 12.02382486540522599, -1.035533905932629173, 2.499999999999784173 ) ) ;
#7825 = SURFACE_STYLE_FILL_AREA ( #26125 ) ;
#7826 = CARTESIAN_POINT ( 'NONE',  ( 0.000000000000000000, -5.999999999999991118, -162.4613248654052029 ) ) ;
#7827 = CARTESIAN_POINT ( 'NONE',  ( -5.196152422706573404, -3.000000000000002665, -128.7886751345947971 ) ) ;
#7828 = CARTESIAN_POINT ( 'NONE',  ( 106.6249999999999289, -1.767766952966376426, -1.767766952966320915 ) ) ;
#7829 = CARTESIAN_POINT ( 'NONE',  ( 6.000000000000000888, 1.743066579297358182E-13, -64.58632486540520290 ) ) ;
#7830 = AXIS2_PLACEMENT_3D ( 'NONE', #28039, #19016, #12118 ) ;
#7831 = CARTESIAN_POINT ( 'NONE',  ( -2.775557561562891351E-14, -5.500000000000115463, -137.2499999999999716 ) ) ;
#7832 = SURFACE_SIDE_STYLE ('',( #14785 ) ) ;
#7833 = CARTESIAN_POINT ( 'NONE',  ( 104.7401757384972569, 0.9320968428604275990, -1.616116470751321144 ) ) ;
#7834 = AXIS2_PLACEMENT_3D ( 'NONE', #14463, #7494, #10276 ) ;
#7835 = ORIENTED_EDGE ( 'NONE', *, *, #28235, .T. ) ;
#7836 = DIRECTION ( 'NONE',  ( 0.000000000000000000, 5.551115123125769144E-17, -1.000000000000000000 ) ) ;
#7837 = AXIS2_PLACEMENT_3D ( 'NONE', #25025, #8768, #30099 ) ;
#7838 = CARTESIAN_POINT ( 'NONE',  ( -3.175426480542816066, 5.499999999999865885, -49.37500000000000711 ) ) ;
#7839 = CARTESIAN_POINT ( 'NONE',  ( 5.999999999999949374, 1.607695154586804565, -97.51933756729746960 ) ) ;
#7840 = CARTESIAN_POINT ( 'NONE',  ( 153.1800748654052597, -2.278174593052058938, 5.499999999999964473 ) ) ;
#7841 = ORIENTED_EDGE ( 'NONE', *, *, #26025, .F. ) ;
#7842 = CARTESIAN_POINT ( 'NONE',  ( 117.1247167782376408, -1.849990392679579099, 1.110223024625156540E-13 ) ) ;
#7843 = CARTESIAN_POINT ( 'NONE',  ( -3.608439182435052128, -6.250000000000110134, -97.94198729810780435 ) ) ;
#7844 = EDGE_CURVE ( 'NONE', #17914, #18017, #27194, .T. ) ;
#7845 = FACE_OUTER_BOUND ( 'NONE', #22499, .T. ) ;
#7846 =( BOUNDED_CURVE ( )  B_SPLINE_CURVE ( 2, ( #21987, #12643, #16694, #4821, #14932, #17398, #920, #15084, #25720 ),
 .UNSPECIFIED., .F., .F. ) 
 B_SPLINE_CURVE_WITH_KNOTS ( ( 3, 2, 2, 2, 3 ),
 ( 0.7031250000000000000, 0.7109375000000000000, 0.7187500000000000000, 0.7265625000000000000, 0.7343750000000000000 ),
 .UNSPECIFIED. ) 
 CURVE ( )  GEOMETRIC_REPRESENTATION_ITEM ( )  RATIONAL_B_SPLINE_CURVE ( ( 1.000000000000000000, 0.9238795325112867385, 1.000000000000000000, 0.9238795325112867385, 1.000000000000000000, 0.9238795325112867385, 1.000000000000000000, 0.9238795325112867385, 1.000000000000000000 ) ) 
 REPRESENTATION_ITEM ( '' )  );
#7847 = EDGE_CURVE ( 'NONE', #3318, #20198, #2051, .T. ) ;
#7848 = CARTESIAN_POINT ( 'NONE',  ( 155.1636751345948255, 0.000000000000000000, 5.500000000000005329 ) ) ;
#7849 = CARTESIAN_POINT ( 'NONE',  ( 113.9374999999997158, 2.500000000000115019, -1.035533905932629173 ) ) ;
#7850 = ORIENTED_EDGE ( 'NONE', *, *, #17451, .F. ) ;
#7851 = ORIENTED_EDGE ( 'NONE', *, *, #21840, .F. ) ;
#7852 = DIRECTION ( 'NONE',  ( -7.147005652999508048E-36, 5.642372883946980038E-36, 1.000000000000000000 ) ) ;
#7853 = AXIS2_PLACEMENT_3D ( 'NONE', #4081, #11508, #27120 ) ;
#7854 =( BOUNDED_CURVE ( )  B_SPLINE_CURVE ( 2, ( #5102, #11939, #21867, #19272, #19566, #26452, #16978, #2807, #4813 ),
 .UNSPECIFIED., .F., .T. ) 
 B_SPLINE_CURVE_WITH_KNOTS ( ( 3, 2, 2, 2, 3 ),
 ( 0.1083333333333333925, 0.1092592592592592782, 0.1111111111111111605, 0.1129629629629629317, 0.1138888888888888173 ),
 .UNSPECIFIED. ) 
 CURVE ( )  GEOMETRIC_REPRESENTATION_ITEM ( )  RATIONAL_B_SPLINE_CURVE ( ( 0.9330127018922194093, 0.9330127018922234061, 1.000000000000000000, 0.8660254037844388186, 1.000000000000000000, 0.8660254037844388186, 1.000000000000000000, 0.9330127018922234061, 0.9330127018922194093 ) ) 
 REPRESENTATION_ITEM ( '' )  );
#7855 = VERTEX_POINT ( 'NONE', #13577 ) ;
#7856 = CYLINDRICAL_SURFACE ( 'NONE', #22907, 2.499999999999999112 ) ;
#7857 = CARTESIAN_POINT ( 'NONE',  ( -3.175426480542816510, 5.499999999999865885, -55.37500000000004263 ) ) ;
#7858 = CARTESIAN_POINT ( 'NONE',  ( -5.196152422706601826, 2.999999999999975131, -69.03867513459482552 ) ) ;
#7859 = CARTESIAN_POINT ( 'NONE',  ( 6.000000000000026645, -1.607695154586707753, -134.2306624327025872 ) ) ;
#7860 = CARTESIAN_POINT ( 'NONE',  ( 1.965048709171757446, 10.82948053518397025, -19.31713205297535652 ) ) ;
#7861 = CARTESIAN_POINT ( 'NONE',  ( 7.216878364870455975, -6.409875621278545621E-14, -72.80801270189222407 ) ) ;
#7862 = DIRECTION ( 'NONE',  ( 0.000000000000000000, 0.000000000000000000, 1.000000000000000000 ) ) ;
#7863 = CARTESIAN_POINT ( 'NONE',  ( 3.464101615137852974, 5.999999999999884537, -169.3363248654052029 ) ) ;
#7864 = CARTESIAN_POINT ( 'NONE',  ( 0.000000000000000000, 9.000000000000007105, -3.000000000000002665 ) ) ;
#7865 = SURFACE_STYLE_FILL_AREA ( #15596 ) ;
#7866 = CARTESIAN_POINT ( 'NONE',  ( 4.763139720814407951, -2.749999999999988454, -138.5000000000000000 ) ) ;
#7867 = CARTESIAN_POINT ( 'NONE',  ( -5.196152422706573404, -3.000000000000002665, -177.7113248654052029 ) ) ;
#7868 = CARTESIAN_POINT ( 'NONE',  ( 5.412658773652739619, 3.124999999999988898, -152.1830127018922667 ) ) ;
#7869 = CARTESIAN_POINT ( 'NONE',  ( 6.000000000000000888, 1.743066579297358182E-13, -70.58632486540523132 ) ) ;
#7870 = CARTESIAN_POINT ( 'NONE',  ( 146.8988248654052313, 3.889087296526011706, 3.889087296526011706 ) ) ;
#7871 = CARTESIAN_POINT ( 'NONE',  ( -3.175426480542816066, -5.500000000000057732, -72.87500000000000000 ) ) ;
#7872 = CARTESIAN_POINT ( 'NONE',  ( -3.464101615137725076, 5.999999999999979572, -85.66367513459481131 ) ) ;
#7873 = CARTESIAN_POINT ( 'NONE',  ( -4.763139720814407951, -2.750000000000016431, -56.49999999999999289 ) ) ;
#7874 = FACE_OUTER_BOUND ( 'NONE', #2903, .T. ) ;
#7875 = ORIENTED_EDGE ( 'NONE', *, *, #127, .T. ) ;
#7876 = CARTESIAN_POINT ( 'NONE',  ( 141.9523502691896510, 0.000000000000000000, 5.000000000000004441 ) ) ;
#7877 = CARTESIAN_POINT ( 'NONE',  ( 149.1562500000000568, -6.000000000000005329, 2.485281374238556218 ) ) ;
#7878 = CARTESIAN_POINT ( 'NONE',  ( -3.464101615137725076, 5.999999999999979572, -97.66367513459481131 ) ) ;
#7879 = CARTESIAN_POINT ( 'NONE',  ( 16.06250000000006040, 2.000000000000151879, 0.8284271247461152399 ) ) ;
#7880 = DIRECTION ( 'NONE',  ( 5.551115123125785167E-17, -1.000000000000000000, -8.881784197001256268E-16 ) ) ;
#7881 = CARTESIAN_POINT ( 'NONE',  ( 114.5622167782375556, 1.849990392679682127, -0.7662911109076485650 ) ) ;
#7882 = EDGE_CURVE ( 'NONE', #12140, #26257, #25236, .T. ) ;
#7883 = ORIENTED_EDGE ( 'NONE', *, *, #14386, .T. ) ;
#7884 = CARTESIAN_POINT ( 'NONE',  ( 146.6250000000000284, 0.000000000000000000, -6.000000000000005329 ) ) ;
#7885 = CARTESIAN_POINT ( 'NONE',  ( -5.196152422706573404, -3.000000000000002665, -122.2113248654052029 ) ) ;
#7886 = CARTESIAN_POINT ( 'NONE',  ( 0.000000000000000000, -5.999999999999991118, -102.4613248654052171 ) ) ;
#7887 = CARTESIAN_POINT ( 'NONE',  ( 0.000000000000000000, 5.499999999999991118, -180.0000000000000568 ) ) ;
#7888 = CARTESIAN_POINT ( 'NONE',  ( 18.56250000000004974, -1.999999999999971800, -0.8284271247462354770 ) ) ;
#7889 = CARTESIAN_POINT ( 'NONE',  ( -5.412658773652739619, 3.124999999999975131, -149.3169872981078186 ) ) ;
#7890 = SURFACE_STYLE_FILL_AREA ( #10227 ) ;
#7891 = CARTESIAN_POINT ( 'NONE',  ( -3.175426480542816510, -5.500000000000057732, -83.37500000000004263 ) ) ;
#7892 = MECHANICAL_DESIGN_GEOMETRIC_PRESENTATION_REPRESENTATION (  '', ( #9878 ), #9390 ) ;
#7893 = CARTESIAN_POINT ( 'NONE',  ( -3.608439182435052128, -6.250000000000110134, -94.30801270189219565 ) ) ;
#7894 = STYLED_ITEM ( 'NONE', ( #22869 ), #12368 ) ;
#7895 = CARTESIAN_POINT ( 'NONE',  ( 3.464101615137757051, -5.999999999999979572, -127.8363248654051887 ) ) ;
#7896 = SURFACE_STYLE_USAGE ( .BOTH. , #18597 ) ;
#7897 = CARTESIAN_POINT ( 'NONE',  ( 3.973952007372695494, -10.26128916632342047, -20.48836482813348070 ) ) ;
#7898 = CARTESIAN_POINT ( 'NONE',  ( 5.196152422706629359, -2.999999999999988898, -58.71132486540520290 ) ) ;
#7899 =( LENGTH_UNIT ( ) NAMED_UNIT ( * ) SI_UNIT ( .MILLI., .METRE. ) );
#7900 = CARTESIAN_POINT ( 'NONE',  ( -4.763139720814407951, 2.749999999999946709, -167.7500000000000000 ) ) ;
#7901 = CARTESIAN_POINT ( 'NONE',  ( -4.999999999999886313, -70.00000000000001421, 7.500000000000007105 ) ) ;
#7902 = CARTESIAN_POINT ( 'NONE',  ( -4.763139720814407951, -2.750000000000016431, -145.0000000000000284 ) ) ;
#7903 = CARTESIAN_POINT ( 'NONE',  ( 0.000000000000000000, -5.999999999999991118, -52.03867513459481131 ) ) ;
#7904 = ADVANCED_FACE ( 'NONE', ( #22462 ), #1398, .T. ) ;
#7905 = CARTESIAN_POINT ( 'NONE',  ( 6.350852961086080661, -9.614813431917819062E-14, -96.37499999999997158 ) ) ;
#7906 = CARTESIAN_POINT ( 'NONE',  ( -19.99999999999998224, -54.99999999999990763, 8.000000000000007105 ) ) ;
#7907 = CARTESIAN_POINT ( 'NONE',  ( -3.175426480542816510, -5.500000000000057732, -80.37500000000002842 ) ) ;
#7908 = CARTESIAN_POINT ( 'NONE',  ( 154.2336002691896226, -4.999999999999989342, 2.071067811865468400 ) ) ;
#7909 = CARTESIAN_POINT ( 'NONE',  ( 141.5699251345948255, 2.278174593052322283, 5.499999999999701572 ) ) ;
#7910 = CARTESIAN_POINT ( 'NONE',  ( 6.000000000000000888, 1.743066579297358182E-13, -108.0863248654051745 ) ) ;
#7911 = CARTESIAN_POINT ( 'NONE',  ( 5.196152422706629359, -2.999999999999988898, -165.2113248654052313 ) ) ;
#7912 = VECTOR ( 'NONE', #23542, 1000.000000000000000 ) ;
#7913 = CARTESIAN_POINT ( 'NONE',  ( -5.999999999999963585, 1.780251999655701777E-13, -68.91367513459482552 ) ) ;
#7914 = LINE ( 'NONE', #17175, #733 ) ;
#7915 = EDGE_CURVE ( 'NONE', #13609, #6944, #12065, .T. ) ;
#7916 = ORIENTED_EDGE ( 'NONE', *, *, #22991, .T. ) ;
#7917 = CARTESIAN_POINT ( 'NONE',  ( 159.6562500000000568, -6.000000000000005329, 2.485281374238555774 ) ) ;
#7918 = PRESENTATION_STYLE_ASSIGNMENT (( #2863 ) ) ;
#7919 = B_SPLINE_CURVE_WITH_KNOTS ( 'NONE', 3,
 ( #1764, #11165, #20512, #29866, #3374, #26166, #10479, #19130, #26717, #14403 ),
 .UNSPECIFIED., .F., .F.,
 ( 4, 2, 2, 2, 4 ),
 ( 0.000000000000000000, 0.0006454309646850751002, 0.001290861929370150200, 0.001936292894055225301, 0.002581723858740300401 ),
 .UNSPECIFIED. ) ;
#7920 = ORIENTED_EDGE ( 'NONE', *, *, #1965, .F. ) ;
#7921 = ORIENTED_EDGE ( 'NONE', *, *, #4341, .F. ) ;
#7922 = CARTESIAN_POINT ( 'NONE',  ( 147.1875000000000284, 4.242640687119269671, 4.242640687119298093 ) ) ;
#7923 = CIRCLE ( 'NONE', #26586, 5.000000000000000888 ) ;
#7924 = ORIENTED_EDGE ( 'NONE', *, *, #4741, .T. ) ;
#7925 = AXIS2_PLACEMENT_3D ( 'NONE', #7123, #4817, #28308 ) ;
#7926 = CARTESIAN_POINT ( 'NONE',  ( -4.763139720814407951, -2.750000000000016431, -106.0000000000000426 ) ) ;
#7927 = CARTESIAN_POINT ( 'NONE',  ( 19.06250000000004619, -1.097466725451379244, -2.649519052838478661 ) ) ;
#7928 = CARTESIAN_POINT ( 'NONE',  ( 3.608439182435180470, -6.249999999999997335, -121.0580127018922667 ) ) ;
#7929 = ORIENTED_EDGE ( 'NONE', *, *, #26868, .T. ) ;
#7930 = CARTESIAN_POINT ( 'NONE',  ( -5.999999999999963585, 1.780251999655701777E-13, -68.91367513459482552 ) ) ;
#7931 = CARTESIAN_POINT ( 'NONE',  ( -5.412658773652684552, -3.125000000000099920, -164.0669872981078186 ) ) ;
#7932 = CARTESIAN_POINT ( 'NONE',  ( 135.0000000000000000, -7.309996799604661533, 8.297000954077597967 ) ) ;
#7933 = CARTESIAN_POINT ( 'NONE',  ( 147.1011751345948539, 3.889087296526011706, -3.889087296526011706 ) ) ;
#7934 = AXIS2_PLACEMENT_3D ( 'NONE', #4478, #20933, #18 ) ;
#7935 = CARTESIAN_POINT ( 'NONE',  ( 2.775557561562891351E-14, 6.250000000000033751, -61.93301270189222407 ) ) ;
#7936 = ORIENTED_EDGE ( 'NONE', *, *, #3016, .F. ) ;
#7937 = CARTESIAN_POINT ( 'NONE',  ( 3.464101615137852974, 5.999999999999884537, -117.4136751345948255 ) ) ;
#7938 = CARTESIAN_POINT ( 'NONE',  ( 116.1636751345946976, 1.414213562373145550, -1.414213562373145550 ) ) ;
#7939 =( BOUNDED_CURVE ( )  B_SPLINE_CURVE ( 2, ( #26776, #11781, #22814, #9446, #23128, #18679, #11480, #6972, #4359 ),
 .UNSPECIFIED., .F., .T. ) 
 B_SPLINE_CURVE_WITH_KNOTS ( ( 3, 2, 2, 2, 3 ),
 ( 0.5781250000000000000, 0.5859375000000000000, 0.5937500000000000000, 0.6015625000000000000, 0.6093750000000000000 ),
 .UNSPECIFIED. ) 
 CURVE ( )  GEOMETRIC_REPRESENTATION_ITEM ( )  RATIONAL_B_SPLINE_CURVE ( ( 1.000000000000000000, 0.9238795325112867385, 1.000000000000000000, 0.9238795325112867385, 1.000000000000000000, 0.9238795325112867385, 1.000000000000000000, 0.9238795325112867385, 1.000000000000000000 ) ) 
 REPRESENTATION_ITEM ( '' )  );
#7940 = CARTESIAN_POINT ( 'NONE',  ( -5.682342569962861134, 9.420267146893170462, -26.96534570410892684 ) ) ;
#7941 = CARTESIAN_POINT ( 'NONE',  ( 155.8988248654052313, 3.889087296526011706, 3.889087296526011706 ) ) ;
#7942 = CARTESIAN_POINT ( 'NONE',  ( 6.350852961086080661, -9.614813431917819062E-14, -171.3750000000000000 ) ) ;
#7943 = CARTESIAN_POINT ( 'NONE',  ( 120.6249999999998295, -1.767766952966376426, -1.767766952966320915 ) ) ;
#7944 = CARTESIAN_POINT ( 'NONE',  ( 19.03867513459492500, 1.110223024625156540E-13, -2.500000000000057732 ) ) ;
#7945 = CARTESIAN_POINT ( 'NONE',  ( 3.608439182435180470, -6.249999999999997335, -170.5580127018922383 ) ) ;
#7946 = CARTESIAN_POINT ( 'NONE',  ( 0.000000000000000000, 0.000000000000000000, 0.000000000000000000 ) ) ;
#7947 = EDGE_CURVE ( 'NONE', #448, #10456, #15732, .T. ) ;
#7948 = CARTESIAN_POINT ( 'NONE',  ( 24.12500000000009237, 1.414213562373201061, 1.414213562373034527 ) ) ;
#7949 = CARTESIAN_POINT ( 'NONE',  ( -4.763139720814407951, -2.750000000000016431, -113.5000000000000426 ) ) ;
#7950 = CARTESIAN_POINT ( 'NONE',  ( -3.175426480542816510, 5.499999999999865885, -107.8750000000000284 ) ) ;
#7951 = FACE_OUTER_BOUND ( 'NONE', #22339, .T. ) ;
#7952 = LINE ( 'NONE', #14749, #19451 ) ;
#7953 = ORIENTED_EDGE ( 'NONE', *, *, #29948, .T. ) ;
#7954 = CARTESIAN_POINT ( 'NONE',  ( 120.8749999999998863, 1.767766952966348670, -1.767766952966209892 ) ) ;
#7955 = CARTESIAN_POINT ( 'NONE',  ( 141.0000000000000284, -19.99999999999998934, 4.000000000000003553 ) ) ;
#7956 = EDGE_CURVE ( 'NONE', #23930, #10100, #4981, .T. ) ;
#7957 = ADVANCED_FACE ( 'NONE', ( #2759 ), #7233, .F. ) ;
#7958 = ORIENTED_EDGE ( 'NONE', *, *, #18510, .F. ) ;
#7959 = CARTESIAN_POINT ( 'NONE',  ( 21.03867513459492500, 1.665334536937734811E-13, -2.500000000000002220 ) ) ;
#7960 = CARTESIAN_POINT ( 'NONE',  ( -3.608439182435115633, 6.249999999999965361, -78.94198729810779014 ) ) ;
#7961 = CARTESIAN_POINT ( 'NONE',  ( -5.196152422706601826, 2.999999999999975131, -109.5386751345948113 ) ) ;
#7962 = ORIENTED_EDGE ( 'NONE', *, *, #6535, .F. ) ;
#7963 = FACE_OUTER_BOUND ( 'NONE', #11124, .T. ) ;
#7964 = ORIENTED_EDGE ( 'NONE', *, *, #21438, .T. ) ;
#7965 = ORIENTED_EDGE ( 'NONE', *, *, #9244, .T. ) ;
#7966 = CARTESIAN_POINT ( 'NONE',  ( 133.7961002691896795, 2.071067811865468400, -4.999999999999989342 ) ) ;
#7967 = ORIENTED_EDGE ( 'NONE', *, *, #493, .F. ) ;
#7968 = CARTESIAN_POINT ( 'NONE',  ( -7.216878364870328078, 0.000000000000000000, -132.6919872981078470 ) ) ;
#7969 = CARTESIAN_POINT ( 'NONE',  ( -3.464101615137757051, -5.999999999999979572, -135.5863248654051745 ) ) ;
#7970 = CARTESIAN_POINT ( 'NONE',  ( -5.999999999999963585, -1.487416814333745711E-14, -167.9136751345948255 ) ) ;
#7971 = DIRECTION ( 'NONE',  ( -7.147005652999508048E-36, 5.642372883946980038E-36, 1.000000000000000000 ) ) ;
#7972 = ORIENTED_EDGE ( 'NONE', *, *, #26900, .F. ) ;
#7973 = CARTESIAN_POINT ( 'NONE',  ( 15.68750000000012612, -0.8284271247459350507, -2.000000000000031530 ) ) ;
#7974 = CARTESIAN_POINT ( 'NONE',  ( 0.1285875681788154201, -16.20696777277755984, -6.610703565164271822 ) ) ;
#7975 = CARTESIAN_POINT ( 'NONE',  ( 24.50000000000010658, 5.545910952697852281E-14, 2.499999999999943601 ) ) ;
#7976 = DIRECTION ( 'NONE',  ( -7.147005652999508048E-36, 5.642372883946980038E-36, 1.000000000000000000 ) ) ;
#7977 = CARTESIAN_POINT ( 'NONE',  ( 140.2351497308104058, 3.535533905932725318, -3.535533905932725318 ) ) ;
#7978 = DIRECTION ( 'NONE',  ( 1.000000000000000000, -5.551115123125773458E-17, -1.260129944081490338E-35 ) ) ;
#7979 = CARTESIAN_POINT ( 'NONE',  ( 13.85117513459488947, -2.499999999999904521, -1.035533905932749299 ) ) ;
#7980 = CARTESIAN_POINT ( 'NONE',  ( -5.412658773652739619, 3.124999999999975131, -68.31698729810781856 ) ) ;
#7981 = CARTESIAN_POINT ( 'NONE',  ( -5.412658773652739619, 3.124999999999975131, -53.31698729810785409 ) ) ;
#7982 = FILL_AREA_STYLE ('',( #29163 ) ) ;
#7983 = CARTESIAN_POINT ( 'NONE',  ( 6.000000000000000888, -1.859271017917181981E-14, -63.66367513459483973 ) ) ;
#7984 = CARTESIAN_POINT ( 'NONE',  ( 106.8124999999997016, 1.035533905932749299, -2.499999999999784173 ) ) ;
#7985 = EDGE_CURVE ( 'NONE', #9162, #25957, #29100, .T. ) ;
#7986 = CARTESIAN_POINT ( 'NONE',  ( 5.196152422706629359, 3.000000000000002665, -74.96132486540524553 ) ) ;
#7987 = CARTESIAN_POINT ( 'NONE',  ( 6.350852961086080661, -9.614813431917819062E-14, -126.3749999999999858 ) ) ;
#7988 = AXIS2_PLACEMENT_3D ( 'NONE', #26353, #10098, #19037 ) ;
#7989 = ORIENTED_EDGE ( 'NONE', *, *, #27252, .F. ) ;
#7990 = DIRECTION ( 'NONE',  ( 0.000000000000000000, -1.000000000000000000, -5.551115123125767911E-17 ) ) ;
#7991 =( BOUNDED_CURVE ( )  B_SPLINE_CURVE ( 2, ( #12440, #5466, #12149, #28966, #26516, #24073, #3165, #19188, #17490 ),
 .UNSPECIFIED., .F., .F. ) 
 B_SPLINE_CURVE_WITH_KNOTS ( ( 3, 2, 2, 2, 3 ),
 ( 0.3823529411764705621, 0.3897058823529411797, 0.3970588235294117418, 0.4044117647058823595, 0.4117647058823529216 ),
 .UNSPECIFIED. ) 
 CURVE ( )  GEOMETRIC_REPRESENTATION_ITEM ( )  RATIONAL_B_SPLINE_CURVE ( ( 1.000000000000000000, 0.9238795325112867385, 1.000000000000000000, 0.9238795325112867385, 1.000000000000000000, 0.9238795325112867385, 1.000000000000000000, 0.9238795325112867385, 1.000000000000000000 ) ) 
 REPRESENTATION_ITEM ( '' )  );
#7992 = CARTESIAN_POINT ( 'NONE',  ( -5.999999999999963585, 8.134310703387671600E-14, -119.3363248654052455 ) ) ;
#7993 = CARTESIAN_POINT ( 'NONE',  ( 124.9999999999999432, -70.00000000000000000, 8.000000000000007105 ) ) ;
#7994 = EDGE_CURVE ( 'NONE', #25957, #22536, #30297, .T. ) ;
#7995 = DIRECTION ( 'NONE',  ( -7.147005652999508048E-36, 5.642372883946980038E-36, 1.000000000000000000 ) ) ;
#7996 = CARTESIAN_POINT ( 'NONE',  ( 0.9868033348211117106, -16.18260772123498725, 6.670819112052090993 ) ) ;
#7997 = PRESENTATION_STYLE_ASSIGNMENT (( #21067 ) ) ;
#7998 = ORIENTED_EDGE ( 'NONE', *, *, #7607, .F. ) ;
#7999 = CARTESIAN_POINT ( 'NONE',  ( 113.4997167782376550, 1.308140751793640533, -1.308140751793640533 ) ) ;
#8000 = CARTESIAN_POINT ( 'NONE',  ( 135.2812500000000284, 2.485281374238585972, 6.000000000000005329 ) ) ;
#8001 = CARTESIAN_POINT ( 'NONE',  ( 3.608439182435180470, -6.249999999999997335, -94.69198729810779014 ) ) ;
#8002 = SURFACE_STYLE_FILL_AREA ( #22149 ) ;
#8003 = CARTESIAN_POINT ( 'NONE',  ( 10.96132486540515849, 1.110223024625156540E-13, 2.499999999999835687 ) ) ;
#8004 = CARTESIAN_POINT ( 'NONE',  ( 113.3749999999999289, -1.767766952966293159, 1.767766952966431937 ) ) ;
#8005 = FILL_AREA_STYLE ('',( #26032 ) ) ;
#8006 = DIRECTION ( 'NONE',  ( -0.000000000000000000, 0.000000000000000000, 1.000000000000000000 ) ) ;
#8007 = CARTESIAN_POINT ( 'NONE',  ( 25.06250000000014211, -1.097466725451379244, -2.649519052838419153 ) ) ;
#8008 = ORIENTED_EDGE ( 'NONE', *, *, #5647, .F. ) ;
#8009 = CARTESIAN_POINT ( 'NONE',  ( 18.53867513459497829, 1.665334536937734811E-13, 2.499999999999946709 ) ) ;
#8010 = CARTESIAN_POINT ( 'NONE',  ( 6.350852961086080661, -9.614813431917819062E-14, -54.37500000000002842 ) ) ;
#8011 = CARTESIAN_POINT ( 'NONE',  ( 136.7886751345948539, 5.500000000000005329, 0.000000000000000000 ) ) ;
#8012 = CARTESIAN_POINT ( 'NONE',  ( 6.000000000000000888, 1.743066579297358182E-13, -51.08632486540523132 ) ) ;
#8013 = CARTESIAN_POINT ( 'NONE',  ( 3.608439182435180470, 6.249999999999982236, -78.55801270189225249 ) ) ;
#8014 = DIRECTION ( 'NONE',  ( 0.000000000000000000, 0.000000000000000000, -1.000000000000000000 ) ) ;
#8015 = CARTESIAN_POINT ( 'NONE',  ( 159.0788997308104058, -4.999999999999989342, 2.071067811865468400 ) ) ;
#8016 = FACE_OUTER_BOUND ( 'NONE', #18400, .T. ) ;
#8017 = CARTESIAN_POINT ( 'NONE',  ( -5.196152422706573404, -3.000000000000002665, -152.7886751345948255 ) ) ;
#8018 = DIRECTION ( 'NONE',  ( 1.000000000000000000, -0.000000000000000000, -0.000000000000000000 ) ) ;
#8019 = EDGE_CURVE ( 'NONE', #12140, #13151, #17455, .T. ) ;
#8020 = CARTESIAN_POINT ( 'NONE',  ( 6.000000000000000888, -1.607695154586752384, -93.73066243270260145 ) ) ;
#8021 = EDGE_CURVE ( 'NONE', #886, #12287, #29285, .T. ) ;
#8022 = CARTESIAN_POINT ( 'NONE',  ( 4.763139720814407951, -2.749999999999988454, -129.5000000000000000 ) ) ;
#8023 = CYLINDRICAL_SURFACE ( 'NONE', #26751, 6.000000000000000888 ) ;
#8024 = CARTESIAN_POINT ( 'NONE',  ( -5.999999999999971578, 1.607695154586715303, -50.98066243270261566 ) ) ;
#8025 = CARTESIAN_POINT ( 'NONE',  ( 4.763139720814407951, 2.750000000000002665, -73.75000000000004263 ) ) ;
#8026 = CARTESIAN_POINT ( 'NONE',  ( 3.175426480543072749, 5.499999999999865885, -55.62500000000003553 ) ) ;
#8027 =( BOUNDED_CURVE ( )  B_SPLINE_CURVE ( 2, ( #20861, #29748, #8879, #11520, #25278, #30056, #9027, #1647, #27892 ),
 .UNSPECIFIED., .F., .T. ) 
 B_SPLINE_CURVE_WITH_KNOTS ( ( 3, 2, 2, 2, 3 ),
 ( 0.4361111111111111160, 0.4370370370370370572, 0.4388888888888888840, 0.4407407407407407662, 0.4416666666666667074 ),
 .UNSPECIFIED. ) 
 CURVE ( )  GEOMETRIC_REPRESENTATION_ITEM ( )  RATIONAL_B_SPLINE_CURVE ( ( 0.9330127018922194093, 0.9330127018922194093, 1.000000000000000000, 0.8660254037844388186, 1.000000000000000000, 0.8660254037844388186, 1.000000000000000000, 0.9330127018922174109, 0.9330127018922194093 ) ) 
 REPRESENTATION_ITEM ( '' )  );
#8028 = VERTEX_POINT ( 'NONE', #23819 ) ;
#8029 = CARTESIAN_POINT ( 'NONE',  ( 153.5625000000000568, -4.242640687119298093, 4.242640687119298093 ) ) ;
#8030 = CYLINDRICAL_SURFACE ( 'NONE', #8449, 2.000000000000012879 ) ;
#8031 = CARTESIAN_POINT ( 'NONE',  ( 14.25000000000012434, 5.551115123125782702E-14, 2.000000000000001776 ) ) ;
#8032 = CARTESIAN_POINT ( 'NONE',  ( 0.000000000000000000, -9.714451465470119729E-16, 17.50000000000004619 ) ) ;
#8033 = CARTESIAN_POINT ( 'NONE',  ( 111.8122167782374419, 0.7662911109077987781, 1.849990392679772278 ) ) ;
#8034 = ORIENTED_EDGE ( 'NONE', *, *, #23620, .T. ) ;
#8035 = CARTESIAN_POINT ( 'NONE',  ( 143.9062500000000568, 6.000000000000005329, -2.485281374238555774 ) ) ;
#8036 = CARTESIAN_POINT ( 'NONE',  ( 161.3144437930461095, -5.725702186695466267, 1.060355218292538204 ) ) ;
#8037 = CARTESIAN_POINT ( 'NONE',  ( -4.763139720814407951, -2.750000000000016431, -181.0000000000000568 ) ) ;
#8038 = CARTESIAN_POINT ( 'NONE',  ( 16.87500000000000000, 1.414213562373256572, -1.414213562373145550 ) ) ;
#8039 = VERTEX_POINT ( 'NONE', #23530 ) ;
#8040 = CARTESIAN_POINT ( 'NONE',  ( 5.412658773652712085, -3.125000000000086153, -145.5669872981077901 ) ) ;
#8041 = CARTESIAN_POINT ( 'NONE',  ( -4.763139720814407951, -2.750000000000016431, -80.50000000000001421 ) ) ;
#8042 = CARTESIAN_POINT ( 'NONE',  ( 14.75000000000004086, -1.873492889144789952, 1.873492889144845464 ) ) ;
#8043 = CARTESIAN_POINT ( 'NONE',  ( 5.412658773652712085, -3.125000000000086153, -98.43301270189225249 ) ) ;
#8044 = CARTESIAN_POINT ( 'NONE',  ( 119.9999999999998437, -0.1589013571266416347, 2.047736629975339451 ) ) ;
#8045 = COLOUR_RGB ( '', 0.09019608, 0.27058824, 0.51372549) ;
#8046 = EDGE_CURVE ( 'NONE', #371, #3222, #18426, .T. ) ;
#8047 = CARTESIAN_POINT ( 'NONE',  ( -2.775557561562891351E-14, -5.500000000000115463, -161.2500000000000000 ) ) ;
#8048 = CARTESIAN_POINT ( 'NONE',  ( 4.763139720814407951, -2.749999999999988454, -147.5000000000000284 ) ) ;
#8049 = CARTESIAN_POINT ( 'NONE',  ( -6.000000000000000888, 1.067854986875958443E-15, 7.560779664488942560E-35 ) ) ;
#8050 = CARTESIAN_POINT ( 'NONE',  ( -4.763139720814407951, -2.750000000000016431, -92.50000000000002842 ) ) ;
#8051 = DIRECTION ( 'NONE',  ( 0.000000000000000000, 0.000000000000000000, -1.000000000000000000 ) ) ;
#8052 = CARTESIAN_POINT ( 'NONE',  ( -6.350852961085760029, -1.281975124255709124E-13, -85.12499999999998579 ) ) ;
#8053 = CARTESIAN_POINT ( 'NONE',  ( 153.6711002691896510, 4.999999999999989342, 2.071067811865468400 ) ) ;
#8054 = CARTESIAN_POINT ( 'NONE',  ( 139.8141223307606822, -9.354659407854123643, -7.895782739253818683 ) ) ;
#8055 = CARTESIAN_POINT ( 'NONE',  ( 18.08632486540531659, -1.767766952966209892, 1.767766952966431937 ) ) ;
#8056 = CARTESIAN_POINT ( 'NONE',  ( 21.62500000000017053, -1.414213562372979016, -1.414213562373090038 ) ) ;
#8057 = CARTESIAN_POINT ( 'NONE',  ( 6.000000000000052403, -1.607695154586662678, -165.1533121635129646 ) ) ;
#8058 = DIRECTION ( 'NONE',  ( 0.000000000000000000, -1.000000000000000000, -8.881784197001264156E-16 ) ) ;
#8059 = CYLINDRICAL_SURFACE ( 'NONE', #20364, 6.000000000000000888 ) ;
#8060 = EDGE_LOOP ( 'NONE', ( #22863, #28351, #11971, #83 ) ) ;
#8061 = CARTESIAN_POINT ( 'NONE',  ( 161.9062500000000568, 6.000000000000005329, -2.485281374238555774 ) ) ;
#8062 = DIRECTION ( 'NONE',  ( 1.000000000000000000, -5.551115123125773458E-17, -1.260129944081490338E-35 ) ) ;
#8063 = CARTESIAN_POINT ( 'NONE',  ( 105.1872167782375556, -1.849990392679441875, -0.7662911109075883909 ) ) ;
#8064 = CARTESIAN_POINT ( 'NONE',  ( 24.84150635094622572, -1.291286745249641628E-13, -2.158493649053927044 ) ) ;
#8065 = VERTEX_POINT ( 'NONE', #25501 ) ;
#8066 = ORIENTED_EDGE ( 'NONE', *, *, #19582, .F. ) ;
#8067 = EDGE_CURVE ( 'NONE', #18315, #19006, #2472, .T. ) ;
#8068 = CARTESIAN_POINT ( 'NONE',  ( 6.350852961086080661, -9.614813431917819062E-14, -105.3750000000000142 ) ) ;
#8069 = CARTESIAN_POINT ( 'NONE',  ( 5.412658773652739619, 3.124999999999988898, -119.1830127018922383 ) ) ;
#8070 = EDGE_LOOP ( 'NONE', ( #9565, #26364, #7000, #18800 ) ) ;
#8071 = CARTESIAN_POINT ( 'NONE',  ( 3.464101615137757051, -5.999999999999979572, -110.4136751345947971 ) ) ;
#8072 = CARTESIAN_POINT ( 'NONE',  ( -3.608439182435115633, 6.249999999999965361, -156.9419872981077617 ) ) ;
#8073 = LINE ( 'NONE', #3315, #9347 ) ;
#8074 = AXIS2_PLACEMENT_3D ( 'NONE', #24648, #3595, #6360 ) ;
#8075 = CARTESIAN_POINT ( 'NONE',  ( 147.3824251345948255, 5.500000000000012434, 2.278174593052012309 ) ) ;
#8076 = AXIS2_PLACEMENT_3D ( 'NONE', #8735, #24991, #3490 ) ;
#8077 = CARTESIAN_POINT ( 'NONE',  ( 3.608439182435180470, 6.249999999999982236, -51.55801270189225249 ) ) ;
#8078 = EDGE_LOOP ( 'NONE', ( #9009, #3834, #20377, #23634 ) ) ;
#8079 = CARTESIAN_POINT ( 'NONE',  ( 0.1661021849294502251, -15.34535758500844693, -8.416596529583351582 ) ) ;
#8080 = CARTESIAN_POINT ( 'NONE',  ( -3.464101615137757051, -5.999999999999979572, -56.66367513459481131 ) ) ;
#8081 = EDGE_CURVE ( 'NONE', #28850, #25181, #1854, .T. ) ;
#8082 = CARTESIAN_POINT ( 'NONE',  ( 3.464101615137852974, 5.999999999999884537, -136.3363248654052313 ) ) ;
#8083 = CARTESIAN_POINT ( 'NONE',  ( -4.999999999999990230, -55.00000000000002132, -8.000000000000007105 ) ) ;
#8084 = CARTESIAN_POINT ( 'NONE',  ( -3.175426480542816510, -5.500000000000057732, -173.3750000000000284 ) ) ;
#8085 = CARTESIAN_POINT ( 'NONE',  ( 105.6252832217623592, 0.000000000000000000, 1.849990392679523588 ) ) ;
#8086 = CARTESIAN_POINT ( 'NONE',  ( 0.000000000000000000, 0.000000000000000000, 0.000000000000000000 ) ) ;
#8087 = CARTESIAN_POINT ( 'NONE',  ( -7.216878364870328078, 0.000000000000000000, -165.0580127018922099 ) ) ;
#8088 = CARTESIAN_POINT ( 'NONE',  ( 154.6800748654052313, -2.278174593052082475, 5.499999999999942268 ) ) ;
#8089 = CARTESIAN_POINT ( 'NONE',  ( 2.081668171172167281E-16, 3.582034040661430693E-16, -2.499999999999999112 ) ) ;
#8090 = CARTESIAN_POINT ( 'NONE',  ( 6.350852961086080661, -9.614813431917819062E-14, -115.8750000000000000 ) ) ;
#8091 =( NAMED_UNIT ( * ) PLANE_ANGLE_UNIT ( ) SI_UNIT ( $, .RADIAN. ) );
#8092 = CARTESIAN_POINT ( 'NONE',  ( 4.763139720814407951, -2.749999999999988454, -102.5000000000000284 ) ) ;
#8093 = CARTESIAN_POINT ( 'NONE',  ( 16.08632486540520645, -1.767766952966376426, 1.767766952966376426 ) ) ;
#8094 = CARTESIAN_POINT ( 'NONE',  ( 3.464101615137852974, 5.999999999999884537, -118.3363248654052171 ) ) ;
#8095 = ORIENTED_EDGE ( 'NONE', *, *, #28548, .T. ) ;
#8096 = CARTESIAN_POINT ( 'NONE',  ( 119.3124999999998437, -1.035533905932689347, 2.500000000000265121 ) ) ;
#8097 = DIRECTION ( 'NONE',  ( 1.000000000000000000, -5.551115123125773458E-17, -1.260129944081490338E-35 ) ) ;
#8098 = CARTESIAN_POINT ( 'NONE',  ( 6.000000000000103917, -1.607695154586573416, -133.6533121635129362 ) ) ;
#8099 = ORIENTED_EDGE ( 'NONE', *, *, #14576, .T. ) ;
#8100 = CARTESIAN_POINT ( 'NONE',  ( 0.000000000000000000, 5.499999999999991118, -162.0000000000000284 ) ) ;
#8101 = CIRCLE ( 'NONE', #27725, 5.500000000000000000 ) ;
#8102 = CARTESIAN_POINT ( 'NONE',  ( -3.608439182435115633, 6.249999999999965361, -83.44198729810781856 ) ) ;
#8103 = CARTESIAN_POINT ( 'NONE',  ( 0.000000000000000000, -5.999999999999991118, -97.03867513459485394 ) ) ;
#8104 = ORIENTED_EDGE ( 'NONE', *, *, #8260, .F. ) ;
#8105 = ORIENTED_EDGE ( 'NONE', *, *, #27883, .F. ) ;
#8106 = CARTESIAN_POINT ( 'NONE',  ( 160.5937500000000284, 6.000000000000005329, 2.485281374238585972 ) ) ;
#8107 = ADVANCED_FACE ( 'NONE', ( #9349 ), #30170, .T. ) ;
#8108 =( BOUNDED_CURVE ( )  B_SPLINE_CURVE ( 2, ( #14003, #7188, #21036, #7035, #4577, #2574, #14155, #11996, #16599 ),
 .UNSPECIFIED., .F., .T. ) 
 B_SPLINE_CURVE_WITH_KNOTS ( ( 3, 2, 2, 2, 3 ),
 ( 0.7027777777777777235, 0.7037037037037037202, 0.7055555555555554914, 0.7074074074074074847, 0.7083333333333333703 ),
 .UNSPECIFIED. ) 
 CURVE ( )  GEOMETRIC_REPRESENTATION_ITEM ( )  RATIONAL_B_SPLINE_CURVE ( ( 0.9330127018922194093, 0.9330127018922154125, 1.000000000000000000, 0.8660254037844388186, 1.000000000000000000, 0.8660254037844388186, 1.000000000000000000, 0.9330127018922194093, 0.9330127018922194093 ) ) 
 REPRESENTATION_ITEM ( '' )  );
#8109 = CARTESIAN_POINT ( 'NONE',  ( -3.608439182435052128, -6.250000000000110134, -137.8080127018922667 ) ) ;
#8110 = ORIENTED_EDGE ( 'NONE', *, *, #24910, .T. ) ;
#8111 = CARTESIAN_POINT ( 'NONE',  ( -3.608439182435115633, 6.249999999999965361, -129.9419872981078470 ) ) ;
#8112 = DIRECTION ( 'NONE',  ( 1.000000000000000000, 0.000000000000000000, 0.000000000000000000 ) ) ;
#8113 = CARTESIAN_POINT ( 'NONE',  ( 4.763139720814407951, -2.749999999999988454, -173.0000000000000568 ) ) ;
#8114 = VECTOR ( 'NONE', #24969, 1000.000000000000000 ) ;
#8115 = CARTESIAN_POINT ( 'NONE',  ( -5.999999999999963585, 1.780251999655701777E-13, -83.33632486540520290 ) ) ;
#8116 = CARTESIAN_POINT ( 'NONE',  ( 6.000000000000000888, -3.330669073875464691E-16, -7.560779664488942560E-35 ) ) ;
#8117 = EDGE_LOOP ( 'NONE', ( #12057, #21223, #16111, #22849 ) ) ;
#8118 = CARTESIAN_POINT ( 'NONE',  ( 13.81249999999996980, 0.8284271247461753029, -2.000000000000091926 ) ) ;
#8119 = FACE_OUTER_BOUND ( 'NONE', #4153, .T. ) ;
#8120 = EDGE_CURVE ( 'NONE', #20406, #13461, #2434, .T. ) ;
#8121 = CARTESIAN_POINT ( 'NONE',  ( 0.000000000000000000, 0.000000000000000000, 0.000000000000000000 ) ) ;
#8122 = LINE ( 'NONE', #17237, #4400 ) ;
#8123 = CARTESIAN_POINT ( 'NONE',  ( -5.196152422706573404, -3.000000000000002665, -107.7886751345948397 ) ) ;
#8124 = CARTESIAN_POINT ( 'NONE',  ( 0.7669223171414829565, -15.58766199952932396, -7.954545454545463912 ) ) ;
#8125 = CARTESIAN_POINT ( 'NONE',  ( -3.608439182435115633, 6.249999999999965361, -68.44198729810779014 ) ) ;
#8126 = CARTESIAN_POINT ( 'NONE',  ( 3.608439182435180470, -6.249999999999997335, -57.19198729810781145 ) ) ;
#8127 = FACE_OUTER_BOUND ( 'NONE', #18898, .T. ) ;
#8128 = CARTESIAN_POINT ( 'NONE',  ( 135.0000000000000284, 1.949781249179022291, 5.142796231657420947 ) ) ;
#8129 = CARTESIAN_POINT ( 'NONE',  ( 147.8511751345948255, -3.889087296526011706, 3.889087296526011706 ) ) ;
#8130 = CARTESIAN_POINT ( 'NONE',  ( -4.999999999999886313, -10.00000000000000888, 8.000000000000007105 ) ) ;
#8131 = CARTESIAN_POINT ( 'NONE',  ( -4.763139720814407951, 2.749999999999946709, -127.2500000000000284 ) ) ;
#8132 = SURFACE_STYLE_USAGE ( .BOTH. , #7832 ) ;
#8133 = CARTESIAN_POINT ( 'NONE',  ( 104.7401757384972285, -1.801236194818849778, -0.4861741747051813167 ) ) ;
#8134 = ORIENTED_EDGE ( 'NONE', *, *, #29593, .F. ) ;
#8135 = LINE ( 'NONE', #12955, #29305 ) ;
#8136 = CARTESIAN_POINT ( 'NONE',  ( 16.58632486540528816, 1.767766952966431937, -1.767766952966487448 ) ) ;
#8137 = DIRECTION ( 'NONE',  ( 0.000000000000000000, -0.9393939393939397808, -0.3428396514843859988 ) ) ;
#8138 = CARTESIAN_POINT ( 'NONE',  ( 108.5386751345947403, 5.551115123125782702E-14, 2.000000000000001776 ) ) ;
#8139 = ORIENTED_EDGE ( 'NONE', *, *, #6755, .T. ) ;
#8140 = CARTESIAN_POINT ( 'NONE',  ( 115.6247167782374561, 1.849990392679523588, 0.000000000000000000 ) ) ;
#8141 = CARTESIAN_POINT ( 'NONE',  ( 6.000000000000000888, -3.330669073875464691E-16, -7.560779664488942560E-35 ) ) ;
#8142 = CARTESIAN_POINT ( 'NONE',  ( 2.775557561562891351E-14, -6.250000000000061284, -97.81698729810783277 ) ) ;
#8143 = CARTESIAN_POINT ( 'NONE',  ( 6.000000000000000888, 1.743066579297358182E-13, -78.08632486540520290 ) ) ;
#8144 = DIRECTION ( 'NONE',  ( 0.000000000000000000, 0.000000000000000000, -1.000000000000000000 ) ) ;
#8145 = CARTESIAN_POINT ( 'NONE',  ( 115.9374999999998010, 2.500000000000054623, -1.035533905932629173 ) ) ;
#8146 = CARTESIAN_POINT ( 'NONE',  ( 140.1363996827915059, -11.13639968279144732, 4.472640761300552548 ) ) ;
#8147 = EDGE_CURVE ( 'NONE', #17914, #28360, #8108, .T. ) ;
#8148 = ORIENTED_EDGE ( 'NONE', *, *, #8340, .F. ) ;
#8149 = CARTESIAN_POINT ( 'NONE',  ( 24.87500000000017408, -2.649519052838167354, -5.551115123125782702E-14 ) ) ;
#8150 = CARTESIAN_POINT ( 'NONE',  ( -6.000000000000007105, -1.607695154586655129, -83.26933756729741276 ) ) ;
#8151 = CARTESIAN_POINT ( 'NONE',  ( 3.175426480543072749, 5.499999999999865885, -51.12500000000002132 ) ) ;
#8152 = CARTESIAN_POINT ( 'NONE',  ( 136.5074251345947971, 2.278174593051935037, -5.500000000000088818 ) ) ;
#8153 = CARTESIAN_POINT ( 'NONE',  ( -5.999999999999963585, -1.487416814333745711E-14, -59.91367513459483263 ) ) ;
#8154 = EDGE_CURVE ( 'NONE', #21664, #14180, #4454, .T. ) ;
#8155 = CARTESIAN_POINT ( 'NONE',  ( 3.608439182435180470, -6.249999999999997335, -76.05801270189223828 ) ) ;
#8156 = CARTESIAN_POINT ( 'NONE',  ( 1.000000000000000888, 0.000000000000000000, 0.000000000000000000 ) ) ;
#8157 = CARTESIAN_POINT ( 'NONE',  ( 148.2976497308104058, 0.000000000000000000, 5.000000000000004441 ) ) ;
#8158 = CARTESIAN_POINT ( 'NONE',  ( -5.999999999999963585, -2.788906526875773208E-15, -176.9136751345948539 ) ) ;
#8159 = CARTESIAN_POINT ( 'NONE',  ( -20.99177011976446394, -10.49588505988223197, -3.158490520261530689E-35 ) ) ;
#8160 = CARTESIAN_POINT ( 'NONE',  ( -2.081668171172168020E-16, -5.204170427930420051E-17, 2.499999999999999112 ) ) ;
#8161 = CARTESIAN_POINT ( 'NONE',  ( -6.000000000000000888, 1.067854986875958443E-15, 7.560779664488942560E-35 ) ) ;
#8162 =( BOUNDED_CURVE ( )  B_SPLINE_CURVE ( 2, ( #22781, #18043, #18494, #30135, #20468, #6939, #6486, #27358, #13907 ),
 .UNSPECIFIED., .F., .F. ) 
 B_SPLINE_CURVE_WITH_KNOTS ( ( 3, 2, 2, 2, 3 ),
 ( 0.8472222222222222099, 0.8481481481481480955, 0.8499999999999999778, 0.8518518518518518601, 0.8527777777777778567 ),
 .UNSPECIFIED. ) 
 CURVE ( )  GEOMETRIC_REPRESENTATION_ITEM ( )  RATIONAL_B_SPLINE_CURVE ( ( 0.9330127018922194093, 0.9330127018922194093, 1.000000000000000000, 0.8660254037844388186, 1.000000000000000000, 0.8660254037844388186, 1.000000000000000000, 0.9330127018922154125, 0.9330127018922194093 ) ) 
 REPRESENTATION_ITEM ( '' )  );
#8163 = CARTESIAN_POINT ( 'NONE',  ( 135.0000000000000284, -6.982120021884474781, 8.500000000000007105 ) ) ;
#8164 = CARTESIAN_POINT ( 'NONE',  ( -4.763139720814407951, -2.750000000000016431, -130.0000000000000000 ) ) ;
#8165 = DIRECTION ( 'NONE',  ( -0.7071067811865455743, -1.644171197757234052E-17, -0.7071067811865495711 ) ) ;
#8166 = CARTESIAN_POINT ( 'NONE',  ( -3.464101615137725076, 5.999999999999979572, -158.5863248654052313 ) ) ;
#8167 = CARTESIAN_POINT ( 'NONE',  ( -6.000000000000023093, 1.607695154586625819, -177.9033121635129930 ) ) ;
#8168 = CARTESIAN_POINT ( 'NONE',  ( 3.175426480543072749, -5.500000000000105693, -62.12500000000000711 ) ) ;
#8169 = CARTESIAN_POINT ( 'NONE',  ( 4.763139720814407951, 2.750000000000002665, -58.75000000000002132 ) ) ;
#8170 = CARTESIAN_POINT ( 'NONE',  ( -5.999999999999968026, -1.607695154586722186, -163.3466878364870070 ) ) ;
#8171 = ORIENTED_EDGE ( 'NONE', *, *, #12886, .T. ) ;
#8172 = CARTESIAN_POINT ( 'NONE',  ( 145.1250000000000284, 0.000000000000000000, -6.000000000000005329 ) ) ;
#8173 = DIRECTION ( 'NONE',  ( 0.000000000000000000, 0.000000000000000000, -1.000000000000000000 ) ) ;
#8174 = STYLED_ITEM ( 'NONE', ( #4281 ), #6354 ) ;
#8175 = CARTESIAN_POINT ( 'NONE',  ( 5.196152422706629359, -2.999999999999988898, -88.71132486540523132 ) ) ;
#8176 = CIRCLE ( 'NONE', #23902, 0.5000000000000004441 ) ;
#8177 = CARTESIAN_POINT ( 'NONE',  ( 113.4372167782374277, 0.7662911109077987781, -1.849990392679291551 ) ) ;
#8178 = AXIS2_PLACEMENT_3D ( 'NONE', #7218, #16630, #25950 ) ;
#8179 = EDGE_LOOP ( 'NONE', ( #25484, #9475, #27381, #15996, #5358, #18560, #29209, #8587, #18351, #18517, #20114, #6333, #12615, #5611, #15389, #183, #23824 ) ) ;
#8180 = CARTESIAN_POINT ( 'NONE',  ( 145.1250000000000284, 0.000000000000000000, -6.000000000000005329 ) ) ;
#8181 = PRESENTATION_LAYER_ASSIGNMENT (  '', '', ( #17548 ) ) ;
#8182 = VERTEX_POINT ( 'NONE', #28214 ) ;
#8183 = EDGE_CURVE ( 'NONE', #7068, #16950, #2229, .T. ) ;
#8184 = EDGE_CURVE ( 'NONE', #10874, #27076, #25777, .T. ) ;
#8185 = CARTESIAN_POINT ( 'NONE',  ( -6.350852961085760029, -1.281975124255709124E-13, -145.1250000000000284 ) ) ;
#8186 = CARTESIAN_POINT ( 'NONE',  ( 3.608439182435180470, 6.249999999999982236, -49.19198729810784698 ) ) ;
#8187 = CARTESIAN_POINT ( 'NONE',  ( 15.37500000000011013, -1.414213562373034527, 1.414213562373034527 ) ) ;
#8188 = VERTEX_POINT ( 'NONE', #21220 ) ;
#8189 = CARTESIAN_POINT ( 'NONE',  ( 3.608439182435180470, -6.249999999999997335, -144.1919872981078470 ) ) ;
#8190 = CARTESIAN_POINT ( 'NONE',  ( 4.763139720814407951, -2.749999999999988454, -77.00000000000001421 ) ) ;
#8191 = CARTESIAN_POINT ( 'NONE',  ( -3.608439182435052128, -6.250000000000110134, -91.30801270189225249 ) ) ;
#8192 = CYLINDRICAL_SURFACE ( 'NONE', #29986, 6.000000000000000888 ) ;
#8193 = CARTESIAN_POINT ( 'NONE',  ( 106.2738248654049187, -1.999999999999941602, -0.8284271247460553989 ) ) ;
#8194 = CARTESIAN_POINT ( 'NONE',  ( 6.000000000000000888, 1.743066579297358182E-13, -90.66367513459483973 ) ) ;
#8195 = CARTESIAN_POINT ( 'NONE',  ( 110.5386751345947403, 0.000000000000000000, 2.000000000000001776 ) ) ;
#8196 = AXIS2_PLACEMENT_3D ( 'NONE', #5050, #24244, #12180 ) ;
#8197 =( BOUNDED_CURVE ( )  B_SPLINE_CURVE ( 2, ( #2084, #28009, #9143, #2238, #20986, #25246, #21133, #30333, #9455 ),
 .UNSPECIFIED., .F., .F. ) 
 B_SPLINE_CURVE_WITH_KNOTS ( ( 3, 2, 2, 2, 3 ),
 ( 0.6916666666666666519, 0.6925925925925925375, 0.6944444444444444198, 0.6962962962962963021, 0.6972222222222222987 ),
 .UNSPECIFIED. ) 
 CURVE ( )  GEOMETRIC_REPRESENTATION_ITEM ( )  RATIONAL_B_SPLINE_CURVE ( ( 0.9330127018922194093, 0.9330127018922194093, 1.000000000000000000, 0.8660254037844388186, 1.000000000000000000, 0.8660254037844388186, 1.000000000000000000, 0.9330127018922154125, 0.9330127018922194093 ) ) 
 REPRESENTATION_ITEM ( '' )  );
#8198 = CARTESIAN_POINT ( 'NONE',  ( -2.775557561562891351E-14, -5.500000000000115463, -156.7500000000000568 ) ) ;
#8199 = CARTESIAN_POINT ( 'NONE',  ( 6.000000000000000888, -1.859271017917181981E-14, -126.6636751345948397 ) ) ;
#8200 = CARTESIAN_POINT ( 'NONE',  ( 0.000000000000000000, 5.499999999999991118, -148.5000000000000284 ) ) ;
#8201 = UNCERTAINTY_MEASURE_WITH_UNIT (LENGTH_MEASURE( 1.000000000000000082E-05 ), #28461, 'distance_accuracy_value', 'NONE');
#8202 = CARTESIAN_POINT ( 'NONE',  ( -4.763139720814407951, 2.749999999999946709, -85.25000000000004263 ) ) ;
#8203 = LINE ( 'NONE', #17619, #8579 ) ;
#8204 = CARTESIAN_POINT ( 'NONE',  ( -2.775557561562891351E-14, -5.500000000000115463, -81.74999999999998579 ) ) ;
#8205 = CARTESIAN_POINT ( 'NONE',  ( 0.000000000000000000, 0.000000000000000000, 0.000000000000000000 ) ) ;
#8206 = CARTESIAN_POINT ( 'NONE',  ( 151.0461002691896510, -2.071067811865468400, 4.999999999999989342 ) ) ;
#8207 = CARTESIAN_POINT ( 'NONE',  ( -5.196152422706601826, 2.999999999999975131, -141.9613248654052597 ) ) ;
#8208 = LINE ( 'NONE', #3904, #25824 ) ;
#8209 = VECTOR ( 'NONE', #1213, 1000.000000000000000 ) ;
#8210 = FACE_OUTER_BOUND ( 'NONE', #638, .T. ) ;
#8211 = CARTESIAN_POINT ( 'NONE',  ( 21.68750000000000711, -0.8284271247461753029, -2.000000000000031530 ) ) ;
#8212 = FACE_OUTER_BOUND ( 'NONE', #22682, .T. ) ;
#8213 = CARTESIAN_POINT ( 'NONE',  ( 150.4613248654052029, -5.500000000000005329, 0.000000000000000000 ) ) ;
#8214 = DIRECTION ( 'NONE',  ( 1.000000000000000000, -5.551115123125773458E-17, -1.260129944081490338E-35 ) ) ;
#8215 = ORIENTED_EDGE ( 'NONE', *, *, #13622, .F. ) ;
#8216 = CARTESIAN_POINT ( 'NONE',  ( 161.1562500000000284, -6.000000000000005329, 2.485281374238555774 ) ) ;
#8217 = CARTESIAN_POINT ( 'NONE',  ( -5.999999999999963585, 1.780251999655701777E-13, -72.83632486540523132 ) ) ;
#8218 = CARTESIAN_POINT ( 'NONE',  ( 5.999999999999949374, 1.607695154586804565, -81.01933756729741276 ) ) ;
#8219 =( GEOMETRIC_REPRESENTATION_CONTEXT ( 3 ) GLOBAL_UNCERTAINTY_ASSIGNED_CONTEXT ( ( #7586 ) ) GLOBAL_UNIT_ASSIGNED_CONTEXT ( ( #27666, #5192, #23257 ) ) REPRESENTATION_CONTEXT ( 'NONE', 'WORKASPACE' ) );
#8220 = CARTESIAN_POINT ( 'NONE',  ( 117.5627832217621460, 0.7662911109078588412, 1.849990392679772278 ) ) ;
#8221 = CARTESIAN_POINT ( 'NONE',  ( 143.9136751345948539, 0.000000000000000000, -5.500000000000005329 ) ) ;
#8222 = EDGE_CURVE ( 'NONE', #7154, #24608, #2653, .T. ) ;
#8223 = ORIENTED_EDGE ( 'NONE', *, *, #10770, .F. ) ;
#8224 = CARTESIAN_POINT ( 'NONE',  ( -4.763139720814407951, 2.749999999999946709, -107.7500000000000142 ) ) ;
#8225 = DIRECTION ( 'NONE',  ( 1.000000000000000000, -0.000000000000000000, -0.000000000000000000 ) ) ;
#8226 = CARTESIAN_POINT ( 'NONE',  ( -3.608439182435115633, 6.249999999999965361, -114.3080127018922525 ) ) ;
#8227 = ORIENTED_EDGE ( 'NONE', *, *, #11335, .T. ) ;
#8228 = DIRECTION ( 'NONE',  ( -7.147005652999508048E-36, 5.642372883946980038E-36, 1.000000000000000000 ) ) ;
#8229 = CARTESIAN_POINT ( 'NONE',  ( 6.000000000000000888, 1.743066579297358182E-13, -78.66367513459483973 ) ) ;
#8230 = LINE ( 'NONE', #22544, #24820 ) ;
#8231 = CARTESIAN_POINT ( 'NONE',  ( -5.412658773652684552, -3.125000000000099920, -50.93301270189220986 ) ) ;
#8232 = EDGE_LOOP ( 'NONE', ( #9194, #8134, #16194, #15894 ) ) ;
#8233 = CARTESIAN_POINT ( 'NONE',  ( 18.03867513459492145, 1.665334536937734811E-13, -2.500000000000057732 ) ) ;
#8234 = LINE ( 'NONE', #15185, #5472 ) ;
#8235 = FACE_OUTER_BOUND ( 'NONE', #20770, .T. ) ;
#8236 = CARTESIAN_POINT ( 'NONE',  ( 141.0863248654052313, 0.000000000000000000, 5.500000000000005329 ) ) ;
#8237 = CARTESIAN_POINT ( 'NONE',  ( -3.175426480542816510, 5.499999999999865885, -170.8750000000000853 ) ) ;
#8238 = CARTESIAN_POINT ( 'NONE',  ( 106.0002832217622029, -1.308140751793585022, -1.308140751793640533 ) ) ;
#8239 = CARTESIAN_POINT ( 'NONE',  ( 5.412658773652739619, 3.124999999999988898, -167.1830127018922383 ) ) ;
#8240 = CARTESIAN_POINT ( 'NONE',  ( -5.196152422706601826, 2.999999999999975131, -48.03867513459481131 ) ) ;
#8241 = CARTESIAN_POINT ( 'NONE',  ( 3.175426480543072749, -5.500000000000105693, -116.1250000000000000 ) ) ;
#8242 = CARTESIAN_POINT ( 'NONE',  ( 116.0000000000000142, 0.000000000000000000, -5.500000000000000000 ) ) ;
#8243 = CARTESIAN_POINT ( 'NONE',  ( -3.175426480542816510, 5.499999999999865885, -101.8750000000000000 ) ) ;
#8244 = CARTESIAN_POINT ( 'NONE',  ( 3.464101615137757051, -5.999999999999979572, -87.33632486540521711 ) ) ;
#8245 = CARTESIAN_POINT ( 'NONE',  ( -5.999999999999957367, 1.607695154586737507, -161.9806624327025872 ) ) ;
#8246 = CARTESIAN_POINT ( 'NONE',  ( 135.2746852666345774, -8.503752835045871095, 8.096569711865882368 ) ) ;
#8247 = VERTEX_POINT ( 'NONE', #162 ) ;
#8248 = EDGE_CURVE ( 'NONE', #16270, #28423, #23967, .T. ) ;
#8249 = CYLINDRICAL_SURFACE ( 'NONE', #16320, 6.000000000000000888 ) ;
#8250 = CARTESIAN_POINT ( 'NONE',  ( 135.3654420556978835, -8.709829393440356782, -8.045671146456855993 ) ) ;
#8251 = CARTESIAN_POINT ( 'NONE',  ( 111.2502832217621886, 1.308140751793696044, -1.308140751793640533 ) ) ;
#8252 = ORIENTED_EDGE ( 'NONE', *, *, #5344, .T. ) ;
#8253 = CARTESIAN_POINT ( 'NONE',  ( 6.350852961086080661, -9.614813431917819062E-14, -160.8750000000000284 ) ) ;
#8254 = CARTESIAN_POINT ( 'NONE',  ( 5.999999999999988454, 1.607695154586737729, -156.5966878364870638 ) ) ;
#8255 = CARTESIAN_POINT ( 'NONE',  ( 109.6247167782375840, 1.849990392679634610, 1.110223024625156540E-13 ) ) ;
#8256 = CARTESIAN_POINT ( 'NONE',  ( 7.216878364870455975, -6.409875621278545621E-14, -80.94198729810780435 ) ) ;
#8257 = CARTESIAN_POINT ( 'NONE',  ( -5.196152422706573404, -3.000000000000002665, -103.2886751345948255 ) ) ;
#8258 = ORIENTED_EDGE ( 'NONE', *, *, #21949, .F. ) ;
#8259 = CARTESIAN_POINT ( 'NONE',  ( 24.50000000000013145, 0.6095397824029125111, -2.424553825690234365 ) ) ;
#8260 = EDGE_CURVE ( 'NONE', #5962, #24536, #25432, .T. ) ;
#8261 = ORIENTED_EDGE ( 'NONE', *, *, #28821, .F. ) ;
#8262 = ORIENTED_EDGE ( 'NONE', *, *, #9151, .F. ) ;
#8263 = CARTESIAN_POINT ( 'NONE',  ( 155.6250000000000284, 0.000000000000000000, -6.000000000000005329 ) ) ;
#8264 = CARTESIAN_POINT ( 'NONE',  ( 3.175426480543072749, -5.500000000000105693, -132.6250000000000000 ) ) ;
#8265 = CARTESIAN_POINT ( 'NONE',  ( 3.608439182435180470, -6.249999999999997335, -142.0580127018922383 ) ) ;
#8266 = CARTESIAN_POINT ( 'NONE',  ( 151.4136751345948539, 0.000000000000000000, -5.500000000000005329 ) ) ;
#8267 = CARTESIAN_POINT ( 'NONE',  ( 3.608439182435180470, 6.249999999999982236, -122.6919872981078043 ) ) ;
#8268 = SURFACE_STYLE_FILL_AREA ( #8437 ) ;
#8269 = CARTESIAN_POINT ( 'NONE',  ( -3.175426480542816510, 5.499999999999865885, -173.8750000000000000 ) ) ;
#8270 = CARTESIAN_POINT ( 'NONE',  ( 5.196152422706629359, 3.000000000000002665, -175.4613248654052313 ) ) ;
#8271 =( NAMED_UNIT ( * ) SI_UNIT ( $, .STERADIAN. ) SOLID_ANGLE_UNIT ( ) );
#8272 = EDGE_LOOP ( 'NONE', ( #12136, #4235, #20762, #8930 ) ) ;
#8273 = CARTESIAN_POINT ( 'NONE',  ( 16.56250000000011369, -1.999999999999911626, -0.8284271247462354770 ) ) ;
#8274 = CARTESIAN_POINT ( 'NONE',  ( 0.2150838311359447030, -15.80975343865253713, -7.511900204273787907 ) ) ;
#8275 = CARTESIAN_POINT ( 'NONE',  ( -3.464101615137725076, 5.999999999999979572, -163.6636751345947971 ) ) ;
#8276 = CARTESIAN_POINT ( 'NONE',  ( 5.196152422706629359, 3.000000000000002665, -56.96132486540522422 ) ) ;
#8277 = CARTESIAN_POINT ( 'NONE',  ( 159.2681041991610016, -11.07692307732762771, -4.615384614413698294 ) ) ;
#8278 = CARTESIAN_POINT ( 'NONE',  ( 3.464101615137852974, 5.999999999999884537, -171.4136751345948255 ) ) ;
#8279 = CARTESIAN_POINT ( 'NONE',  ( 6.000000000000000888, 1.607695154586715303, -46.51933756729744118 ) ) ;
#8280 = CARTESIAN_POINT ( 'NONE',  ( 115.8752832217622313, -1.849990392679468076, 1.110223024625156540E-13 ) ) ;
#8281 = CARTESIAN_POINT ( 'NONE',  ( -7.216878364870328078, 0.000000000000000000, -65.19198729810777593 ) ) ;
#8282 = CARTESIAN_POINT ( 'NONE',  ( -7.216878364870328078, 0.000000000000000000, -56.19198729810781145 ) ) ;
#8283 = CARTESIAN_POINT ( 'NONE',  ( 3.464101615137757051, -5.999999999999979572, -170.4136751345948255 ) ) ;
#8284 = DIRECTION ( 'NONE',  ( -7.147005652999508048E-36, 5.642372883946980038E-36, 1.000000000000000000 ) ) ;
#8285 = CARTESIAN_POINT ( 'NONE',  ( 119.9999999999998437, 0.3537249946064329187, -2.089338094882287056 ) ) ;
#8286 = CARTESIAN_POINT ( 'NONE',  ( -4.999999999999886313, -9.000000000000007105, -4.000000000000003553 ) ) ;
#8287 = CARTESIAN_POINT ( 'NONE',  ( 3.175426480543072749, -5.500000000000105693, -131.1250000000000000 ) ) ;
#8288 = EDGE_CURVE ( 'NONE', #13246, #8435, #16079, .T. ) ;
#8289 = ORIENTED_EDGE ( 'NONE', *, *, #11444, .T. ) ;
#8290 = CARTESIAN_POINT ( 'NONE',  ( 24.06250000000009592, -2.649519052838178457, 1.097466725451439196 ) ) ;
#8291 = ADVANCED_FACE ( 'NONE', ( #26252 ), #7228, .T. ) ;
#8292 = AXIS2_PLACEMENT_3D ( 'NONE', #133, #9199, #27761 ) ;
#8293 = DIRECTION ( 'NONE',  ( 1.000000000000000000, 0.000000000000000000, 1.734723475976807094E-15 ) ) ;
#8294 = CARTESIAN_POINT ( 'NONE',  ( 2.081668171172167281E-16, 3.582034040661430693E-16, -2.499999999999999112 ) ) ;
#8295 = CARTESIAN_POINT ( 'NONE',  ( 0.000000000000000000, -5.999999999999991118, -161.5386751345948539 ) ) ;
#8296 =( BOUNDED_CURVE ( )  B_SPLINE_CURVE ( 2, ( #21243, #9568, #478, #23844, #19101, #4492, #23407, #2200, #16665 ),
 .UNSPECIFIED., .F., .F. ) 
 B_SPLINE_CURVE_WITH_KNOTS ( ( 3, 2, 2, 2, 3 ),
 ( 0.1194444444444444642, 0.1203703703703703498, 0.1222222222222222321, 0.1240740740740741144, 0.1250000000000000000 ),
 .UNSPECIFIED. ) 
 CURVE ( )  GEOMETRIC_REPRESENTATION_ITEM ( )  RATIONAL_B_SPLINE_CURVE ( ( 0.9330127018922194093, 0.9330127018922234061, 1.000000000000000000, 0.8660254037844388186, 1.000000000000000000, 0.8660254037844388186, 1.000000000000000000, 0.9330127018922194093, 0.9330127018922194093 ) ) 
 REPRESENTATION_ITEM ( '' )  );
#8297 = FACE_OUTER_BOUND ( 'NONE', #24817, .T. ) ;
#8298 = ORIENTED_EDGE ( 'NONE', *, *, #17909, .T. ) ;
#8299 = CARTESIAN_POINT ( 'NONE',  ( 115.3747167782374987, -5.551115123125782702E-14, -1.849990392679523588 ) ) ;
#8300 = CARTESIAN_POINT ( 'NONE',  ( 10.85117513459490013, -2.499999999999844569, -1.035533905932749299 ) ) ;
#8301 = CARTESIAN_POINT ( 'NONE',  ( 5.412658773652712085, -3.125000000000086153, -115.5669872981078328 ) ) ;
#8302 = CARTESIAN_POINT ( 'NONE',  ( 19.60117513459486815, -1.035533905932629173, 2.500000000000024425 ) ) ;
#8303 = EDGE_CURVE ( 'NONE', #5729, #7007, #22313, .T. ) ;
#8304 =( BOUNDED_CURVE ( )  B_SPLINE_CURVE ( 2, ( #26146, #4948, #21113, #2799, #48, #21412, #21564, #18819, #16973 ),
 .UNSPECIFIED., .F., .T. ) 
 B_SPLINE_CURVE_WITH_KNOTS ( ( 3, 2, 2, 2, 3 ),
 ( 0.2583333333333333037, 0.2592592592592593004, 0.2611111111111110716, 0.2629629629629629539, 0.2638888888888889506 ),
 .UNSPECIFIED. ) 
 CURVE ( )  GEOMETRIC_REPRESENTATION_ITEM ( )  RATIONAL_B_SPLINE_CURVE ( ( 0.9330127018922194093, 0.9330127018922154125, 1.000000000000000000, 0.8660254037844388186, 1.000000000000000000, 0.8660254037844388186, 1.000000000000000000, 0.9330127018922154125, 0.9330127018922194093 ) ) 
 REPRESENTATION_ITEM ( '' )  );
#8305 = DIRECTION ( 'NONE',  ( -1.734723475976824844E-16, 1.000000000000000000, -0.000000000000000000 ) ) ;
#8306 = CARTESIAN_POINT ( 'NONE',  ( 114.6249999999999574, -1.767766952966431937, -1.767766952966431937 ) ) ;
#8307 = CARTESIAN_POINT ( 'NONE',  ( 159.0723610732460713, -12.00000000000000888, 4.000000000000001776 ) ) ;
#8308 = CARTESIAN_POINT ( 'NONE',  ( 143.9062500000000568, 6.000000000000005329, -2.485281374238555774 ) ) ;
#8309 = ORIENTED_EDGE ( 'NONE', *, *, #21885, .F. ) ;
#8310 = CARTESIAN_POINT ( 'NONE',  ( 24.50000000000015987, 1.873492889145123019, 1.873492889144734441 ) ) ;
#8311 = CARTESIAN_POINT ( 'NONE',  ( 136.1175748654052313, 5.500000000000012434, -2.278174593052012309 ) ) ;
#8312 = CARTESIAN_POINT ( 'NONE',  ( 3.175426480543072749, -5.500000000000105693, -51.62500000000001421 ) ) ;
#8313 = VECTOR ( 'NONE', #774, 1000.000000000000000 ) ;
#8314 = CARTESIAN_POINT ( 'NONE',  ( 140.7261751345948539, -3.889087296526011706, -3.889087296526011706 ) ) ;
#8315 = CARTESIAN_POINT ( 'NONE',  ( 136.1324251345948539, -5.500000000000012434, -2.278174593052012309 ) ) ;
#8316 = CARTESIAN_POINT ( 'NONE',  ( 5.412658773652712085, -3.125000000000086153, -72.93301270189222407 ) ) ;
#8317 = CARTESIAN_POINT ( 'NONE',  ( 136.0000000000000284, -8.946933499675704837, -8.000000000000007105 ) ) ;
#8318 = CARTESIAN_POINT ( 'NONE',  ( 151.6726497308104058, -5.000000000000004441, 0.000000000000000000 ) ) ;
#8319 = CYLINDRICAL_SURFACE ( 'NONE', #8432, 6.000000000000000888 ) ;
#8320 = CARTESIAN_POINT ( 'NONE',  ( 6.000000000000000888, 7.762456499804235646E-14, -118.5863248654052313 ) ) ;
#8321 = CIRCLE ( 'NONE', #12297, 2.000000000000012879 ) ;
#8322 = CARTESIAN_POINT ( 'NONE',  ( 24.53656071872807232, -0.3046082907918452598, 2.449202433447952743 ) ) ;
#8323 = CARTESIAN_POINT ( 'NONE',  ( 135.3281957118843479, -8.627452770990513997, 8.066272317427783278 ) ) ;
#8324 = CARTESIAN_POINT ( 'NONE',  ( -4.763139720814407951, -2.750000000000016431, -136.0000000000000000 ) ) ;
#8325 = CARTESIAN_POINT ( 'NONE',  ( -5.999999999999963585, 1.780251999655701777E-13, -74.91367513459485394 ) ) ;
#8326 = DIRECTION ( 'NONE',  ( -8.326672684688675286E-17, -2.081668171172168821E-17, 1.000000000000000000 ) ) ;
#8327 = VERTEX_POINT ( 'NONE', #2610 ) ;
#8328 = EDGE_CURVE ( 'NONE', #7517, #4859, #1670, .T. ) ;
#8329 = CARTESIAN_POINT ( 'NONE',  ( -4.763139720814407951, -2.750000000000016431, -59.50000000000000000 ) ) ;
#8330 = CARTESIAN_POINT ( 'NONE',  ( -4.763139720814407951, 2.749999999999946709, -55.25000000000002132 ) ) ;
#8331 = FILL_AREA_STYLE ('',( #24611 ) ) ;
#8332 = ORIENTED_EDGE ( 'NONE', *, *, #4836, .T. ) ;
#8333 = CARTESIAN_POINT ( 'NONE',  ( 110.3749999999999289, -1.767766952966209892, 1.767766952966542959 ) ) ;
#8334 = CARTESIAN_POINT ( 'NONE',  ( 146.9062500000000568, 6.000000000000005329, -2.485281374238556218 ) ) ;
#8335 = DIRECTION ( 'NONE',  ( -7.147005652999508048E-36, 5.642372883946980038E-36, 1.000000000000000000 ) ) ;
#8336 = CARTESIAN_POINT ( 'NONE',  ( 15.68750000000012612, -0.8284271247459350507, -2.000000000000031530 ) ) ;
#8337 =( GEOMETRIC_REPRESENTATION_CONTEXT ( 3 ) GLOBAL_UNCERTAINTY_ASSIGNED_CONTEXT ( ( #28383 ) ) GLOBAL_UNIT_ASSIGNED_CONTEXT ( ( #314, #7, #17081 ) ) REPRESENTATION_CONTEXT ( 'NONE', 'WORKASPACE' ) );
#8338 = FILL_AREA_STYLE_COLOUR ( '', #4774 ) ;
#8339 = CARTESIAN_POINT ( 'NONE',  ( 110.5622167782373992, 1.849990392679501827, -0.7662911109077087390 ) ) ;
#8340 = EDGE_CURVE ( 'NONE', #1935, #27983, #6168, .T. ) ;
#8341 = EDGE_CURVE ( 'NONE', #14551, #11262, #24442, .T. ) ;
#8342 = ORIENTED_EDGE ( 'NONE', *, *, #1254, .F. ) ;
#8343 = CARTESIAN_POINT ( 'NONE',  ( 143.2500000000000568, -6.000000000000005329, 0.000000000000000000 ) ) ;
#8344 = CARTESIAN_POINT ( 'NONE',  ( 161.4835765834562267, -3.531227715922129917, -4.872661563383335448 ) ) ;
#8345 = ORIENTED_EDGE ( 'NONE', *, *, #13078, .F. ) ;
#8346 = CARTESIAN_POINT ( 'NONE',  ( 3.175426480543072749, -5.500000000000105693, -143.1250000000000000 ) ) ;
#8347 = CARTESIAN_POINT ( 'NONE',  ( 5.412658773652739619, 3.124999999999988898, -47.81698729810779014 ) ) ;
#8348 = CARTESIAN_POINT ( 'NONE',  ( 18.68750000000004974, -0.8284271247461753029, -1.999999999999971800 ) ) ;
#8349 = EDGE_LOOP ( 'NONE', ( #19526, #3190, #28586 ) ) ;
#8350 = CARTESIAN_POINT ( 'NONE',  ( -5.412658773652684552, -3.125000000000099920, -146.0669872981078470 ) ) ;
#8351 = CARTESIAN_POINT ( 'NONE',  ( -2.775557561562891351E-14, -5.500000000000115463, -72.75000000000004263 ) ) ;
#8352 = CARTESIAN_POINT ( 'NONE',  ( 12.93750000000004086, -2.649519052838298805, -1.097466725451559322 ) ) ;
#8353 = CARTESIAN_POINT ( 'NONE',  ( 2.775557561562891351E-14, 6.250000000000033751, -97.93301270189225249 ) ) ;
#8354 = ORIENTED_EDGE ( 'NONE', *, *, #15196, .T. ) ;
#8355 = CARTESIAN_POINT ( 'NONE',  ( -3.175426480542816510, -5.500000000000057732, -152.3750000000000000 ) ) ;
#8356 = CARTESIAN_POINT ( 'NONE',  ( -4.763867271839550277, -9.917884865257443394, -21.33175192690178079 ) ) ;
#8357 = LINE ( 'NONE', #24188, #9325 ) ;
#8358 = CYLINDRICAL_SURFACE ( 'NONE', #16543, 1.000000000000000888 ) ;
#8359 = CIRCLE ( 'NONE', #508, 0.5000000000000004441 ) ;
#8360 = CARTESIAN_POINT ( 'NONE',  ( 3.464101615137757051, -5.999999999999979572, -90.91367513459485394 ) ) ;
#8361 = DIRECTION ( 'NONE',  ( -7.147005652999508048E-36, 5.642372883946980038E-36, 1.000000000000000000 ) ) ;
#8362 = DIRECTION ( 'NONE',  ( 0.7304298117691189196, 0.6274463451496932187, 0.2697839395464846635 ) ) ;
#8363 = CARTESIAN_POINT ( 'NONE',  ( 3.175426480543072749, -5.500000000000105693, -155.1249999999999716 ) ) ;
#8364 = DIRECTION ( 'NONE',  ( 1.000000000000000000, -5.551115123125774074E-17, 0.000000000000000000 ) ) ;
#8365 = CARTESIAN_POINT ( 'NONE',  ( -4.763139720814407951, -2.750000000000016431, -149.5000000000000284 ) ) ;
#8366 = CARTESIAN_POINT ( 'NONE',  ( 156.4613248654052029, -5.500000000000005329, 0.000000000000000000 ) ) ;
#8367 = EDGE_CURVE ( 'NONE', #23217, #19618, #23397, .T. ) ;
#8368 = CARTESIAN_POINT ( 'NONE',  ( 3.175426480543072749, -5.500000000000105693, -87.62500000000000000 ) ) ;
#8369 = CYLINDRICAL_SURFACE ( 'NONE', #28605, 6.000000000000000888 ) ;
#8370 = CARTESIAN_POINT ( 'NONE',  ( 5.196152422706629359, -2.999999999999988898, -130.7113248654052597 ) ) ;
#8371 = CARTESIAN_POINT ( 'NONE',  ( -4.763139720814407951, -2.750000000000016431, -80.50000000000001421 ) ) ;
#8372 = CARTESIAN_POINT ( 'NONE',  ( 6.000000000000000888, -1.859271017917181981E-14, -120.0863248654052313 ) ) ;
#8373 = CARTESIAN_POINT ( 'NONE',  ( 152.7336002691896510, -4.999999999999989342, 2.071067811865468400 ) ) ;
#8374 = CARTESIAN_POINT ( 'NONE',  ( -5.999999999999971578, 1.607695154586715303, -141.9033121635129930 ) ) ;
#8375 = CARTESIAN_POINT ( 'NONE',  ( -20.99999999999998224, -19.99999999999998934, 5.000000000000004441 ) ) ;
#8376 = CARTESIAN_POINT ( 'NONE',  ( 135.1949251345948539, 5.500000000000012434, -2.278174593052012309 ) ) ;
#8377 = CARTESIAN_POINT ( 'NONE',  ( 6.000000000000000888, 1.607695154586715303, -125.0966878364870354 ) ) ;
#8378 = CARTESIAN_POINT ( 'NONE',  ( 120.1872167782373992, -1.849990392679441875, -0.7662911109076485650 ) ) ;
#8379 = ADVANCED_FACE ( 'NONE', ( #7963 ), #26835, .T. ) ;
#8380 = CYLINDRICAL_SURFACE ( 'NONE', #23838, 0.5000000000000004441 ) ;
#8381 = ORIENTED_EDGE ( 'NONE', *, *, #12516, .T. ) ;
#8382 = CARTESIAN_POINT ( 'NONE',  ( 160.3125000000000284, 4.242640687119298093, -4.242640687119298093 ) ) ;
#8383 = CARTESIAN_POINT ( 'NONE',  ( 6.000000000000000888, 1.743066579297358182E-13, -70.58632486540521711 ) ) ;
#8384 = CARTESIAN_POINT ( 'NONE',  ( 145.6949251345948255, 5.500000000000012434, -2.278174593052012309 ) ) ;
#8385 = CARTESIAN_POINT ( 'NONE',  ( 118.6252832217622029, 5.551115123125782702E-14, 1.849990392679634610 ) ) ;
#8386 = CIRCLE ( 'NONE', #4469, 5.000000000000004441 ) ;
#8387 = UNCERTAINTY_MEASURE_WITH_UNIT (LENGTH_MEASURE( 1.000000000000000082E-05 ), #22279, 'distance_accuracy_value', 'NONE');
#8388 = ORIENTED_EDGE ( 'NONE', *, *, #13236, .T. ) ;
#8389 = CARTESIAN_POINT ( 'NONE',  ( 6.350852961086080661, -9.614813431917819062E-14, -97.87499999999998579 ) ) ;
#8390 = CARTESIAN_POINT ( 'NONE',  ( 5.999999999999949374, 1.607695154586804565, -71.09668783648703538 ) ) ;
#8391 =( BOUNDED_CURVE ( )  B_SPLINE_CURVE ( 2, ( #17701, #26864, #17547, #21985, #19539, #10471, #1218, #15242, #29331 ),
 .UNSPECIFIED., .F., .F. ) 
 B_SPLINE_CURVE_WITH_KNOTS ( ( 3, 2, 2, 2, 3 ),
 ( 0.1083333333333333370, 0.1092592592592592643, 0.1111111111111111049, 0.1129629629629629595, 0.1138888888888888867 ),
 .UNSPECIFIED. ) 
 CURVE ( )  GEOMETRIC_REPRESENTATION_ITEM ( )  RATIONAL_B_SPLINE_CURVE ( ( 0.9330127018922194093, 0.9330127018922194093, 1.000000000000000000, 0.8660254037844388186, 1.000000000000000000, 0.8660254037844388186, 1.000000000000000000, 0.9330127018922194093, 0.9330127018922194093 ) ) 
 REPRESENTATION_ITEM ( '' )  );
#8392 = CARTESIAN_POINT ( 'NONE',  ( 7.216878364870455975, -6.409875621278545621E-14, -114.8080127018922383 ) ) ;
#8393 = ORIENTED_EDGE ( 'NONE', *, *, #7210, .F. ) ;
#8394 = CARTESIAN_POINT ( 'NONE',  ( -5.196152422706601826, 2.999999999999975131, -93.96132486540520290 ) ) ;
#8395 = CARTESIAN_POINT ( 'NONE',  ( 135.0000000000000568, -8.296129373581107913, 7.693241659069887994 ) ) ;
#8396 = VECTOR ( 'NONE', #22477, 1000.000000000000000 ) ;
#8397 = CARTESIAN_POINT ( 'NONE',  ( 6.000000000000000888, 1.607695154586715303, -63.59668783648704959 ) ) ;
#8398 = CARTESIAN_POINT ( 'NONE',  ( 3.608439182435180470, 6.249999999999982236, -54.55801270189220276 ) ) ;
#8399 = ORIENTED_EDGE ( 'NONE', *, *, #13249, .T. ) ;
#8400 = CARTESIAN_POINT ( 'NONE',  ( 115.8511751345946976, -1.999999999999971800, -0.8284271247459350507 ) ) ;
#8401 = CARTESIAN_POINT ( 'NONE',  ( -6.000000000000007105, -1.607695154586655129, -167.2693375672974128 ) ) ;
#8402 = CARTESIAN_POINT ( 'NONE',  ( 155.3363248654052313, 0.000000000000000000, -5.500000000000005329 ) ) ;
#8403 = CARTESIAN_POINT ( 'NONE',  ( -3.175426480542816510, 5.499999999999865885, -172.3750000000000000 ) ) ;
#8404 = CARTESIAN_POINT ( 'NONE',  ( 115.6249999999998295, -1.767766952966376426, -1.767766952966320915 ) ) ;
#8405 = CARTESIAN_POINT ( 'NONE',  ( -6.000000000000007105, -1.607695154586655129, -158.2693375672974128 ) ) ;
#8406 = CARTESIAN_POINT ( 'NONE',  ( 2.775557561562891351E-14, -6.250000000000061284, -158.6830127018922099 ) ) ;
#8407 = CARTESIAN_POINT ( 'NONE',  ( 6.000000000000000888, 1.743066579297358182E-13, -82.58632486540520290 ) ) ;
#8408 = EDGE_CURVE ( 'NONE', #18931, #6372, #1354, .T. ) ;
#8409 = CARTESIAN_POINT ( 'NONE',  ( -4.763139720814407951, -2.750000000000016431, -107.5000000000000426 ) ) ;
#8410 = CARTESIAN_POINT ( 'NONE',  ( 106.1488248654049187, -2.000000000000001776, 0.8284271247463557142 ) ) ;
#8411 = EDGE_CURVE ( 'NONE', #16120, #20574, #6121, .T. ) ;
#8412 = CARTESIAN_POINT ( 'NONE',  ( -4.763139720814407951, 2.749999999999946709, -104.7500000000000142 ) ) ;
#8413 = CYLINDRICAL_SURFACE ( 'NONE', #27260, 5.500000000000000000 ) ;
#8414 = CARTESIAN_POINT ( 'NONE',  ( 141.1949251345947971, 5.500000000000012434, -2.278174593052012309 ) ) ;
#8415 = CARTESIAN_POINT ( 'NONE',  ( 135.0968198485644791, -7.962041090232468754, 8.242705641925590854 ) ) ;
#8416 = VECTOR ( 'NONE', #7656, 1000.000000000000000 ) ;
#8417 = ORIENTED_EDGE ( 'NONE', *, *, #3365, .T. ) ;
#8418 = CARTESIAN_POINT ( 'NONE',  ( 15.50000000000018119, 1.873492889145123019, -1.873492889144956486 ) ) ;
#8419 = CARTESIAN_POINT ( 'NONE',  ( -6.000000000000007105, -1.607695154586655129, -90.76933756729744118 ) ) ;
#8420 = CARTESIAN_POINT ( 'NONE',  ( 109.8752832217622739, -1.849990392679468076, 1.110223024625156540E-13 ) ) ;
#8421 = CARTESIAN_POINT ( 'NONE',  ( 5.196152422706629359, -2.999999999999988898, -133.7113248654052029 ) ) ;
#8422 = ORIENTED_EDGE ( 'NONE', *, *, #29593, .T. ) ;
#8423 = CARTESIAN_POINT ( 'NONE',  ( 139.5863248654052313, 0.000000000000000000, 5.500000000000005329 ) ) ;
#8424 = CIRCLE ( 'NONE', #25598, 6.000000000000001776 ) ;
#8425 = CARTESIAN_POINT ( 'NONE',  ( -7.216878364870328078, 0.000000000000000000, -81.69198729810780435 ) ) ;
#8426 = CARTESIAN_POINT ( 'NONE',  ( 5.196152422706629359, -2.999999999999988898, -96.78867513459482552 ) ) ;
#8427 = EDGE_LOOP ( 'NONE', ( #9612, #10601, #16608, #26000 ) ) ;
#8428 = CARTESIAN_POINT ( 'NONE',  ( 6.000000000000000888, 7.762456499804234384E-14, -144.6636751345948255 ) ) ;
#8429 = ORIENTED_EDGE ( 'NONE', *, *, #27593, .T. ) ;
#8430 = EDGE_LOOP ( 'NONE', ( #28534, #11001, #4269, #26823 ) ) ;
#8431 = CARTESIAN_POINT ( 'NONE',  ( 157.0312500000000853, -2.485281374238555774, -6.000000000000005329 ) ) ;
#8432 = AXIS2_PLACEMENT_3D ( 'NONE', #3856, #17890, #15593 ) ;
#8433 = CARTESIAN_POINT ( 'NONE',  ( -6.350852961085760029, -1.281975124255709124E-13, -121.1250000000000426 ) ) ;
#8434 = CARTESIAN_POINT ( 'NONE',  ( 3.608439182435180470, 6.249999999999982236, -135.5580127018922667 ) ) ;
#8435 = VERTEX_POINT ( 'NONE', #29455 ) ;
#8436 = CARTESIAN_POINT ( 'NONE',  ( -3.608439182435115633, 6.249999999999965361, -126.9419872981078328 ) ) ;
#8437 = FILL_AREA_STYLE ('',( #901 ) ) ;
#8438 = CARTESIAN_POINT ( 'NONE',  ( -3.175426480542816510, -5.500000000000057732, -174.8750000000000284 ) ) ;
#8439 = CARTESIAN_POINT ( 'NONE',  ( 159.0000000000000853, -11.33333333333334281, 4.000000000000006217 ) ) ;
#8440 = CARTESIAN_POINT ( 'NONE',  ( 107.6636751345946692, -1.414213562373173305, 1.414213562373145550 ) ) ;
#8441 = VERTEX_POINT ( 'NONE', #24402 ) ;
#8442 = CARTESIAN_POINT ( 'NONE',  ( 13.68750000000000178, -0.8284271247459350507, -2.000000000000091926 ) ) ;
#8443 = CARTESIAN_POINT ( 'NONE',  ( -0.08077072505711925532, -15.22017114206482269, -7.626010301205228714 ) ) ;
#8444 = CARTESIAN_POINT ( 'NONE',  ( 6.000000000000000888, 7.762456499804234384E-14, -138.6636751345948255 ) ) ;
#8445 = CARTESIAN_POINT ( 'NONE',  ( 140.0550748654052597, -5.500000000000012434, -2.278174593052012309 ) ) ;
#8446 = CARTESIAN_POINT ( 'NONE',  ( 0.7509536901451536739, -15.55282566733050942, -8.022540739038966251 ) ) ;
#8447 = CARTESIAN_POINT ( 'NONE',  ( 117.0002832217621602, -1.308140751793557266, -1.308140751793529510 ) ) ;
#8448 = CARTESIAN_POINT ( 'NONE',  ( 3.608439182435180470, 6.249999999999982236, -67.19198729810780435 ) ) ;
#8449 = AXIS2_PLACEMENT_3D ( 'NONE', #10835, #17436, #29371 ) ;
#8450 = CARTESIAN_POINT ( 'NONE',  ( 5.412658773652739619, 3.124999999999988898, -55.31698729810785409 ) ) ;
#8451 = CARTESIAN_POINT ( 'NONE',  ( 104.1247167782375556, -1.849990392679468076, 0.000000000000000000 ) ) ;
#8452 = CARTESIAN_POINT ( 'NONE',  ( -3.464101615137757051, -5.999999999999979572, -128.6636751345948255 ) ) ;
#8453 = CARTESIAN_POINT ( 'NONE',  ( 148.2261751345948539, -3.889087296526011706, -3.889087296526011706 ) ) ;
#8454 = CARTESIAN_POINT ( 'NONE',  ( 6.000000000000000888, 1.743066579297358182E-13, -75.08632486540521711 ) ) ;
#8455 = EDGE_CURVE ( 'NONE', #15757, #24851, #9941, .T. ) ;
#8456 = CARTESIAN_POINT ( 'NONE',  ( -6.350852961085760029, -1.281975124255709124E-13, -128.6250000000000000 ) ) ;
#8457 = ORIENTED_EDGE ( 'NONE', *, *, #24672, .F. ) ;
#8458 = CARTESIAN_POINT ( 'NONE',  ( 0.000000000000000000, 5.999999999999977796, -157.7886751345948255 ) ) ;
#8459 = CYLINDRICAL_SURFACE ( 'NONE', #11948, 6.000000000000000888 ) ;
#8460 = CARTESIAN_POINT ( 'NONE',  ( 12.83632486540528461, 1.767766952966431937, 1.767766952966320915 ) ) ;
#8461 = CARTESIAN_POINT ( 'NONE',  ( 141.3898502691896510, 3.535533905932725318, -3.535533905932725318 ) ) ;
#8462 = EDGE_LOOP ( 'NONE', ( #18030, #19191, #23892, #1263 ) ) ;
#8463 = CARTESIAN_POINT ( 'NONE',  ( 115.1872167782374987, -1.849990392679441875, -0.7662911109075283278 ) ) ;
#8464 = CARTESIAN_POINT ( 'NONE',  ( 6.000000000000000888, -1.859271017917181981E-14, -72.08632486540521711 ) ) ;
#8465 = CARTESIAN_POINT ( 'NONE',  ( 10.06250000000005151, 2.000000000000212275, 0.8284271247461152399 ) ) ;
#8466 = CARTESIAN_POINT ( 'NONE',  ( -7.216878364870328078, 0.000000000000000000, -114.6919872981078328 ) ) ;
#8467 = CARTESIAN_POINT ( 'NONE',  ( 147.6636751345948255, 0.000000000000000000, 5.500000000000005329 ) ) ;
#8468 = CARTESIAN_POINT ( 'NONE',  ( 112.9374999999997726, 2.500000000000115019, -1.035533905932448873 ) ) ;
#8469 = VERTEX_POINT ( 'NONE', #14905 ) ;
#8470 = DIRECTION ( 'NONE',  ( -7.147005652999508048E-36, 5.642372883946980038E-36, 1.000000000000000000 ) ) ;
#8471 = CARTESIAN_POINT ( 'NONE',  ( 142.5000000000000568, 6.000000000000005329, 0.000000000000000000 ) ) ;
#8472 = ORIENTED_EDGE ( 'NONE', *, *, #2159, .T. ) ;
#8473 = DIRECTION ( 'NONE',  ( 0.000000000000000000, 0.000000000000000000, 1.000000000000000000 ) ) ;
#8474 = ADVANCED_FACE ( 'NONE', ( #26550 ), #15519, .T. ) ;
#8475 = CARTESIAN_POINT ( 'NONE',  ( 6.350852961086080661, -9.614813431917819062E-14, -46.87500000000000000 ) ) ;
#8476 = CARTESIAN_POINT ( 'NONE',  ( 136.6011751345948539, 3.889087296526011706, -3.889087296526011706 ) ) ;
#8477 = CARTESIAN_POINT ( 'NONE',  ( 7.216878364870455975, -6.409875621278545621E-14, -74.30801270189223828 ) ) ;
#8478 = DIRECTION ( 'NONE',  ( -1.000000000000000000, -1.665334536937736783E-16, -2.220446049250315546E-16 ) ) ;
#8479 = CARTESIAN_POINT ( 'NONE',  ( 153.0788997308104058, -4.999999999999989342, 2.071067811865468400 ) ) ;
#8480 = CARTESIAN_POINT ( 'NONE',  ( 6.000000000000000888, 1.743066579297358182E-13, -102.6636751345948397 ) ) ;
#8481 = DIRECTION ( 'NONE',  ( 1.000000000000000000, 1.067522139062651411E-16, 0.000000000000000000 ) ) ;
#8482 = DIRECTION ( 'NONE',  ( -7.147005652999508048E-36, 5.642372883946980038E-36, 1.000000000000000000 ) ) ;
#8483 =( BOUNDED_CURVE ( )  B_SPLINE_CURVE ( 2, ( #1525, #8598, #22593, #21978, #20285, #911, #29478, #26702, #5816 ),
 .UNSPECIFIED., .F., .F. ) 
 B_SPLINE_CURVE_WITH_KNOTS ( ( 3, 2, 2, 2, 3 ),
 ( 0.002777777777777767909, 0.003703703703703653538, 0.005555555555555535818, 0.007407407407407418098, 0.008333333333333414750 ),
 .UNSPECIFIED. ) 
 CURVE ( )  GEOMETRIC_REPRESENTATION_ITEM ( )  RATIONAL_B_SPLINE_CURVE ( ( 0.9330127018922194093, 0.9330127018922194093, 1.000000000000000000, 0.8660254037844388186, 1.000000000000000000, 0.8660254037844388186, 1.000000000000000000, 0.9330127018922154125, 0.9330127018922194093 ) ) 
 REPRESENTATION_ITEM ( '' )  );
#8484 = ADVANCED_FACE ( 'NONE', ( #22264 ), #17371, .T. ) ;
#8485 = CARTESIAN_POINT ( 'NONE',  ( -2.775557561562891351E-14, -5.500000000000115463, -131.2500000000000284 ) ) ;
#8486 = CARTESIAN_POINT ( 'NONE',  ( 10.47617513459493743, 1.035533905932869425, 2.499999999999844569 ) ) ;
#8487 = FACE_OUTER_BOUND ( 'NONE', #16560, .T. ) ;
#8488 =( NAMED_UNIT ( * ) SI_UNIT ( $, .STERADIAN. ) SOLID_ANGLE_UNIT ( ) );
#8489 = VERTEX_POINT ( 'NONE', #22113 ) ;
#8490 = CARTESIAN_POINT ( 'NONE',  ( 3.175426480543072749, -5.500000000000105693, -59.12499999999999289 ) ) ;
#8491 = CARTESIAN_POINT ( 'NONE',  ( -3.464101615137757051, -5.999999999999979572, -77.08632486540521711 ) ) ;
#8492 =( BOUNDED_CURVE ( )  B_SPLINE_CURVE ( 2, ( #6867, #18875, #23481 ),
 .UNSPECIFIED., .F., .T. ) 
 B_SPLINE_CURVE_WITH_KNOTS ( ( 3, 3 ),
 ( 0.01315883293259485255, 0.01562500000000000000 ),
 .UNSPECIFIED. ) 
 CURVE ( )  GEOMETRIC_REPRESENTATION_ITEM ( )  RATIONAL_B_SPLINE_CURVE ( ( 0.9671125746063278239, 0.9759710988702530177, 1.000000000000000000 ) ) 
 REPRESENTATION_ITEM ( '' )  );
#8493 = CARTESIAN_POINT ( 'NONE',  ( 6.000000000000052403, -1.607695154586662678, -174.1533121635130215 ) ) ;
#8494 = EDGE_LOOP ( 'NONE', ( #4101, #30394, #13208, #17097 ) ) ;
#8495 = CARTESIAN_POINT ( 'NONE',  ( 107.9999999999998863, 2.500000000000002220, 0.000000000000000000 ) ) ;
#8496 = CARTESIAN_POINT ( 'NONE',  ( 144.8437500000000000, -6.000000000000005329, -2.485281374238556218 ) ) ;
#8497 = CARTESIAN_POINT ( 'NONE',  ( -5.196152422706573404, -3.000000000000002665, -118.2886751345948397 ) ) ;
#8498 = CARTESIAN_POINT ( 'NONE',  ( 5.196152422706629359, -2.999999999999988898, -48.78867513459483973 ) ) ;
#8499 = ORIENTED_EDGE ( 'NONE', *, *, #6809, .T. ) ;
#8500 = CARTESIAN_POINT ( 'NONE',  ( 136.3125000000000284, 4.242640687119298093, -4.242640687119298093 ) ) ;
#8501 = CARTESIAN_POINT ( 'NONE',  ( 161.3463853183868366, -5.851553901883566944, -0.2004824262064201779 ) ) ;
#8502 = ORIENTED_EDGE ( 'NONE', *, *, #16577, .F. ) ;
#8503 = CARTESIAN_POINT ( 'NONE',  ( 3.175426480543072749, -5.500000000000105693, -141.6250000000000000 ) ) ;
#8504 = ORIENTED_EDGE ( 'NONE', *, *, #4839, .F. ) ;
#8505 = CARTESIAN_POINT ( 'NONE',  ( 2.775557561562891351E-14, 6.250000000000033751, -47.56698729810781856 ) ) ;
#8506 = CARTESIAN_POINT ( 'NONE',  ( 19.00000000000020961, 2.000000000000223821, -5.551115123125782702E-14 ) ) ;
#8507 = ORIENTED_EDGE ( 'NONE', *, *, #26909, .F. ) ;
#8508 = EDGE_CURVE ( 'NONE', #19788, #18908, #7582, .T. ) ;
#8509 = CARTESIAN_POINT ( 'NONE',  ( 6.350852961086080661, -9.614813431917819062E-14, -75.37500000000000000 ) ) ;
#8510 = VERTEX_POINT ( 'NONE', #25297 ) ;
#8511 = DIRECTION ( 'NONE',  ( 1.000000000000000000, 1.734723475976843579E-16, -0.000000000000000000 ) ) ;
#8512 = CARTESIAN_POINT ( 'NONE',  ( 106.2113248654051745, -1.999999999999946265, 0.000000000000000000 ) ) ;
#8513 = CARTESIAN_POINT ( 'NONE',  ( 135.0000000000000284, -6.982120021884474781, -8.500000000000007105 ) ) ;
#8514 = CARTESIAN_POINT ( 'NONE',  ( 110.6636751345946976, -1.414213562373090038, 1.414213562373034527 ) ) ;
#8515 = EDGE_CURVE ( 'NONE', #28288, #28619, #30196, .T. ) ;
#8516 = DIRECTION ( 'NONE',  ( 0.000000000000000000, -0.5343848195299158998, 0.8452413055784600004 ) ) ;
#8517 = EDGE_CURVE ( 'NONE', #14191, #5616, #22860, .T. ) ;
#8518 = CARTESIAN_POINT ( 'NONE',  ( 3.175426480543072749, -5.500000000000105693, -158.1250000000000284 ) ) ;
#8519 = DIRECTION ( 'NONE',  ( 0.000000000000000000, 0.000000000000000000, 1.000000000000000000 ) ) ;
#8520 = AXIS2_PLACEMENT_3D ( 'NONE', #17099, #21698, #10946 ) ;
#8521 = FACE_OUTER_BOUND ( 'NONE', #19619, .T. ) ;
#8522 = CARTESIAN_POINT ( 'NONE',  ( 0.000000000000000000, 5.499999999999991118, -90.00000000000002842 ) ) ;
#8523 = CARTESIAN_POINT ( 'NONE',  ( -5.196152422706573404, -3.000000000000002665, -140.7886751345947971 ) ) ;
#8524 = DIRECTION ( 'NONE',  ( -1.000000000000000000, 0.000000000000000000, 0.000000000000000000 ) ) ;
#8525 = CARTESIAN_POINT ( 'NONE',  ( 0.000000000000000000, 5.499999999999991118, -73.50000000000001421 ) ) ;
#8526 = DIRECTION ( 'NONE',  ( 1.000000000000000000, -5.551115123125773458E-17, -1.260129944081490338E-35 ) ) ;
#8527 = CARTESIAN_POINT ( 'NONE',  ( 153.4836002691896226, 4.999999999999989342, -2.071067811865468400 ) ) ;
#8528 = CARTESIAN_POINT ( 'NONE',  ( 150.2886751345948255, 5.500000000000005329, 0.000000000000000000 ) ) ;
#8529 = CARTESIAN_POINT ( 'NONE',  ( 0.000000000000000000, -5.999999999999991118, -108.4613248654052171 ) ) ;
#8530 = CARTESIAN_POINT ( 'NONE',  ( 135.5699251345948255, 2.278174593052383567, 5.499999999999640288 ) ) ;
#8531 =( BOUNDED_CURVE ( )  B_SPLINE_CURVE ( 2, ( #27169, #8597, #25017, #20426, #3358, #29320, #29476, #1374, #17691 ),
 .UNSPECIFIED., .F., .F. ) 
 B_SPLINE_CURVE_WITH_KNOTS ( ( 3, 2, 2, 2, 3 ),
 ( 0.9361111111111111160, 0.9370370370370370017, 0.9388888888888888840, 0.9407407407407407662, 0.9416666666666666519 ),
 .UNSPECIFIED. ) 
 CURVE ( )  GEOMETRIC_REPRESENTATION_ITEM ( )  RATIONAL_B_SPLINE_CURVE ( ( 0.9330127018922194093, 0.9330127018922194093, 1.000000000000000000, 0.8660254037844388186, 1.000000000000000000, 0.8660254037844388186, 1.000000000000000000, 0.9330127018922194093, 0.9330127018922194093 ) ) 
 REPRESENTATION_ITEM ( '' )  );
#8532 = CARTESIAN_POINT ( 'NONE',  ( 111.7738248654051745, 2.000000000000061728, 0.8284271247463557142 ) ) ;
#8533 = LINE ( 'NONE', #27254, #28333 ) ;
#8534 = DIRECTION ( 'NONE',  ( -7.147005652999508048E-36, 5.642372883946980038E-36, 1.000000000000000000 ) ) ;
#8535 = ORIENTED_EDGE ( 'NONE', *, *, #2677, .F. ) ;
#8536 = CARTESIAN_POINT ( 'NONE',  ( 154.7812500000000568, 2.485281374238585972, 6.000000000000005329 ) ) ;
#8537 = CARTESIAN_POINT ( 'NONE',  ( -0.07769256095284393648, -15.23231281889969679, 7.500000000000007105 ) ) ;
#8538 = CARTESIAN_POINT ( 'NONE',  ( -5.999999999999963585, -1.487416814333745711E-14, -172.4136751345948255 ) ) ;
#8539 = CARTESIAN_POINT ( 'NONE',  ( 116.6252832217622313, 0.000000000000000000, 1.849990392679523588 ) ) ;
#8540 =( BOUNDED_SURFACE ( )  B_SPLINE_SURFACE ( 1, 2, ( 
 ( #7053, #7205, #2728, #16616, #18756, #26088, #143, #21793, #14314, #19348, #12306, #28078, #14461, #9970, #16465, #18911, #28231, #21502, #21202, #17051, #14595, #2451, #23947, #25794, #28667, #3033, #28377, #429, #4744, #23794, #4884, #11862, #23508, #9818, #9524, #7357, #28523, #23655, #2591, #12010, #21345, #26230, #9670, #286, #19060, #16762, #12157, #19194, #16905, #5182, #2884, #21647, #583, #26525, #15033, #17649, #1026, #22091, #10577, #19776, #24683, #29124, #13060, #13216, #29432, #8084, #29277, #876, #27131, #21940, #3625, #22393, #5627, #8403, #3784, #17811, #1332, #22553, #24380, #6100, #15512, #7942, #10424, #12597, #7785, #8237, #19931, #10274, #24834, #26667, #17201, #10744, #15360, #3323, #17498, #26971, #20089, #19638, #5478, #5936, #12751, #26814, #3176, #24226, #10123, #19494, #14884, #5777, #15189, #28824, #28975, #17352, #24523, #3471, #12905, #22241, #1169, #30053, #4244, #8719, #1486, #13824, #6393, #23168, #22852, #4558, #11357, #20704, #9170, #18263, #27889, #20856, #11040, #9023, #18565, #18413, #13982, #27427, #30209, #6249, #29743, #4398, #20249, #20386, #15974, #18107, #10895, #8875, #13356, #25606, #15826, #2112, #25435, #29598, #27574, #11516, #8558, #1641, #25126, #13667, #3929, #6860, #27733, #15668, #6712, #17963, #16286, #27275, #11197, #23009, #24977, #6554, #22702, #4091, #13511, #25272, #16129, #1790, #1953, #20544, #29894, #18719, #5291, #247, #28343, #9935, #26343, #9630, #7461, #25900, #25754, #393, #4702, #5144, #23618, #23322, #28629, #19023, #18868, #2265, #26052, #11672, #14277, #23765, #21013, #19161, #7318, #14562, #28496, #544, #9783, #14428, #23475, #16430, #7600, #2848, #23906, #12268, #17014, #2552, #19309, #14136, #16728, #11979, #7165, #21613, #16872, #28043, #21307, #28189, #4995, #2696, #30360, #16580, #26193, #9327, #7013, #12121, #2412, #21462, #11824, #21163, #102, #9485, #4849, #21907, #702, #7751, #24194, #1137, #3287, #19459, #12415, #19740, #14994, #3589, #8365, #24484, #10706, #17775, #22356, #27095, #13020, #10086, #8200, #26481, #26632, #26777, #24333, #14700, #1292, #26933, #8048, #22052, #24047, #20050, #14850, #29087, #29236, #3139, #21759, #5590, #17461, #2994, #3434, #12713, #28940, #987, #28787, #29395, #5894, #17316, #7902, #17615, #17161, #841, #12561, #10241, #10388, #5743, #19600, #10538, #15152, #5440, #12866, #22204, #19892, #15321, #24644, #25237, #20822, #9134, #13785, #18526, #25399, #1911, #8987, #11318, #27693, #4360, #23129, #13183, #26572, #10168, #21693, #5226, #10315, #24265, #28003, #12343, #12499, #16391, #4520, #19241, #630, #27851, #17095, #26275, #11782, #9868, #13942, #5522, #19537, #61, #21123, #785, #17246, #14099, #25713, #4666, #28567, #23983, #6820, #28871, #7831, #10013, #5374, #14930, #14639, #12638, #21984, #23288, #16245, #2927, #19391, #916, #25559, #28716, #21837, #7536, #30324, #14783, #9285, #2230, #16947, #11631, #20976, #7687, #23435, #18680, #26423, #6973, #24128, #3075, #2378, #15564, #3674, #1533, #24881, #27330, #27179, #10790, #19823, #12795, #25027, #29640, #10943, #20292, #3981, #29329, #6295, #1079, #13110, #8287, #3522, #18013, #3830, #15081, #17700, #15241, #22446, #27027, #8605, #12952, #13259, #6149, #3366, #24732, #22600, #5991, #15718, #13404, #22750, #8456, #1382, #26863, #5672, #22137, #10469, #17394, #1692, #5823, #22289, #29168, #8131, #19680, #17861, #26708, #15408, #20140, #29022, #7987, #24422, #17546, #24573, #1216, #29487, #10627, #19978, #13873, #18312, #11089, #23366, #16024, #2310, #1998, #14177, #20906, #30250, #18763, #27780, #7059, #30403, #20592, #9219, #28084, #18610, #23514, #6602, #9371, #15875, #8922, #14026, #29793, #29942, #25481, #27624, #20434, #18459, #22899, #4750, #25323, #11711, #4597, #8769, #6756, #21055, #18156, #11244, #4298, #23214, #13559, #16472, #6905, #25173, #16327, #27469, #25801, #6446, #20752, #2160, #4138, #16176, #13716, #1843, #23057, #11562, #11407, #30101, #27931, #9066, #4448, #25647, #7364, #9978, #23803, #14469, #2893, #12164, #17059, #21510, #5336, #5487, #21801, #437, #21656, #23662, #19501, #14322, #26389, #14747, #28384, #748, #26535, #10134, #24091, #14891, #16771, #28833, #7792, #291, #2737, #4891, #149, #592, #12314, #2597, #17207, #19068, #9529, #3041, #7650, #26096, #9825, #19355, #12458, #2455, #11870, #12016, #28676, #21208, #18917, #28238, #5038, #7212, #16624, #9678, #25944, #21352, #19202, #16913, #28531, #7500, #26238, #5191, #14603, #23955, #24841, #17818, #6255, #19937, #15517, #24233, #24388, #3333, #26980, #26676, #13221, #20095, #7950, #29439, #21950, #3791, #22559, #3479, #5944, #20257, #10586, #12758, #17360, #1490, #15366, #10901, #12911, #3632, #22100, #884, #10282, #29133, #1339, #15199, #5784, #24690, #22248, #8412, #1177, #27138, #27281, #29603, #29284, #13069, #15042, #8563, #5636, #6107, #17968, #19784, #3183, #12607, #19645, #28984, #1034, #8092, #10434, #17507, #26820, #24531, #8243, #17655, #22402, #10751, #15833, #2271, #1797, #13363, #9175, #20862, #20549, #27579, #16134, #27894, #27432, #22708, #2117, #11203, #8880, #8725, #29749, #16290, #13829, #1649, #4250, #25280, #21017, #6866, #30212, #25610, #13520, #11047, #23014, #24982, #23175, #18417, #22858, #15674, #4563, #29901, #13987, #6560, #18723, #25440, #4404, #23327, #1959, #18268, #15979, #18114, #6399, #11676, #11521, #20391, #13672, #11364, #30366, #9333, #18572, #28048, #20709, #25132, #30057, #3933, #4097, #27738, #9028, #6718, #19316, #11983, #28637, #28348, #10094, #16878, #26198, #14708, #23767, #2999, #26348, #16586, #5150, #24052, #14565, #19464, #2559, #5296, #11832, #4857, #9940, #25760, #25907, #21470, #14283, #7019, #14434, #18874, #706, #21313, #7608, #551, #16436, #2701, #17020, #4707, #7171, #23625, #9788, #9492, #12419, #2855, #21168, #12274, #14141, #21763, #23480, #16732, #19166, #2417, #12127, #255, #110, #28197, #28500, #9638, #26056, #23912, #19030, #7324, #5001, #398, #21618, #7466, #10394, #29242, #8052, #13025, #17467, #1297, #1456, #17781, #26781, #17620, #19605, #15480, #10248, #22362, #10711, #24339, #27100, #22524, #6068, #20055, #10865, #12720, #24807, #3755, #26637, #19745, #847, #26488, #26940, #8204, #28944, #13188, #14999, #5444, #29401, #3596, #3293, #29091, #5901, #8371, #7907, #14854, #15328, #28793, #17320, #12870, #7755, #5596, #24198, #5746, #22210, #17167, #24649, #15158, #22058, #24490, #3144, #12568, #21913, #992, #3437, #1144, #10543, #19900, #18082, #8686, #22819, #15944, #2235, #11485, #2080, #4214, #27698, #30176, #6521, #20827, #4526, #15637, #20220, #27545, #25242, #6825, #23293, #13633, #4366, #1761, #22669, #6680, #1611, #9141, #20509, #29567, #25567, #22978, #15794, #8525, #1917, #17931, #11162, #20669, #27248, #16100, #11325, #18533, #25404, #27856, #13791, #30023, #20358, #13330, #13948, #16251, #6221, #24947, #3900, #29864, #11014, #29712, #8993, #8843, #4056, #27394, #23136, #6361, #18228, #25100, #18382, #13479, #12240, #25873, #26162, #19129, #25721, #16695, #7432, #28316, #16841, #2818, #14533, #361, #26017, #18834, #28008, #4669, #21129, #28462, #215, #16398, #9292, #4966, #11950, #511, #5267, #21430, #7573, #14674, #19281, #24018, #9905, #6981, #5113, #23441, #23584, #23734, #21275, #11637, #28603, #23873, #14399, #18991, #20983, #16553, #21579, #2522, #30331, #9752, #16988, #26311, #7292, #18686, #14104, #67, #2382, #11789, #9453, #28161, #7130, #4822, #14247, #9601, #2666, #12090, #21876, #17432, #815, #2964, #10355, #14824, #27065, #28908, #3561, #26902, #15448, #29060, #24610, #12384, #3110, #12534, #5712, #5412, #22327, #29208, #17133, #8169, #670, #12991, #1261, #12686, #15123, #29366, #19716, #10209, #26459, #10671, #24454, #20018, #22019, #12831, #19573, #10056, #19431, #7873, #10507, #24305, #14965, #3408, #954, #17585, #8026, #5865, #6029, #8330, #26746, #22175, #24168, #17741, #17286, #15283, #21731, #26608, #28757, #7726, #5562, #3254, #1109, #19862, #23209, #30246, #22747, #6443, #27327, #22597, #23053, #4293, #25023, #11557, #11086, #1530, #18455, #30097, #29790, #15872, #25318, #6752, #6290, #10940, #11401, #20431, #18152, #18010, #8603, #25477, #1993, #20288, #13554, #4135, #9214, #16173, #9062, #4444, #1688, #29637, #1839, #3827, #20747, #27622, #8766, #24877, #13869, #27464, #2155, #15713, #25170, #27776, #13257, #13401, #8918, #22897, #3978, #11241, #20589, #18605 ),
 ( #29938, #18308, #6597, #20902, #16020, #13712, #27927, #6900, #432, #4887, #19197, #19351, #5186, #25939, #5031, #7055, #2887, #28080, #9821, #28526, #11864, #14598, #9973, #23950, #7495, #28670, #145, #12308, #21651, #14172, #28233, #18759, #14020, #14464, #26091, #16467, #586, #2453, #23362, #16908, #21505, #21204, #7207, #16764, #26233, #25796, #2306, #2731, #9526, #18913, #9366, #30399, #16324, #23797, #11706, #14316, #23657, #25643, #4593, #21051, #4746, #23510, #16618, #2593, #12012, #12160, #19062, #21347, #288, #9672, #28379, #7359, #28978, #10747, #17501, #26816, #15362, #24383, #3628, #26974, #17204, #5779, #24686, #15193, #20091, #10428, #14887, #7645, #19934, #12601, #29280, #7945, #17054, #24525, #3474, #13064, #3326, #22396, #5939, #26528, #12907, #1335, #22244, #26384, #3179, #5331, #12453, #5481, #10580, #14741, #24228, #22094, #21943, #24085, #15036, #19497, #3036, #879, #8239, #1172, #21795, #12754, #17652, #743, #7788, #10277, #19779, #10127, #28827, #19640, #17355, #26670, #5630, #1029, #29127, #8087, #2231, #25869, #16246, #18377, #13626, #21124, #11632, #62, #18527, #9286, #27694, #6103, #15514, #4361, #6974, #20823, #11481, #30325, #9135, #14100, #27852, #2379, #2516, #18829, #6821, #18681, #20666, #16547, #11319, #23436, #11783, #25400, #28155, #23579, #7125, #9447, #11946, #13786, #4818, #14244, #6674, #30171, #1912, #27134, #28005, #16392, #30017, #29435, #16093, #24837, #8406, #4667, #23131, #25561, #25714, #17814, #8988, #4209, #22974, #2077, #4521, #13943, #23289, #20977, #19426, #28309, #9902, #506, #26604, #3105, #26456, #812, #19125, #7287, #28598, #210, #28753, #24163, #9597, #9749, #14669, #28456, #21269, #7566, #2661, #14961, #16836, #21872, #10203, #3249, #16984, #19569, #16690, #21424, #7428, #24016, #23728, #28903, #17130, #4960, #5407, #26012, #7868, #17282, #19277, #2961, #5558, #26307, #26157, #14392, #24302, #12379, #12084, #21726, #10048, #5109, #14530, #23869, #2811, #7722, #12236, #21576, #22482, #22322, #15599, #20012, #24913, #15754, #1572, #24769, #1418, #3405, #8642, #10504, #3862, #10980, #26898, #18047, #6326, #27360, #12679, #19712, #12987, #19858, #3711, #20177, #29529, #17894, #22784, #27820, #25524, #6488, #27967, #22939, #29830, #13910, #4487, #11284, #8959, #30140, #2194, #15914, #8806, #23256, #29982, #27664, #25210, #6644, #20941, #9253, #16064, #25366, #23097, #4634, #14065, #4019, #2042, #11449, #20793, #9102, #10450, #29620, #3809, #8265, #1060, #13385, #5967, #22728, #22422, #4117, #17990, #27306, #8748, #17840, #27448, #20412, #10603, #6274, #18134, #15694, #13539, #27003, #29772, #5803, #17679, #3654, #3503, #25005, #12933, #1671, #1361, #19804, #6420, #27159, #15388, #29149, #13238, #8109, #10771, #1511, #17528, #11066, #15542, #15855, #25154, #26841, #15220, #22582, #19957, #24551, #22269, #24711, #13090, #20119, #29462, #8434, #6129, #24861, #16312, #11540, #6735, #21189, #18748, #18290, #20883, #18440, #25634, #2140, #23498, #16154, #7045, #30387, #6581, #27910, #28069, #9197, #16457, #14161, #25784, #11697, #6888, #30080, #8900, #16004, #1978, #9355, #30234, #27604, #20573, #4582, #23194, #11851, #16607, #2293, #18902, #25928, #131, #4875, #9515, #25304, #4732, #4275, #4427, #14007, #18589, #22878, #28222, #2441, #23352, #21041, #1821, #7195, #23037, #11224, #29923, #11386, #13698, #13854, #20729, #9049, #27758, #25463, #28514, #26214, #21336, #21929, #26513, #16895, #7483, #17190, #3163, #417, #12146, #2720, #5170, #9959, #26654, #5464, #14872, #28657, #21783, #24215, #571, #12587, #28965, #9660, #14306, #21636, #19337, #862, #17338, #7628, #28812, #24070, #21491, #277, #19050, #19185, #726, #14583, #23935, #14727, #2872, #7773, #12292, #10262, #23646, #19623, #17038, #3020, #5018, #7928, #26077, #2579, #12002, #9806, #28366, #7346, #16751, #14449, #23784, #26370, #5318, #12437, #10111, #19480, #8069, #3311, #3774, #15502, #5766, #22692, #22228, #12738, #29588, #10885, #10563, #17639, #6088, #17954, #17487, #22078, #22540, #1159, #29266, #29111, #19764, #6238, #13206, #1012, #24670, #15351, #11030, #27266, #20240, #15658, #3459, #10413, #13049, #15023, #1474, #8392, #19920, #5615, #24965, #8226, #3919, #26962, #8709, #24827, #8548, #13348, #22381, #1630, #20376, #15175, #29731, #18099, #24366, #26801, #5923, #24510, #3614, #1320, #10732, #20078, #29421, #17799, #27117, #27415, #4386, #8866, #21150, #22998, #28031, #21005, #9474, #23159, #18708, #6382, #27564, #6543, #30200, #29884, #16422, #23313, #11187, #2257, #25116, #7002, #25743, #6700, #9161, #23465, #13813, #15964, #20535, #4690, #18555, #14125, #16119, #2401, #2100, #25262, #18249, #11813, #27880, #90, #25423, #6848, #4234, #4079, #13501, #1941, #4546, #18405, #9013, #16275, #11507, #11661, #20847, #30351, #15816, #22841, #25594, #13971, #13657, #1782, #11345, #9316, #20691, #30042, #27721, #21898, #14841, #21751, #16568, #21449, #17153, #3130, #16716, #9773, #21298, #14269, #17006, #28621, #19010, #23609, #14417, #2545, #690, #24038, #23754, #19150, #19299, #10075, #236, #9620, #2983, #7450, #26183, #28334, #26041, #28774, #26331, #5132, #14554, #23896, #2837, #7745, #534, #9925, #8043, #26623, #17607, #19592, #8353, #13010, #17453, #10231, #22509, #15143, #1443, #1129, #13317, #20041, #29387, #17919, #26923, #6206, #29554, #19731, #17761, #27235, #27085, #22658, #5733, #15625, #14985, #26767, #13172, #28929, #29079, #24633, #24474, #7893, #5884, #22040, #3885, #3424, #10851, #3738, #5581, #15309, #20204, #24325, #10376, #12854, #22348, #12704, #24935, #6052, #3278, #15467, #976, #10528, #19882, #29229, #1282, #8191, #24792, #3581, #10695, #1901, #14090, #25704, #18371, #11308, #1598, #4349, #29698, #20657, #11470, #6346, #25550, #25390, #13934, #11623, #27993, #20966, #30162, #1747, #4043, #15781, #30317, #13463, #22807, #11146, #30005, #20494, #29852, #13776, #12076, #7279, #21718, #19265, #18821, #21414, #28297, #16828, #2652, #24007, #16683, #7557, #496, #7115, #28446, #28591, #9738, #16974, #14662, #26298, #12228, #7421, #201, #9437, #16535, #2506, #9892, #347, #28147, #21115, #26149, #23718, #12369, #17121, #2801, #19417, #26447, #658, #5401, #10040, #25862, #5253, #4808, #4950, #5096, #19117, #23426, #28741, #2952, #14523, #23862, #2371, #7713, #23571, #21566, #11773, #11934, #50, #14382, #14236, #21261, #9588, #26004, #29048, #26735, #21862, #22470, #27050, #17421, #8013, #17725, #3701, #942, #12668, #22005, #5701, #10496, #27202, #6015, #15434, #29194, #22312, #24761, #19846, #13132, #29516, #10193, #14809, #22162, #8155, #1408, #17886, #17571, #29354, #15110, #12978, #10817, #3546, #24155, #10342, #20167, #19561, #19704, #8477, #3097, #24441, #26888, #3393, #12524, #5850, #26593, #806, #12819, #28896, #8316, #7861, #15268, #17273, #5549, #14954, #24294, #24596, #1245, #10654, #20003, #20317, #2029, #3854, #6781, #4475, #15901, #8948, #2183, #22927, #25053, #29665, #27806, #18339, #16201, #25200, #16053, #4012, #13285, #22628, #11113, #13741, #27501, #18183, #6631, #4163, #20781, #13588, #9091, #9240, #25511, #1869, #25354, #27354, #23241, #18038, #30128, #18487, #1717, #13901, #30282, #11586, #20930, #18634, #20461, #6177, #15590, #13428, #6479, #8634, #1564, #4323, #23087, #6317, #24905, #22773, #10969, #15743, #11435, #29820, #11271, #8797, #20624, #29970, #27655, #14879, #14591, #21642, #15, #11738, #28970, #26520, #4622, #17044, #7635, #3317, #10267, #3170, #7935, #26223, #23391, #5323, #6930, #5473, #735, #5176, #27955, #19632, #2879, #17346, #19343, #1019, #7779, #17196, #5621, #14734, #24373, #26660, #7086, #28113, #18791, #12744, #15028, #22084, #10418, #16353, #26376, #25672, #16501, #21788, #24078, #12300, #2338, #24221, #23942, #3027, #579, #10117, #12444, #9965, #28663, #12593, #21934, #19489, #28819, #870, #6094, #24970, #11035, #22697, #8552, #3780, #26966, #15181, #12899, #29271, #6243, #8398, #24517, #26806, #24830, #20083, #8714, #13506, #29594, #15821, #1785, #27421, #19770, #18103, #3464, #13354, #1164, #1324, #1480, #29427, #29118, #25121, #1635, #13210, #27122, #8077, #4085, #19924, #22545, #3925, #8231, #22234, #10738, #10890, #10571, #17960, #17805, #3618, #15507, #17643, #5929, #20380, #22388, #13055, #29738, #15354, #24677, #20244, #27271, #15665, #6852, #23614, #2407, #23469, #25600, #18712, #21157, #27884, #11818, #25895, #6549, #11192, #18559 ) ),
 .UNSPECIFIED., .F., .F., .F. ) 
 B_SPLINE_SURFACE_WITH_KNOTS ( ( 2, 2 ),
 ( 3, 2, 2, 2, 2, 2, 2, 2, 2, 2, 2, 2, 2, 2, 2, 2, 2, 2, 2, 2, 2, 2, 2, 2, 2, 2, 2, 2, 2, 2, 2, 2, 2, 2, 2, 2, 2, 2, 2, 2, 2, 2, 2, 2, 2, 2, 2, 2, 2, 2, 2, 2, 2, 2, 2, 2, 2, 2, 2, 2, 2, 2, 2, 2, 2, 2, 2, 2, 2, 2, 2, 2, 2, 2, 2, 2, 2, 2, 2, 2, 2, 2, 2, 2, 2, 2, 2, 2, 2, 2, 2, 2, 2, 2, 2, 2, 2, 2, 2, 2, 2, 2, 2, 2, 2, 2, 2, 2, 2, 2, 2, 2, 2, 2, 2, 2, 2, 2, 2, 2, 2, 2, 2, 2, 2, 2, 2, 2, 2, 2, 2, 2, 2, 2, 2, 2, 2, 2, 2, 2, 2, 2, 2, 2, 2, 2, 2, 2, 2, 2, 2, 2, 2, 2, 2, 2, 2, 2, 2, 2, 2, 2, 2, 2, 2, 2, 2, 2, 2, 2, 2, 2, 2, 2, 2, 2, 2, 2, 2, 2, 2, 2, 2, 2, 2, 2, 2, 2, 2, 2, 2, 2, 2, 2, 2, 2, 2, 2, 2, 2, 2, 2, 2, 2, 2, 2, 2, 2, 2, 2, 2, 2, 2, 2, 2, 2, 2, 2, 2, 2, 2, 2, 2, 2, 2, 2, 2, 2, 2, 2, 2, 2, 2, 2, 2, 2, 2, 2, 2, 2, 2, 2, 2, 2, 2, 2, 2, 2, 2, 2, 2, 2, 2, 2, 2, 2, 2, 2, 2, 2, 2, 2, 2, 2, 2, 2, 2, 2, 2, 2, 2, 2, 2, 2, 2, 2, 2, 2, 2, 2, 2, 2, 2, 2, 2, 2, 2, 2, 2, 2, 2, 2, 2, 2, 2, 2, 2, 2, 2, 2, 2, 2, 2, 2, 2, 2, 2, 2, 2, 2, 2, 2, 2, 2, 2, 2, 2, 2, 2, 2, 2, 2, 2, 2, 2, 2, 2, 2, 2, 2, 2, 2, 2, 2, 2, 2, 2, 2, 2, 2, 2, 2, 2, 2, 2, 2, 2, 2, 2, 2, 2, 2, 2, 2, 2, 2, 2, 2, 2, 2, 2, 2, 2, 2, 2, 2, 2, 2, 2, 2, 2, 2, 2, 2, 2, 2, 2, 2, 2, 2, 2, 2, 2, 2, 2, 2, 2, 2, 2, 2, 2, 2, 2, 2, 2, 2, 2, 2, 2, 2, 2, 2, 2, 2, 2, 2, 2, 2, 2, 2, 2, 2, 2, 2, 2, 2, 2, 2, 2, 2, 2, 2, 2, 2, 2, 2, 2, 2, 2, 2, 2, 2, 2, 2, 2, 2, 2, 2, 2, 2, 2, 2, 2, 2, 2, 2, 2, 2, 2, 2, 2, 2, 2, 2, 2, 2, 2, 2, 2, 2, 2, 2, 2, 2, 2, 2, 2, 2, 2, 2, 2, 2, 2, 2, 2, 2, 2, 2, 2, 2, 2, 2, 2, 2, 2, 2, 2, 2, 2, 2, 2, 2, 2, 2, 2, 2, 2, 2, 2, 2, 2, 2, 2, 2, 2, 2, 2, 2, 2, 2, 2, 2, 2, 2, 2, 2, 2, 2, 2, 2, 2, 2, 2, 2, 2, 2, 2, 2, 2, 2, 2, 2, 2, 2, 2, 2, 2, 2, 2, 2, 3 ),
 ( 0.000000000000000000, 1.000000000000000000 ),
 ( 0.000000000000000000, 0.001851851851851851923, 0.003703703703703703845, 0.005555555555555555768, 0.007407407407407407690, 0.009259259259259258745, 0.01111111111111111154, 0.01296296296296296259, 0.01481481481481481538, 0.01666666666666666644, 0.01851851851851851749, 0.02037037037037037202, 0.02222222222222222307, 0.02407407407407407413, 0.02592592592592592518, 0.02777777777777777624, 0.02962962962962963076, 0.03148148148148147835, 0.03333333333333333287, 0.03518518518518518740, 0.03703703703703703498, 0.03888888888888888951, 0.04074074074074074403, 0.04259259259259259162, 0.04444444444444444614, 0.04629629629629629373, 0.04814814814814814825, 0.05000000000000000278, 0.05185185185185185036, 0.05370370370370370489, 0.05555555555555555247, 0.05740740740740740700, 0.05925925925925926152, 0.06111111111111110911, 0.06296296296296295669, 0.06481481481481481122, 0.06666666666666666574, 0.06851851851851852027, 0.07037037037037037479, 0.07222222222222221544, 0.07407407407407406996, 0.07592592592592592449, 0.07777777777777777901, 0.07962962962962963354, 0.08148148148148148806, 0.08333333333333332871, 0.08518518518518518323, 0.08703703703703703776, 0.08888888888888889228, 0.09074074074074074681, 0.09259259259259258745, 0.09444444444444444198, 0.09629629629629629650, 0.09814814814814815103, 0.1000000000000000056, 0.1018518518518518462, 0.1037037037037037007, 0.1055555555555555552, 0.1074074074074074098, 0.1092592592592592643, 0.1111111111111111049, 0.1129629629629629595, 0.1148148148148148140, 0.1166666666666666685, 0.1185185185185185230, 0.1203703703703703637, 0.1222222222222222182, 0.1240740740740740727, 0.1259259259259259134, 0.1277777777777777679, 0.1296296296296296224, 0.1314814814814814770, 0.1333333333333333315, 0.1351851851851851860, 0.1370370370370370405, 0.1388888888888888951, 0.1407407407407407496, 0.1425925925925926041, 0.1444444444444444309, 0.1462962962962962854, 0.1481481481481481399, 0.1499999999999999944, 0.1518518518518518490, 0.1537037037037037035, 0.1555555555555555580, 0.1574074074074074125, 0.1592592592592592671, 0.1611111111111111216, 0.1629629629629629761, 0.1648148148148148029, 0.1666666666666666574, 0.1685185185185185119, 0.1703703703703703665, 0.1722222222222222210, 0.1740740740740740755, 0.1759259259259259300, 0.1777777777777777846, 0.1796296296296296391, 0.1814814814814814936, 0.1833333333333333204, 0.1851851851851851749, 0.1870370370370370294, 0.1888888888888888840, 0.1907407407407407385, 0.1925925925925925930, 0.1944444444444444475, 0.1962962962962963021, 0.1981481481481481566, 0.2000000000000000111, 0.2018518518518518656, 0.2037037037037036924, 0.2055555555555555469, 0.2074074074074074014, 0.2092592592592592560, 0.2111111111111111105, 0.2129629629629629650, 0.2148148148148148195, 0.2166666666666666741, 0.2185185185185185286, 0.2203703703703703831, 0.2222222222222222099, 0.2240740740740740644, 0.2259259259259259189, 0.2277777777777777735, 0.2296296296296296280, 0.2314814814814814825, 0.2333333333333333370, 0.2351851851851851916, 0.2370370370370370461, 0.2388888888888889006, 0.2407407407407407274, 0.2425925925925925819, 0.2444444444444444364, 0.2462962962962962910, 0.2481481481481481455, 0.2500000000000000000, 0.2518518518518518268, 0.2537037037037037090, 0.2555555555555555358, 0.2574074074074074181, 0.2592592592592592449, 0.2611111111111111271, 0.2629629629629629539, 0.2648148148148148362, 0.2666666666666666630, 0.2685185185185185452, 0.2703703703703703720, 0.2722222222222221988, 0.2740740740740740811, 0.2759259259259259078, 0.2777777777777777901, 0.2796296296296296169, 0.2814814814814814992, 0.2833333333333333259, 0.2851851851851852082, 0.2870370370370370350, 0.2888888888888888618, 0.2907407407407407440, 0.2925925925925925708, 0.2944444444444444531, 0.2962962962962962798, 0.2981481481481481621, 0.2999999999999999889, 0.3018518518518518712, 0.3037037037037036979, 0.3055555555555555802, 0.3074074074074074070, 0.3092592592592592338, 0.3111111111111111160, 0.3129629629629629428, 0.3148148148148148251, 0.3166666666666666519, 0.3185185185185185341, 0.3203703703703703609, 0.3222222222222222432, 0.3240740740740740700, 0.3259259259259259522, 0.3277777777777777790, 0.3296296296296296058, 0.3314814814814814881, 0.3333333333333333148, 0.3351851851851851971, 0.3370370370370370239, 0.3388888888888889062, 0.3407407407407407329, 0.3425925925925926152, 0.3444444444444444420, 0.3462962962962962687, 0.3481481481481481510, 0.3499999999999999778, 0.3518518518518518601, 0.3537037037037036868, 0.3555555555555555691, 0.3574074074074073959, 0.3592592592592592782, 0.3611111111111111049, 0.3629629629629629872, 0.3648148148148148140, 0.3666666666666666408, 0.3685185185185185230, 0.3703703703703703498, 0.3722222222222222321, 0.3740740740740740589, 0.3759259259259259411, 0.3777777777777777679, 0.3796296296296296502, 0.3814814814814814770, 0.3833333333333333592, 0.3851851851851851860, 0.3870370370370370128, 0.3888888888888888951, 0.3907407407407407218, 0.3925925925925926041, 0.3944444444444444309, 0.3962962962962963132, 0.3981481481481481399, 0.4000000000000000222, 0.4018518518518518490, 0.4037037037037037313, 0.4055555555555555580, 0.4074074074074073848, 0.4092592592592592671, 0.4111111111111110938, 0.4129629629629629761, 0.4148148148148148029, 0.4166666666666666852, 0.4185185185185185119, 0.4203703703703703942, 0.4222222222222222210, 0.4240740740740740478, 0.4259259259259259300, 0.4277777777777777568, 0.4296296296296296391, 0.4314814814814814659, 0.4333333333333333481, 0.4351851851851851749, 0.4370370370370370572, 0.4388888888888888840, 0.4407407407407407662, 0.4425925925925925930, 0.4444444444444444198, 0.4462962962962963021, 0.4481481481481481288, 0.4500000000000000111, 0.4518518518518518379, 0.4537037037037037202, 0.4555555555555555469, 0.4574074074074074292, 0.4592592592592592560, 0.4611111111111111382, 0.4629629629629629650, 0.4648148148148147918, 0.4666666666666666741, 0.4685185185185185008, 0.4703703703703703831, 0.4722222222222222099, 0.4740740740740740922, 0.4759259259259259189, 0.4777777777777778012, 0.4796296296296296280, 0.4814814814814814548, 0.4833333333333333370, 0.4851851851851851638, 0.4870370370370370461, 0.4888888888888888729, 0.4907407407407407551, 0.4925925925925925819, 0.4944444444444444642, 0.4962962962962962910, 0.4981481481481481732, 0.5000000000000000000, 0.5018518518518518823, 0.5037037037037036535, 0.5055555555555555358, 0.5074074074074074181, 0.5092592592592593004, 0.5111111111111110716, 0.5129629629629629539, 0.5148148148148148362, 0.5166666666666667185, 0.5185185185185184897, 0.5203703703703703720, 0.5222222222222222543, 0.5240740740740740256, 0.5259259259259259078, 0.5277777777777777901, 0.5296296296296296724, 0.5314814814814814437, 0.5333333333333333259, 0.5351851851851852082, 0.5370370370370370905, 0.5388888888888888618, 0.5407407407407407440, 0.5425925925925926263, 0.5444444444444443976, 0.5462962962962962798, 0.5481481481481481621, 0.5500000000000000444, 0.5518518518518518157, 0.5537037037037036979, 0.5555555555555555802, 0.5574074074074074625, 0.5592592592592592338, 0.5611111111111111160, 0.5629629629629629983, 0.5648148148148147696, 0.5666666666666666519, 0.5685185185185185341, 0.5703703703703704164, 0.5722222222222221877, 0.5740740740740740700, 0.5759259259259259522, 0.5777777777777777235, 0.5796296296296296058, 0.5814814814814814881, 0.5833333333333333703, 0.5851851851851851416, 0.5870370370370370239, 0.5888888888888889062, 0.5907407407407407884, 0.5925925925925925597, 0.5944444444444444420, 0.5962962962962963243, 0.5981481481481480955, 0.5999999999999999778, 0.6018518518518518601, 0.6037037037037037424, 0.6055555555555555136, 0.6074074074074073959, 0.6092592592592592782, 0.6111111111111111605, 0.6129629629629629317, 0.6148148148148148140, 0.6166666666666666963, 0.6185185185185184675, 0.6203703703703703498, 0.6222222222222222321, 0.6240740740740741144, 0.6259259259259258856, 0.6277777777777777679, 0.6296296296296296502, 0.6314814814814815325, 0.6333333333333333037, 0.6351851851851851860, 0.6370370370370370683, 0.6388888888888888395, 0.6407407407407407218, 0.6425925925925926041, 0.6444444444444444864, 0.6462962962962962576, 0.6481481481481481399, 0.6500000000000000222, 0.6518518518518519045, 0.6537037037037036757, 0.6555555555555555580, 0.6574074074074074403, 0.6592592592592592116, 0.6611111111111110938, 0.6629629629629629761, 0.6648148148148148584, 0.6666666666666666297, 0.6685185185185185119, 0.6703703703703703942, 0.6722222222222222765, 0.6740740740740740478, 0.6759259259259259300, 0.6777777777777778123, 0.6796296296296295836, 0.6814814814814814659, 0.6833333333333333481, 0.6851851851851852304, 0.6870370370370370017, 0.6888888888888888840, 0.6907407407407407662, 0.6925925925925925375, 0.6944444444444444198, 0.6962962962962963021, 0.6981481481481481843, 0.6999999999999999556, 0.7018518518518518379, 0.7037037037037037202, 0.7055555555555556024, 0.7074074074074073737, 0.7092592592592592560, 0.7111111111111111382, 0.7129629629629629095, 0.7148148148148147918, 0.7166666666666666741, 0.7185185185185185563, 0.7203703703703703276, 0.7222222222222222099, 0.7240740740740740922, 0.7259259259259259744, 0.7277777777777777457, 0.7296296296296296280, 0.7314814814814815103, 0.7333333333333332815, 0.7351851851851851638, 0.7370370370370370461, 0.7388888888888889284, 0.7407407407407406996, 0.7425925925925925819, 0.7444444444444444642, 0.7462962962962963465, 0.7481481481481481177, 0.7500000000000000000, 0.7518518518518518823, 0.7537037037037036535, 0.7555555555555555358, 0.7574074074074074181, 0.7592592592592593004, 0.7611111111111110716, 0.7629629629629629539, 0.7648148148148148362, 0.7666666666666667185, 0.7685185185185184897, 0.7703703703703703720, 0.7722222222222222543, 0.7740740740740740256, 0.7759259259259259078, 0.7777777777777777901, 0.7796296296296296724, 0.7814814814814814437, 0.7833333333333333259, 0.7851851851851852082, 0.7870370370370370905, 0.7888888888888888618, 0.7907407407407407440, 0.7925925925925926263, 0.7944444444444443976, 0.7962962962962962798, 0.7981481481481481621, 0.8000000000000000444, 0.8018518518518518157, 0.8037037037037036979, 0.8055555555555555802, 0.8074074074074074625, 0.8092592592592592338, 0.8111111111111111160, 0.8129629629629629983, 0.8148148148148147696, 0.8166666666666666519, 0.8185185185185185341, 0.8203703703703704164, 0.8222222222222221877, 0.8240740740740740700, 0.8259259259259259522, 0.8277777777777777235, 0.8296296296296296058, 0.8314814814814814881, 0.8333333333333333703, 0.8351851851851851416, 0.8370370370370370239, 0.8388888888888889062, 0.8407407407407407884, 0.8425925925925925597, 0.8444444444444444420, 0.8462962962962963243, 0.8481481481481480955, 0.8499999999999999778, 0.8518518518518518601, 0.8537037037037037424, 0.8555555555555555136, 0.8574074074074073959, 0.8592592592592592782, 0.8611111111111111605, 0.8629629629629629317, 0.8648148148148148140, 0.8666666666666666963, 0.8685185185185184675, 0.8703703703703703498, 0.8722222222222222321, 0.8740740740740741144, 0.8759259259259258856, 0.8777777777777777679, 0.8796296296296296502, 0.8814814814814815325, 0.8833333333333333037, 0.8851851851851851860, 0.8870370370370370683, 0.8888888888888888395, 0.8907407407407407218, 0.8925925925925926041, 0.8944444444444444864, 0.8962962962962962576, 0.8981481481481481399, 0.9000000000000000222, 0.9018518518518519045, 0.9037037037037036757, 0.9055555555555555580, 0.9074074074074074403, 0.9092592592592592116, 0.9111111111111110938, 0.9129629629629629761, 0.9148148148148148584, 0.9166666666666666297, 0.9185185185185185119, 0.9203703703703703942, 0.9222222222222222765, 0.9240740740740740478, 0.9259259259259259300, 0.9277777777777778123, 0.9296296296296295836, 0.9314814814814814659, 0.9333333333333333481, 0.9351851851851852304, 0.9370370370370370017, 0.9388888888888888840, 0.9407407407407407662, 0.9425925925925925375, 0.9444444444444444198, 0.9462962962962963021, 0.9481481481481481843, 0.9499999999999999556, 0.9518518518518518379, 0.9537037037037037202, 0.9555555555555556024, 0.9574074074074073737, 0.9592592592592592560, 0.9611111111111111382, 0.9629629629629629095, 0.9648148148148147918, 0.9666666666666666741, 0.9685185185185185563, 0.9703703703703703276, 0.9722222222222222099, 0.9740740740740740922, 0.9759259259259259744, 0.9777777777777777457, 0.9796296296296296280, 0.9814814814814815103, 0.9833333333333332815, 0.9851851851851851638, 0.9870370370370370461, 0.9888888888888889284, 0.9907407407407406996, 0.9925925925925925819, 0.9944444444444444642, 0.9962962962962963465, 0.9981481481481481177, 1.000000000000000000 ),
 .UNSPECIFIED. ) 
 GEOMETRIC_REPRESENTATION_ITEM ( )  RATIONAL_B_SPLINE_SURFACE ( (
 ( 1.000000000000000000, 0.8660254037844387076, 1.000000000000000000, 0.8660254037844387076, 1.000000000000000000, 0.8660254037844387076, 1.000000000000000000, 0.8660254037844387076, 1.000000000000000000, 0.8660254037844387076, 1.000000000000000000, 0.8660254037844387076, 1.000000000000000000, 0.8660254037844387076, 1.000000000000000000, 0.8660254037844387076, 1.000000000000000000, 0.8660254037844387076, 1.000000000000000000, 0.8660254037844387076, 1.000000000000000000, 0.8660254037844387076, 1.000000000000000000, 0.8660254037844387076, 1.000000000000000000, 0.8660254037844387076, 1.000000000000000000, 0.8660254037844387076, 1.000000000000000000, 0.8660254037844387076, 1.000000000000000000, 0.8660254037844387076, 1.000000000000000000, 0.8660254037844387076, 1.000000000000000000, 0.8660254037844387076, 1.000000000000000000, 0.8660254037844387076, 1.000000000000000000, 0.8660254037844387076, 1.000000000000000000, 0.8660254037844387076, 1.000000000000000000, 0.8660254037844387076, 1.000000000000000000, 0.8660254037844387076, 1.000000000000000000, 0.8660254037844387076, 1.000000000000000000, 0.8660254037844387076, 1.000000000000000000, 0.8660254037844387076, 1.000000000000000000, 0.8660254037844387076, 1.000000000000000000, 0.8660254037844387076, 1.000000000000000000, 0.8660254037844387076, 1.000000000000000000, 0.8660254037844387076, 1.000000000000000000, 0.8660254037844387076, 1.000000000000000000, 0.8660254037844387076, 1.000000000000000000, 0.8660254037844387076, 1.000000000000000000, 0.8660254037844387076, 1.000000000000000000, 0.8660254037844387076, 1.000000000000000000, 0.8660254037844387076, 1.000000000000000000, 0.8660254037844387076, 1.000000000000000000, 0.8660254037844387076, 1.000000000000000000, 0.8660254037844387076, 1.000000000000000000, 0.8660254037844387076, 1.000000000000000000, 0.8660254037844387076, 1.000000000000000000, 0.8660254037844387076, 1.000000000000000000, 0.8660254037844387076, 1.000000000000000000, 0.8660254037844387076, 1.000000000000000000, 0.8660254037844387076, 1.000000000000000000, 0.8660254037844387076, 1.000000000000000000, 0.8660254037844387076, 1.000000000000000000, 0.8660254037844387076, 1.000000000000000000, 0.8660254037844387076, 1.000000000000000000, 0.8660254037844387076, 1.000000000000000000, 0.8660254037844387076, 1.000000000000000000, 0.8660254037844387076, 1.000000000000000000, 0.8660254037844387076, 1.000000000000000000, 0.8660254037844387076, 1.000000000000000000, 0.8660254037844387076, 1.000000000000000000, 0.8660254037844387076, 1.000000000000000000, 0.8660254037844387076, 1.000000000000000000, 0.8660254037844387076, 1.000000000000000000, 0.8660254037844387076, 1.000000000000000000, 0.8660254037844387076, 1.000000000000000000, 0.8660254037844387076, 1.000000000000000000, 0.8660254037844387076, 1.000000000000000000, 0.8660254037844387076, 1.000000000000000000, 0.8660254037844387076, 1.000000000000000000, 0.8660254037844387076, 1.000000000000000000, 0.8660254037844387076, 1.000000000000000000, 0.8660254037844387076, 1.000000000000000000, 0.8660254037844387076, 1.000000000000000000, 0.8660254037844387076, 1.000000000000000000, 0.8660254037844387076, 1.000000000000000000, 0.8660254037844387076, 1.000000000000000000, 0.8660254037844387076, 1.000000000000000000, 0.8660254037844387076, 1.000000000000000000, 0.8660254037844387076, 1.000000000000000000, 0.8660254037844387076, 1.000000000000000000, 0.8660254037844387076, 1.000000000000000000, 0.8660254037844387076, 1.000000000000000000, 0.8660254037844387076, 1.000000000000000000, 0.8660254037844387076, 1.000000000000000000, 0.8660254037844387076, 1.000000000000000000, 0.8660254037844387076, 1.000000000000000000, 0.8660254037844387076, 1.000000000000000000, 0.8660254037844387076, 1.000000000000000000, 0.8660254037844387076, 1.000000000000000000, 0.8660254037844387076, 1.000000000000000000, 0.8660254037844387076, 1.000000000000000000, 0.8660254037844387076, 1.000000000000000000, 0.8660254037844387076, 1.000000000000000000, 0.8660254037844387076, 1.000000000000000000, 0.8660254037844387076, 1.000000000000000000, 0.8660254037844387076, 1.000000000000000000, 0.8660254037844387076, 1.000000000000000000, 0.8660254037844387076, 1.000000000000000000, 0.8660254037844387076, 1.000000000000000000, 0.8660254037844387076, 1.000000000000000000, 0.8660254037844387076, 1.000000000000000000, 0.8660254037844387076, 1.000000000000000000, 0.8660254037844387076, 1.000000000000000000, 0.8660254037844387076, 1.000000000000000000, 0.8660254037844387076, 1.000000000000000000, 0.8660254037844387076, 1.000000000000000000, 0.8660254037844387076, 1.000000000000000000, 0.8660254037844387076, 1.000000000000000000, 0.8660254037844387076, 1.000000000000000000, 0.8660254037844387076, 1.000000000000000000, 0.8660254037844387076, 1.000000000000000000, 0.8660254037844387076, 1.000000000000000000, 0.8660254037844387076, 1.000000000000000000, 0.8660254037844387076, 1.000000000000000000, 0.8660254037844387076, 1.000000000000000000, 0.8660254037844387076, 1.000000000000000000, 0.8660254037844387076, 1.000000000000000000, 0.8660254037844387076, 1.000000000000000000, 0.8660254037844387076, 1.000000000000000000, 0.8660254037844387076, 1.000000000000000000, 0.8660254037844387076, 1.000000000000000000, 0.8660254037844387076, 1.000000000000000000, 0.8660254037844387076, 1.000000000000000000, 0.8660254037844387076, 1.000000000000000000, 0.8660254037844387076, 1.000000000000000000, 0.8660254037844387076, 1.000000000000000000, 0.8660254037844387076, 1.000000000000000000, 0.8660254037844387076, 1.000000000000000000, 0.8660254037844387076, 1.000000000000000000, 0.8660254037844387076, 1.000000000000000000, 0.8660254037844387076, 1.000000000000000000, 0.8660254037844387076, 1.000000000000000000, 0.8660254037844387076, 1.000000000000000000, 0.8660254037844387076, 1.000000000000000000, 0.8660254037844387076, 1.000000000000000000, 0.8660254037844387076, 1.000000000000000000, 0.8660254037844387076, 1.000000000000000000, 0.8660254037844387076, 1.000000000000000000, 0.8660254037844387076, 1.000000000000000000, 0.8660254037844387076, 1.000000000000000000, 0.8660254037844387076, 1.000000000000000000, 0.8660254037844387076, 1.000000000000000000, 0.8660254037844387076, 1.000000000000000000, 0.8660254037844387076, 1.000000000000000000, 0.8660254037844387076, 1.000000000000000000, 0.8660254037844387076, 1.000000000000000000, 0.8660254037844387076, 1.000000000000000000, 0.8660254037844387076, 1.000000000000000000, 0.8660254037844387076, 1.000000000000000000, 0.8660254037844387076, 1.000000000000000000, 0.8660254037844387076, 1.000000000000000000, 0.8660254037844387076, 1.000000000000000000, 0.8660254037844387076, 1.000000000000000000, 0.8660254037844387076, 1.000000000000000000, 0.8660254037844387076, 1.000000000000000000, 0.8660254037844387076, 1.000000000000000000, 0.8660254037844387076, 1.000000000000000000, 0.8660254037844387076, 1.000000000000000000, 0.8660254037844387076, 1.000000000000000000, 0.8660254037844387076, 1.000000000000000000, 0.8660254037844387076, 1.000000000000000000, 0.8660254037844387076, 1.000000000000000000, 0.8660254037844387076, 1.000000000000000000, 0.8660254037844387076, 1.000000000000000000, 0.8660254037844387076, 1.000000000000000000, 0.8660254037844387076, 1.000000000000000000, 0.8660254037844387076, 1.000000000000000000, 0.8660254037844387076, 1.000000000000000000, 0.8660254037844387076, 1.000000000000000000, 0.8660254037844387076, 1.000000000000000000, 0.8660254037844387076, 1.000000000000000000, 0.8660254037844387076, 1.000000000000000000, 0.8660254037844387076, 1.000000000000000000, 0.8660254037844387076, 1.000000000000000000, 0.8660254037844387076, 1.000000000000000000, 0.8660254037844387076, 1.000000000000000000, 0.8660254037844387076, 1.000000000000000000, 0.8660254037844387076, 1.000000000000000000, 0.8660254037844387076, 1.000000000000000000, 0.8660254037844387076, 1.000000000000000000, 0.8660254037844387076, 1.000000000000000000, 0.8660254037844387076, 1.000000000000000000, 0.8660254037844387076, 1.000000000000000000, 0.8660254037844387076, 1.000000000000000000, 0.8660254037844387076, 1.000000000000000000, 0.8660254037844387076, 1.000000000000000000, 0.8660254037844387076, 1.000000000000000000, 0.8660254037844387076, 1.000000000000000000, 0.8660254037844387076, 1.000000000000000000, 0.8660254037844387076, 1.000000000000000000, 0.8660254037844387076, 1.000000000000000000, 0.8660254037844387076, 1.000000000000000000, 0.8660254037844387076, 1.000000000000000000, 0.8660254037844387076, 1.000000000000000000, 0.8660254037844387076, 1.000000000000000000, 0.8660254037844387076, 1.000000000000000000, 0.8660254037844387076, 1.000000000000000000, 0.8660254037844387076, 1.000000000000000000, 0.8660254037844387076, 1.000000000000000000, 0.8660254037844387076, 1.000000000000000000, 0.8660254037844387076, 1.000000000000000000, 0.8660254037844387076, 1.000000000000000000, 0.8660254037844387076, 1.000000000000000000, 0.8660254037844387076, 1.000000000000000000, 0.8660254037844387076, 1.000000000000000000, 0.8660254037844387076, 1.000000000000000000, 0.8660254037844387076, 1.000000000000000000, 0.8660254037844387076, 1.000000000000000000, 0.8660254037844387076, 1.000000000000000000, 0.8660254037844387076, 1.000000000000000000, 0.8660254037844387076, 1.000000000000000000, 0.8660254037844387076, 1.000000000000000000, 0.8660254037844387076, 1.000000000000000000, 0.8660254037844387076, 1.000000000000000000, 0.8660254037844387076, 1.000000000000000000, 0.8660254037844387076, 1.000000000000000000, 0.8660254037844387076, 1.000000000000000000, 0.8660254037844387076, 1.000000000000000000, 0.8660254037844387076, 1.000000000000000000, 0.8660254037844387076, 1.000000000000000000, 0.8660254037844387076, 1.000000000000000000, 0.8660254037844387076, 1.000000000000000000, 0.8660254037844387076, 1.000000000000000000, 0.8660254037844387076, 1.000000000000000000, 0.8660254037844387076, 1.000000000000000000, 0.8660254037844387076, 1.000000000000000000, 0.8660254037844387076, 1.000000000000000000, 0.8660254037844387076, 1.000000000000000000, 0.8660254037844387076, 1.000000000000000000, 0.8660254037844387076, 1.000000000000000000, 0.8660254037844387076, 1.000000000000000000, 0.8660254037844387076, 1.000000000000000000, 0.8660254037844387076, 1.000000000000000000, 0.8660254037844387076, 1.000000000000000000, 0.8660254037844387076, 1.000000000000000000, 0.8660254037844387076, 1.000000000000000000, 0.8660254037844387076, 1.000000000000000000, 0.8660254037844387076, 1.000000000000000000, 0.8660254037844387076, 1.000000000000000000, 0.8660254037844387076, 1.000000000000000000, 0.8660254037844387076, 1.000000000000000000, 0.8660254037844387076, 1.000000000000000000, 0.8660254037844387076, 1.000000000000000000, 0.8660254037844387076, 1.000000000000000000, 0.8660254037844387076, 1.000000000000000000, 0.8660254037844387076, 1.000000000000000000, 0.8660254037844387076, 1.000000000000000000, 0.8660254037844387076, 1.000000000000000000, 0.8660254037844387076, 1.000000000000000000, 0.8660254037844387076, 1.000000000000000000, 0.8660254037844387076, 1.000000000000000000, 0.8660254037844387076, 1.000000000000000000, 0.8660254037844387076, 1.000000000000000000, 0.8660254037844387076, 1.000000000000000000, 0.8660254037844387076, 1.000000000000000000, 0.8660254037844387076, 1.000000000000000000, 0.8660254037844387076, 1.000000000000000000, 0.8660254037844387076, 1.000000000000000000, 0.8660254037844387076, 1.000000000000000000, 0.8660254037844387076, 1.000000000000000000, 0.8660254037844387076, 1.000000000000000000, 0.8660254037844387076, 1.000000000000000000, 0.8660254037844387076, 1.000000000000000000, 0.8660254037844387076, 1.000000000000000000, 0.8660254037844387076, 1.000000000000000000, 0.8660254037844387076, 1.000000000000000000, 0.8660254037844387076, 1.000000000000000000, 0.8660254037844387076, 1.000000000000000000, 0.8660254037844387076, 1.000000000000000000, 0.8660254037844387076, 1.000000000000000000, 0.8660254037844387076, 1.000000000000000000, 0.8660254037844387076, 1.000000000000000000, 0.8660254037844387076, 1.000000000000000000, 0.8660254037844387076, 1.000000000000000000, 0.8660254037844387076, 1.000000000000000000, 0.8660254037844387076, 1.000000000000000000, 0.8660254037844387076, 1.000000000000000000, 0.8660254037844387076, 1.000000000000000000, 0.8660254037844387076, 1.000000000000000000, 0.8660254037844387076, 1.000000000000000000, 0.8660254037844387076, 1.000000000000000000, 0.8660254037844387076, 1.000000000000000000, 0.8660254037844387076, 1.000000000000000000, 0.8660254037844387076, 1.000000000000000000, 0.8660254037844387076, 1.000000000000000000, 0.8660254037844387076, 1.000000000000000000, 0.8660254037844387076, 1.000000000000000000, 0.8660254037844387076, 1.000000000000000000, 0.8660254037844387076, 1.000000000000000000, 0.8660254037844387076, 1.000000000000000000, 0.8660254037844387076, 1.000000000000000000, 0.8660254037844387076, 1.000000000000000000, 0.8660254037844387076, 1.000000000000000000, 0.8660254037844387076, 1.000000000000000000, 0.8660254037844387076, 1.000000000000000000, 0.8660254037844387076, 1.000000000000000000, 0.8660254037844387076, 1.000000000000000000, 0.8660254037844387076, 1.000000000000000000, 0.8660254037844387076, 1.000000000000000000, 0.8660254037844387076, 1.000000000000000000, 0.8660254037844387076, 1.000000000000000000, 0.8660254037844387076, 1.000000000000000000, 0.8660254037844387076, 1.000000000000000000, 0.8660254037844387076, 1.000000000000000000, 0.8660254037844387076, 1.000000000000000000, 0.8660254037844387076, 1.000000000000000000, 0.8660254037844387076, 1.000000000000000000, 0.8660254037844387076, 1.000000000000000000, 0.8660254037844387076, 1.000000000000000000, 0.8660254037844387076, 1.000000000000000000, 0.8660254037844387076, 1.000000000000000000, 0.8660254037844387076, 1.000000000000000000, 0.8660254037844387076, 1.000000000000000000, 0.8660254037844387076, 1.000000000000000000, 0.8660254037844387076, 1.000000000000000000, 0.8660254037844387076, 1.000000000000000000, 0.8660254037844387076, 1.000000000000000000, 0.8660254037844387076, 1.000000000000000000, 0.8660254037844387076, 1.000000000000000000, 0.8660254037844387076, 1.000000000000000000, 0.8660254037844387076, 1.000000000000000000, 0.8660254037844387076, 1.000000000000000000, 0.8660254037844387076, 1.000000000000000000, 0.8660254037844387076, 1.000000000000000000, 0.8660254037844387076, 1.000000000000000000, 0.8660254037844387076, 1.000000000000000000, 0.8660254037844387076, 1.000000000000000000, 0.8660254037844387076, 1.000000000000000000, 0.8660254037844387076, 1.000000000000000000, 0.8660254037844387076, 1.000000000000000000, 0.8660254037844387076, 1.000000000000000000, 0.8660254037844387076, 1.000000000000000000, 0.8660254037844387076, 1.000000000000000000, 0.8660254037844387076, 1.000000000000000000, 0.8660254037844387076, 1.000000000000000000, 0.8660254037844387076, 1.000000000000000000, 0.8660254037844387076, 1.000000000000000000, 0.8660254037844387076, 1.000000000000000000, 0.8660254037844387076, 1.000000000000000000, 0.8660254037844387076, 1.000000000000000000, 0.8660254037844387076, 1.000000000000000000, 0.8660254037844387076, 1.000000000000000000, 0.8660254037844387076, 1.000000000000000000, 0.8660254037844387076, 1.000000000000000000, 0.8660254037844387076, 1.000000000000000000, 0.8660254037844387076, 1.000000000000000000, 0.8660254037844387076, 1.000000000000000000, 0.8660254037844387076, 1.000000000000000000, 0.8660254037844387076, 1.000000000000000000, 0.8660254037844387076, 1.000000000000000000, 0.8660254037844387076, 1.000000000000000000, 0.8660254037844387076, 1.000000000000000000, 0.8660254037844387076, 1.000000000000000000, 0.8660254037844387076, 1.000000000000000000, 0.8660254037844387076, 1.000000000000000000, 0.8660254037844387076, 1.000000000000000000, 0.8660254037844387076, 1.000000000000000000, 0.8660254037844387076, 1.000000000000000000, 0.8660254037844387076, 1.000000000000000000, 0.8660254037844387076, 1.000000000000000000, 0.8660254037844387076, 1.000000000000000000, 0.8660254037844387076, 1.000000000000000000, 0.8660254037844387076, 1.000000000000000000, 0.8660254037844387076, 1.000000000000000000, 0.8660254037844387076, 1.000000000000000000, 0.8660254037844387076, 1.000000000000000000, 0.8660254037844387076, 1.000000000000000000, 0.8660254037844387076, 1.000000000000000000, 0.8660254037844387076, 1.000000000000000000, 0.8660254037844387076, 1.000000000000000000, 0.8660254037844387076, 1.000000000000000000, 0.8660254037844387076, 1.000000000000000000, 0.8660254037844387076, 1.000000000000000000, 0.8660254037844387076, 1.000000000000000000, 0.8660254037844387076, 1.000000000000000000, 0.8660254037844387076, 1.000000000000000000, 0.8660254037844387076, 1.000000000000000000, 0.8660254037844387076, 1.000000000000000000, 0.8660254037844387076, 1.000000000000000000, 0.8660254037844387076, 1.000000000000000000, 0.8660254037844387076, 1.000000000000000000, 0.8660254037844387076, 1.000000000000000000, 0.8660254037844387076, 1.000000000000000000, 0.8660254037844387076, 1.000000000000000000, 0.8660254037844387076, 1.000000000000000000, 0.8660254037844387076, 1.000000000000000000, 0.8660254037844387076, 1.000000000000000000, 0.8660254037844387076, 1.000000000000000000, 0.8660254037844387076, 1.000000000000000000, 0.8660254037844387076, 1.000000000000000000, 0.8660254037844387076, 1.000000000000000000, 0.8660254037844387076, 1.000000000000000000, 0.8660254037844387076, 1.000000000000000000, 0.8660254037844387076, 1.000000000000000000, 0.8660254037844387076, 1.000000000000000000, 0.8660254037844387076, 1.000000000000000000, 0.8660254037844387076, 1.000000000000000000, 0.8660254037844387076, 1.000000000000000000, 0.8660254037844387076, 1.000000000000000000, 0.8660254037844387076, 1.000000000000000000, 0.8660254037844387076, 1.000000000000000000, 0.8660254037844387076, 1.000000000000000000, 0.8660254037844387076, 1.000000000000000000, 0.8660254037844387076, 1.000000000000000000, 0.8660254037844387076, 1.000000000000000000, 0.8660254037844387076, 1.000000000000000000, 0.8660254037844387076, 1.000000000000000000, 0.8660254037844387076, 1.000000000000000000, 0.8660254037844387076, 1.000000000000000000, 0.8660254037844387076, 1.000000000000000000, 0.8660254037844387076, 1.000000000000000000, 0.8660254037844387076, 1.000000000000000000, 0.8660254037844387076, 1.000000000000000000, 0.8660254037844387076, 1.000000000000000000, 0.8660254037844387076, 1.000000000000000000, 0.8660254037844387076, 1.000000000000000000, 0.8660254037844387076, 1.000000000000000000, 0.8660254037844387076, 1.000000000000000000, 0.8660254037844387076, 1.000000000000000000, 0.8660254037844387076, 1.000000000000000000, 0.8660254037844387076, 1.000000000000000000, 0.8660254037844387076, 1.000000000000000000, 0.8660254037844387076, 1.000000000000000000, 0.8660254037844387076, 1.000000000000000000, 0.8660254037844387076, 1.000000000000000000, 0.8660254037844387076, 1.000000000000000000, 0.8660254037844387076, 1.000000000000000000, 0.8660254037844387076, 1.000000000000000000, 0.8660254037844387076, 1.000000000000000000, 0.8660254037844387076, 1.000000000000000000, 0.8660254037844387076, 1.000000000000000000, 0.8660254037844387076, 1.000000000000000000, 0.8660254037844387076, 1.000000000000000000, 0.8660254037844387076, 1.000000000000000000, 0.8660254037844387076, 1.000000000000000000, 0.8660254037844387076, 1.000000000000000000, 0.8660254037844387076, 1.000000000000000000, 0.8660254037844387076, 1.000000000000000000, 0.8660254037844387076, 1.000000000000000000, 0.8660254037844387076, 1.000000000000000000, 0.8660254037844387076, 1.000000000000000000, 0.8660254037844387076, 1.000000000000000000, 0.8660254037844387076, 1.000000000000000000, 0.8660254037844387076, 1.000000000000000000, 0.8660254037844387076, 1.000000000000000000, 0.8660254037844387076, 1.000000000000000000, 0.8660254037844387076, 1.000000000000000000, 0.8660254037844387076, 1.000000000000000000, 0.8660254037844387076, 1.000000000000000000, 0.8660254037844387076, 1.000000000000000000, 0.8660254037844387076, 1.000000000000000000, 0.8660254037844387076, 1.000000000000000000, 0.8660254037844387076, 1.000000000000000000, 0.8660254037844387076, 1.000000000000000000, 0.8660254037844387076, 1.000000000000000000, 0.8660254037844387076, 1.000000000000000000, 0.8660254037844387076, 1.000000000000000000, 0.8660254037844387076, 1.000000000000000000, 0.8660254037844387076, 1.000000000000000000, 0.8660254037844387076, 1.000000000000000000, 0.8660254037844387076, 1.000000000000000000, 0.8660254037844387076, 1.000000000000000000, 0.8660254037844387076, 1.000000000000000000, 0.8660254037844387076, 1.000000000000000000, 0.8660254037844387076, 1.000000000000000000, 0.8660254037844387076, 1.000000000000000000, 0.8660254037844387076, 1.000000000000000000, 0.8660254037844387076, 1.000000000000000000, 0.8660254037844387076, 1.000000000000000000, 0.8660254037844387076, 1.000000000000000000, 0.8660254037844387076, 1.000000000000000000, 0.8660254037844387076, 1.000000000000000000, 0.8660254037844387076, 1.000000000000000000, 0.8660254037844387076, 1.000000000000000000, 0.8660254037844387076, 1.000000000000000000, 0.8660254037844387076, 1.000000000000000000, 0.8660254037844387076, 1.000000000000000000, 0.8660254037844387076, 1.000000000000000000, 0.8660254037844387076, 1.000000000000000000, 0.8660254037844387076, 1.000000000000000000, 0.8660254037844387076, 1.000000000000000000, 0.8660254037844387076, 1.000000000000000000, 0.8660254037844387076, 1.000000000000000000, 0.8660254037844387076, 1.000000000000000000, 0.8660254037844387076, 1.000000000000000000, 0.8660254037844387076, 1.000000000000000000, 0.8660254037844387076, 1.000000000000000000, 0.8660254037844387076, 1.000000000000000000, 0.8660254037844387076, 1.000000000000000000, 0.8660254037844387076, 1.000000000000000000, 0.8660254037844387076, 1.000000000000000000, 0.8660254037844387076, 1.000000000000000000, 0.8660254037844387076, 1.000000000000000000, 0.8660254037844387076, 1.000000000000000000, 0.8660254037844387076, 1.000000000000000000, 0.8660254037844387076, 1.000000000000000000, 0.8660254037844387076, 1.000000000000000000, 0.8660254037844387076, 1.000000000000000000, 0.8660254037844387076, 1.000000000000000000, 0.8660254037844387076, 1.000000000000000000, 0.8660254037844387076, 1.000000000000000000, 0.8660254037844387076, 1.000000000000000000, 0.8660254037844387076, 1.000000000000000000, 0.8660254037844387076, 1.000000000000000000, 0.8660254037844387076, 1.000000000000000000, 0.8660254037844387076, 1.000000000000000000, 0.8660254037844387076, 1.000000000000000000, 0.8660254037844387076, 1.000000000000000000, 0.8660254037844387076, 1.000000000000000000, 0.8660254037844387076, 1.000000000000000000, 0.8660254037844387076, 1.000000000000000000, 0.8660254037844387076, 1.000000000000000000, 0.8660254037844387076, 1.000000000000000000, 0.8660254037844387076, 1.000000000000000000, 0.8660254037844387076, 1.000000000000000000, 0.8660254037844387076, 1.000000000000000000, 0.8660254037844387076, 1.000000000000000000, 0.8660254037844387076, 1.000000000000000000, 0.8660254037844387076, 1.000000000000000000, 0.8660254037844387076, 1.000000000000000000, 0.8660254037844387076, 1.000000000000000000, 0.8660254037844387076, 1.000000000000000000, 0.8660254037844387076, 1.000000000000000000, 0.8660254037844387076, 1.000000000000000000, 0.8660254037844387076, 1.000000000000000000, 0.8660254037844387076, 1.000000000000000000, 0.8660254037844387076, 1.000000000000000000, 0.8660254037844387076, 1.000000000000000000, 0.8660254037844387076, 1.000000000000000000, 0.8660254037844387076, 1.000000000000000000, 0.8660254037844387076, 1.000000000000000000, 0.8660254037844387076, 1.000000000000000000, 0.8660254037844387076, 1.000000000000000000, 0.8660254037844387076, 1.000000000000000000, 0.8660254037844387076, 1.000000000000000000, 0.8660254037844387076, 1.000000000000000000, 0.8660254037844387076, 1.000000000000000000, 0.8660254037844387076, 1.000000000000000000, 0.8660254037844387076, 1.000000000000000000, 0.8660254037844387076, 1.000000000000000000, 0.8660254037844387076, 1.000000000000000000, 0.8660254037844387076, 1.000000000000000000, 0.8660254037844387076, 1.000000000000000000, 0.8660254037844387076, 1.000000000000000000, 0.8660254037844387076, 1.000000000000000000),
 ( 1.000000000000000000, 0.8660254037844387076, 1.000000000000000000, 0.8660254037844387076, 1.000000000000000000, 0.8660254037844387076, 1.000000000000000000, 0.8660254037844387076, 1.000000000000000000, 0.8660254037844387076, 1.000000000000000000, 0.8660254037844387076, 1.000000000000000000, 0.8660254037844387076, 1.000000000000000000, 0.8660254037844387076, 1.000000000000000000, 0.8660254037844387076, 1.000000000000000000, 0.8660254037844387076, 1.000000000000000000, 0.8660254037844387076, 1.000000000000000000, 0.8660254037844387076, 1.000000000000000000, 0.8660254037844387076, 1.000000000000000000, 0.8660254037844387076, 1.000000000000000000, 0.8660254037844387076, 1.000000000000000000, 0.8660254037844387076, 1.000000000000000000, 0.8660254037844387076, 1.000000000000000000, 0.8660254037844387076, 1.000000000000000000, 0.8660254037844387076, 1.000000000000000000, 0.8660254037844387076, 1.000000000000000000, 0.8660254037844387076, 1.000000000000000000, 0.8660254037844387076, 1.000000000000000000, 0.8660254037844387076, 1.000000000000000000, 0.8660254037844387076, 1.000000000000000000, 0.8660254037844387076, 1.000000000000000000, 0.8660254037844387076, 1.000000000000000000, 0.8660254037844387076, 1.000000000000000000, 0.8660254037844387076, 1.000000000000000000, 0.8660254037844387076, 1.000000000000000000, 0.8660254037844387076, 1.000000000000000000, 0.8660254037844387076, 1.000000000000000000, 0.8660254037844387076, 1.000000000000000000, 0.8660254037844387076, 1.000000000000000000, 0.8660254037844387076, 1.000000000000000000, 0.8660254037844387076, 1.000000000000000000, 0.8660254037844387076, 1.000000000000000000, 0.8660254037844387076, 1.000000000000000000, 0.8660254037844387076, 1.000000000000000000, 0.8660254037844387076, 1.000000000000000000, 0.8660254037844387076, 1.000000000000000000, 0.8660254037844387076, 1.000000000000000000, 0.8660254037844387076, 1.000000000000000000, 0.8660254037844387076, 1.000000000000000000, 0.8660254037844387076, 1.000000000000000000, 0.8660254037844387076, 1.000000000000000000, 0.8660254037844387076, 1.000000000000000000, 0.8660254037844387076, 1.000000000000000000, 0.8660254037844387076, 1.000000000000000000, 0.8660254037844387076, 1.000000000000000000, 0.8660254037844387076, 1.000000000000000000, 0.8660254037844387076, 1.000000000000000000, 0.8660254037844387076, 1.000000000000000000, 0.8660254037844387076, 1.000000000000000000, 0.8660254037844387076, 1.000000000000000000, 0.8660254037844387076, 1.000000000000000000, 0.8660254037844387076, 1.000000000000000000, 0.8660254037844387076, 1.000000000000000000, 0.8660254037844387076, 1.000000000000000000, 0.8660254037844387076, 1.000000000000000000, 0.8660254037844387076, 1.000000000000000000, 0.8660254037844387076, 1.000000000000000000, 0.8660254037844387076, 1.000000000000000000, 0.8660254037844387076, 1.000000000000000000, 0.8660254037844387076, 1.000000000000000000, 0.8660254037844387076, 1.000000000000000000, 0.8660254037844387076, 1.000000000000000000, 0.8660254037844387076, 1.000000000000000000, 0.8660254037844387076, 1.000000000000000000, 0.8660254037844387076, 1.000000000000000000, 0.8660254037844387076, 1.000000000000000000, 0.8660254037844387076, 1.000000000000000000, 0.8660254037844387076, 1.000000000000000000, 0.8660254037844387076, 1.000000000000000000, 0.8660254037844387076, 1.000000000000000000, 0.8660254037844387076, 1.000000000000000000, 0.8660254037844387076, 1.000000000000000000, 0.8660254037844387076, 1.000000000000000000, 0.8660254037844387076, 1.000000000000000000, 0.8660254037844387076, 1.000000000000000000, 0.8660254037844387076, 1.000000000000000000, 0.8660254037844387076, 1.000000000000000000, 0.8660254037844387076, 1.000000000000000000, 0.8660254037844387076, 1.000000000000000000, 0.8660254037844387076, 1.000000000000000000, 0.8660254037844387076, 1.000000000000000000, 0.8660254037844387076, 1.000000000000000000, 0.8660254037844387076, 1.000000000000000000, 0.8660254037844387076, 1.000000000000000000, 0.8660254037844387076, 1.000000000000000000, 0.8660254037844387076, 1.000000000000000000, 0.8660254037844387076, 1.000000000000000000, 0.8660254037844387076, 1.000000000000000000, 0.8660254037844387076, 1.000000000000000000, 0.8660254037844387076, 1.000000000000000000, 0.8660254037844387076, 1.000000000000000000, 0.8660254037844387076, 1.000000000000000000, 0.8660254037844387076, 1.000000000000000000, 0.8660254037844387076, 1.000000000000000000, 0.8660254037844387076, 1.000000000000000000, 0.8660254037844387076, 1.000000000000000000, 0.8660254037844387076, 1.000000000000000000, 0.8660254037844387076, 1.000000000000000000, 0.8660254037844387076, 1.000000000000000000, 0.8660254037844387076, 1.000000000000000000, 0.8660254037844387076, 1.000000000000000000, 0.8660254037844387076, 1.000000000000000000, 0.8660254037844387076, 1.000000000000000000, 0.8660254037844387076, 1.000000000000000000, 0.8660254037844387076, 1.000000000000000000, 0.8660254037844387076, 1.000000000000000000, 0.8660254037844387076, 1.000000000000000000, 0.8660254037844387076, 1.000000000000000000, 0.8660254037844387076, 1.000000000000000000, 0.8660254037844387076, 1.000000000000000000, 0.8660254037844387076, 1.000000000000000000, 0.8660254037844387076, 1.000000000000000000, 0.8660254037844387076, 1.000000000000000000, 0.8660254037844387076, 1.000000000000000000, 0.8660254037844387076, 1.000000000000000000, 0.8660254037844387076, 1.000000000000000000, 0.8660254037844387076, 1.000000000000000000, 0.8660254037844387076, 1.000000000000000000, 0.8660254037844387076, 1.000000000000000000, 0.8660254037844387076, 1.000000000000000000, 0.8660254037844387076, 1.000000000000000000, 0.8660254037844387076, 1.000000000000000000, 0.8660254037844387076, 1.000000000000000000, 0.8660254037844387076, 1.000000000000000000, 0.8660254037844387076, 1.000000000000000000, 0.8660254037844387076, 1.000000000000000000, 0.8660254037844387076, 1.000000000000000000, 0.8660254037844387076, 1.000000000000000000, 0.8660254037844387076, 1.000000000000000000, 0.8660254037844387076, 1.000000000000000000, 0.8660254037844387076, 1.000000000000000000, 0.8660254037844387076, 1.000000000000000000, 0.8660254037844387076, 1.000000000000000000, 0.8660254037844387076, 1.000000000000000000, 0.8660254037844387076, 1.000000000000000000, 0.8660254037844387076, 1.000000000000000000, 0.8660254037844387076, 1.000000000000000000, 0.8660254037844387076, 1.000000000000000000, 0.8660254037844387076, 1.000000000000000000, 0.8660254037844387076, 1.000000000000000000, 0.8660254037844387076, 1.000000000000000000, 0.8660254037844387076, 1.000000000000000000, 0.8660254037844387076, 1.000000000000000000, 0.8660254037844387076, 1.000000000000000000, 0.8660254037844387076, 1.000000000000000000, 0.8660254037844387076, 1.000000000000000000, 0.8660254037844387076, 1.000000000000000000, 0.8660254037844387076, 1.000000000000000000, 0.8660254037844387076, 1.000000000000000000, 0.8660254037844387076, 1.000000000000000000, 0.8660254037844387076, 1.000000000000000000, 0.8660254037844387076, 1.000000000000000000, 0.8660254037844387076, 1.000000000000000000, 0.8660254037844387076, 1.000000000000000000, 0.8660254037844387076, 1.000000000000000000, 0.8660254037844387076, 1.000000000000000000, 0.8660254037844387076, 1.000000000000000000, 0.8660254037844387076, 1.000000000000000000, 0.8660254037844387076, 1.000000000000000000, 0.8660254037844387076, 1.000000000000000000, 0.8660254037844387076, 1.000000000000000000, 0.8660254037844387076, 1.000000000000000000, 0.8660254037844387076, 1.000000000000000000, 0.8660254037844387076, 1.000000000000000000, 0.8660254037844387076, 1.000000000000000000, 0.8660254037844387076, 1.000000000000000000, 0.8660254037844387076, 1.000000000000000000, 0.8660254037844387076, 1.000000000000000000, 0.8660254037844387076, 1.000000000000000000, 0.8660254037844387076, 1.000000000000000000, 0.8660254037844387076, 1.000000000000000000, 0.8660254037844387076, 1.000000000000000000, 0.8660254037844387076, 1.000000000000000000, 0.8660254037844387076, 1.000000000000000000, 0.8660254037844387076, 1.000000000000000000, 0.8660254037844387076, 1.000000000000000000, 0.8660254037844387076, 1.000000000000000000, 0.8660254037844387076, 1.000000000000000000, 0.8660254037844387076, 1.000000000000000000, 0.8660254037844387076, 1.000000000000000000, 0.8660254037844387076, 1.000000000000000000, 0.8660254037844387076, 1.000000000000000000, 0.8660254037844387076, 1.000000000000000000, 0.8660254037844387076, 1.000000000000000000, 0.8660254037844387076, 1.000000000000000000, 0.8660254037844387076, 1.000000000000000000, 0.8660254037844387076, 1.000000000000000000, 0.8660254037844387076, 1.000000000000000000, 0.8660254037844387076, 1.000000000000000000, 0.8660254037844387076, 1.000000000000000000, 0.8660254037844387076, 1.000000000000000000, 0.8660254037844387076, 1.000000000000000000, 0.8660254037844387076, 1.000000000000000000, 0.8660254037844387076, 1.000000000000000000, 0.8660254037844387076, 1.000000000000000000, 0.8660254037844387076, 1.000000000000000000, 0.8660254037844387076, 1.000000000000000000, 0.8660254037844387076, 1.000000000000000000, 0.8660254037844387076, 1.000000000000000000, 0.8660254037844387076, 1.000000000000000000, 0.8660254037844387076, 1.000000000000000000, 0.8660254037844387076, 1.000000000000000000, 0.8660254037844387076, 1.000000000000000000, 0.8660254037844387076, 1.000000000000000000, 0.8660254037844387076, 1.000000000000000000, 0.8660254037844387076, 1.000000000000000000, 0.8660254037844387076, 1.000000000000000000, 0.8660254037844387076, 1.000000000000000000, 0.8660254037844387076, 1.000000000000000000, 0.8660254037844387076, 1.000000000000000000, 0.8660254037844387076, 1.000000000000000000, 0.8660254037844387076, 1.000000000000000000, 0.8660254037844387076, 1.000000000000000000, 0.8660254037844387076, 1.000000000000000000, 0.8660254037844387076, 1.000000000000000000, 0.8660254037844387076, 1.000000000000000000, 0.8660254037844387076, 1.000000000000000000, 0.8660254037844387076, 1.000000000000000000, 0.8660254037844387076, 1.000000000000000000, 0.8660254037844387076, 1.000000000000000000, 0.8660254037844387076, 1.000000000000000000, 0.8660254037844387076, 1.000000000000000000, 0.8660254037844387076, 1.000000000000000000, 0.8660254037844387076, 1.000000000000000000, 0.8660254037844387076, 1.000000000000000000, 0.8660254037844387076, 1.000000000000000000, 0.8660254037844387076, 1.000000000000000000, 0.8660254037844387076, 1.000000000000000000, 0.8660254037844387076, 1.000000000000000000, 0.8660254037844387076, 1.000000000000000000, 0.8660254037844387076, 1.000000000000000000, 0.8660254037844387076, 1.000000000000000000, 0.8660254037844387076, 1.000000000000000000, 0.8660254037844387076, 1.000000000000000000, 0.8660254037844387076, 1.000000000000000000, 0.8660254037844387076, 1.000000000000000000, 0.8660254037844387076, 1.000000000000000000, 0.8660254037844387076, 1.000000000000000000, 0.8660254037844387076, 1.000000000000000000, 0.8660254037844387076, 1.000000000000000000, 0.8660254037844387076, 1.000000000000000000, 0.8660254037844387076, 1.000000000000000000, 0.8660254037844387076, 1.000000000000000000, 0.8660254037844387076, 1.000000000000000000, 0.8660254037844387076, 1.000000000000000000, 0.8660254037844387076, 1.000000000000000000, 0.8660254037844387076, 1.000000000000000000, 0.8660254037844387076, 1.000000000000000000, 0.8660254037844387076, 1.000000000000000000, 0.8660254037844387076, 1.000000000000000000, 0.8660254037844387076, 1.000000000000000000, 0.8660254037844387076, 1.000000000000000000, 0.8660254037844387076, 1.000000000000000000, 0.8660254037844387076, 1.000000000000000000, 0.8660254037844387076, 1.000000000000000000, 0.8660254037844387076, 1.000000000000000000, 0.8660254037844387076, 1.000000000000000000, 0.8660254037844387076, 1.000000000000000000, 0.8660254037844387076, 1.000000000000000000, 0.8660254037844387076, 1.000000000000000000, 0.8660254037844387076, 1.000000000000000000, 0.8660254037844387076, 1.000000000000000000, 0.8660254037844387076, 1.000000000000000000, 0.8660254037844387076, 1.000000000000000000, 0.8660254037844387076, 1.000000000000000000, 0.8660254037844387076, 1.000000000000000000, 0.8660254037844387076, 1.000000000000000000, 0.8660254037844387076, 1.000000000000000000, 0.8660254037844387076, 1.000000000000000000, 0.8660254037844387076, 1.000000000000000000, 0.8660254037844387076, 1.000000000000000000, 0.8660254037844387076, 1.000000000000000000, 0.8660254037844387076, 1.000000000000000000, 0.8660254037844387076, 1.000000000000000000, 0.8660254037844387076, 1.000000000000000000, 0.8660254037844387076, 1.000000000000000000, 0.8660254037844387076, 1.000000000000000000, 0.8660254037844387076, 1.000000000000000000, 0.8660254037844387076, 1.000000000000000000, 0.8660254037844387076, 1.000000000000000000, 0.8660254037844387076, 1.000000000000000000, 0.8660254037844387076, 1.000000000000000000, 0.8660254037844387076, 1.000000000000000000, 0.8660254037844387076, 1.000000000000000000, 0.8660254037844387076, 1.000000000000000000, 0.8660254037844387076, 1.000000000000000000, 0.8660254037844387076, 1.000000000000000000, 0.8660254037844387076, 1.000000000000000000, 0.8660254037844387076, 1.000000000000000000, 0.8660254037844387076, 1.000000000000000000, 0.8660254037844387076, 1.000000000000000000, 0.8660254037844387076, 1.000000000000000000, 0.8660254037844387076, 1.000000000000000000, 0.8660254037844387076, 1.000000000000000000, 0.8660254037844387076, 1.000000000000000000, 0.8660254037844387076, 1.000000000000000000, 0.8660254037844387076, 1.000000000000000000, 0.8660254037844387076, 1.000000000000000000, 0.8660254037844387076, 1.000000000000000000, 0.8660254037844387076, 1.000000000000000000, 0.8660254037844387076, 1.000000000000000000, 0.8660254037844387076, 1.000000000000000000, 0.8660254037844387076, 1.000000000000000000, 0.8660254037844387076, 1.000000000000000000, 0.8660254037844387076, 1.000000000000000000, 0.8660254037844387076, 1.000000000000000000, 0.8660254037844387076, 1.000000000000000000, 0.8660254037844387076, 1.000000000000000000, 0.8660254037844387076, 1.000000000000000000, 0.8660254037844387076, 1.000000000000000000, 0.8660254037844387076, 1.000000000000000000, 0.8660254037844387076, 1.000000000000000000, 0.8660254037844387076, 1.000000000000000000, 0.8660254037844387076, 1.000000000000000000, 0.8660254037844387076, 1.000000000000000000, 0.8660254037844387076, 1.000000000000000000, 0.8660254037844387076, 1.000000000000000000, 0.8660254037844387076, 1.000000000000000000, 0.8660254037844387076, 1.000000000000000000, 0.8660254037844387076, 1.000000000000000000, 0.8660254037844387076, 1.000000000000000000, 0.8660254037844387076, 1.000000000000000000, 0.8660254037844387076, 1.000000000000000000, 0.8660254037844387076, 1.000000000000000000, 0.8660254037844387076, 1.000000000000000000, 0.8660254037844387076, 1.000000000000000000, 0.8660254037844387076, 1.000000000000000000, 0.8660254037844387076, 1.000000000000000000, 0.8660254037844387076, 1.000000000000000000, 0.8660254037844387076, 1.000000000000000000, 0.8660254037844387076, 1.000000000000000000, 0.8660254037844387076, 1.000000000000000000, 0.8660254037844387076, 1.000000000000000000, 0.8660254037844387076, 1.000000000000000000, 0.8660254037844387076, 1.000000000000000000, 0.8660254037844387076, 1.000000000000000000, 0.8660254037844387076, 1.000000000000000000, 0.8660254037844387076, 1.000000000000000000, 0.8660254037844387076, 1.000000000000000000, 0.8660254037844387076, 1.000000000000000000, 0.8660254037844387076, 1.000000000000000000, 0.8660254037844387076, 1.000000000000000000, 0.8660254037844387076, 1.000000000000000000, 0.8660254037844387076, 1.000000000000000000, 0.8660254037844387076, 1.000000000000000000, 0.8660254037844387076, 1.000000000000000000, 0.8660254037844387076, 1.000000000000000000, 0.8660254037844387076, 1.000000000000000000, 0.8660254037844387076, 1.000000000000000000, 0.8660254037844387076, 1.000000000000000000, 0.8660254037844387076, 1.000000000000000000, 0.8660254037844387076, 1.000000000000000000, 0.8660254037844387076, 1.000000000000000000, 0.8660254037844387076, 1.000000000000000000, 0.8660254037844387076, 1.000000000000000000, 0.8660254037844387076, 1.000000000000000000, 0.8660254037844387076, 1.000000000000000000, 0.8660254037844387076, 1.000000000000000000, 0.8660254037844387076, 1.000000000000000000, 0.8660254037844387076, 1.000000000000000000, 0.8660254037844387076, 1.000000000000000000, 0.8660254037844387076, 1.000000000000000000, 0.8660254037844387076, 1.000000000000000000, 0.8660254037844387076, 1.000000000000000000, 0.8660254037844387076, 1.000000000000000000, 0.8660254037844387076, 1.000000000000000000, 0.8660254037844387076, 1.000000000000000000, 0.8660254037844387076, 1.000000000000000000, 0.8660254037844387076, 1.000000000000000000, 0.8660254037844387076, 1.000000000000000000, 0.8660254037844387076, 1.000000000000000000, 0.8660254037844387076, 1.000000000000000000, 0.8660254037844387076, 1.000000000000000000, 0.8660254037844387076, 1.000000000000000000, 0.8660254037844387076, 1.000000000000000000, 0.8660254037844387076, 1.000000000000000000, 0.8660254037844387076, 1.000000000000000000, 0.8660254037844387076, 1.000000000000000000, 0.8660254037844387076, 1.000000000000000000, 0.8660254037844387076, 1.000000000000000000, 0.8660254037844387076, 1.000000000000000000, 0.8660254037844387076, 1.000000000000000000, 0.8660254037844387076, 1.000000000000000000, 0.8660254037844387076, 1.000000000000000000, 0.8660254037844387076, 1.000000000000000000, 0.8660254037844387076, 1.000000000000000000, 0.8660254037844387076, 1.000000000000000000, 0.8660254037844387076, 1.000000000000000000, 0.8660254037844387076, 1.000000000000000000, 0.8660254037844387076, 1.000000000000000000, 0.8660254037844387076, 1.000000000000000000, 0.8660254037844387076, 1.000000000000000000, 0.8660254037844387076, 1.000000000000000000, 0.8660254037844387076, 1.000000000000000000, 0.8660254037844387076, 1.000000000000000000, 0.8660254037844387076, 1.000000000000000000, 0.8660254037844387076, 1.000000000000000000, 0.8660254037844387076, 1.000000000000000000, 0.8660254037844387076, 1.000000000000000000, 0.8660254037844387076, 1.000000000000000000, 0.8660254037844387076, 1.000000000000000000, 0.8660254037844387076, 1.000000000000000000, 0.8660254037844387076, 1.000000000000000000, 0.8660254037844387076, 1.000000000000000000, 0.8660254037844387076, 1.000000000000000000, 0.8660254037844387076, 1.000000000000000000, 0.8660254037844387076, 1.000000000000000000, 0.8660254037844387076, 1.000000000000000000, 0.8660254037844387076, 1.000000000000000000, 0.8660254037844387076, 1.000000000000000000, 0.8660254037844387076, 1.000000000000000000, 0.8660254037844387076, 1.000000000000000000, 0.8660254037844387076, 1.000000000000000000, 0.8660254037844387076, 1.000000000000000000, 0.8660254037844387076, 1.000000000000000000, 0.8660254037844387076, 1.000000000000000000, 0.8660254037844387076, 1.000000000000000000, 0.8660254037844387076, 1.000000000000000000, 0.8660254037844387076, 1.000000000000000000, 0.8660254037844387076, 1.000000000000000000, 0.8660254037844387076, 1.000000000000000000, 0.8660254037844387076, 1.000000000000000000, 0.8660254037844387076, 1.000000000000000000, 0.8660254037844387076, 1.000000000000000000, 0.8660254037844387076, 1.000000000000000000, 0.8660254037844387076, 1.000000000000000000, 0.8660254037844387076, 1.000000000000000000, 0.8660254037844387076, 1.000000000000000000, 0.8660254037844387076, 1.000000000000000000, 0.8660254037844387076, 1.000000000000000000, 0.8660254037844387076, 1.000000000000000000, 0.8660254037844387076, 1.000000000000000000, 0.8660254037844387076, 1.000000000000000000, 0.8660254037844387076, 1.000000000000000000, 0.8660254037844387076, 1.000000000000000000, 0.8660254037844387076, 1.000000000000000000, 0.8660254037844387076, 1.000000000000000000, 0.8660254037844387076, 1.000000000000000000, 0.8660254037844387076, 1.000000000000000000, 0.8660254037844387076, 1.000000000000000000, 0.8660254037844387076, 1.000000000000000000, 0.8660254037844387076, 1.000000000000000000, 0.8660254037844387076, 1.000000000000000000, 0.8660254037844387076, 1.000000000000000000, 0.8660254037844387076, 1.000000000000000000, 0.8660254037844387076, 1.000000000000000000, 0.8660254037844387076, 1.000000000000000000, 0.8660254037844387076, 1.000000000000000000, 0.8660254037844387076, 1.000000000000000000, 0.8660254037844387076, 1.000000000000000000, 0.8660254037844387076, 1.000000000000000000, 0.8660254037844387076, 1.000000000000000000, 0.8660254037844387076, 1.000000000000000000, 0.8660254037844387076, 1.000000000000000000, 0.8660254037844387076, 1.000000000000000000, 0.8660254037844387076, 1.000000000000000000, 0.8660254037844387076, 1.000000000000000000, 0.8660254037844387076, 1.000000000000000000, 0.8660254037844387076, 1.000000000000000000, 0.8660254037844387076, 1.000000000000000000, 0.8660254037844387076, 1.000000000000000000, 0.8660254037844387076, 1.000000000000000000, 0.8660254037844387076, 1.000000000000000000, 0.8660254037844387076, 1.000000000000000000, 0.8660254037844387076, 1.000000000000000000, 0.8660254037844387076, 1.000000000000000000, 0.8660254037844387076, 1.000000000000000000, 0.8660254037844387076, 1.000000000000000000, 0.8660254037844387076, 1.000000000000000000, 0.8660254037844387076, 1.000000000000000000, 0.8660254037844387076, 1.000000000000000000, 0.8660254037844387076, 1.000000000000000000, 0.8660254037844387076, 1.000000000000000000, 0.8660254037844387076, 1.000000000000000000, 0.8660254037844387076, 1.000000000000000000, 0.8660254037844387076, 1.000000000000000000, 0.8660254037844387076, 1.000000000000000000, 0.8660254037844387076, 1.000000000000000000, 0.8660254037844387076, 1.000000000000000000, 0.8660254037844387076, 1.000000000000000000, 0.8660254037844387076, 1.000000000000000000, 0.8660254037844387076, 1.000000000000000000, 0.8660254037844387076, 1.000000000000000000, 0.8660254037844387076, 1.000000000000000000, 0.8660254037844387076, 1.000000000000000000, 0.8660254037844387076, 1.000000000000000000, 0.8660254037844387076, 1.000000000000000000, 0.8660254037844387076, 1.000000000000000000, 0.8660254037844387076, 1.000000000000000000, 0.8660254037844387076, 1.000000000000000000, 0.8660254037844387076, 1.000000000000000000, 0.8660254037844387076, 1.000000000000000000, 0.8660254037844387076, 1.000000000000000000, 0.8660254037844387076, 1.000000000000000000, 0.8660254037844387076, 1.000000000000000000, 0.8660254037844387076, 1.000000000000000000, 0.8660254037844387076, 1.000000000000000000, 0.8660254037844387076, 1.000000000000000000, 0.8660254037844387076, 1.000000000000000000, 0.8660254037844387076, 1.000000000000000000, 0.8660254037844387076, 1.000000000000000000, 0.8660254037844387076, 1.000000000000000000, 0.8660254037844387076, 1.000000000000000000, 0.8660254037844387076, 1.000000000000000000, 0.8660254037844387076, 1.000000000000000000, 0.8660254037844387076, 1.000000000000000000, 0.8660254037844387076, 1.000000000000000000, 0.8660254037844387076, 1.000000000000000000, 0.8660254037844387076, 1.000000000000000000, 0.8660254037844387076, 1.000000000000000000, 0.8660254037844387076, 1.000000000000000000, 0.8660254037844387076, 1.000000000000000000, 0.8660254037844387076, 1.000000000000000000, 0.8660254037844387076, 1.000000000000000000, 0.8660254037844387076, 1.000000000000000000, 0.8660254037844387076, 1.000000000000000000, 0.8660254037844387076, 1.000000000000000000, 0.8660254037844387076, 1.000000000000000000, 0.8660254037844387076, 1.000000000000000000, 0.8660254037844387076, 1.000000000000000000, 0.8660254037844387076, 1.000000000000000000, 0.8660254037844387076, 1.000000000000000000, 0.8660254037844387076, 1.000000000000000000, 0.8660254037844387076, 1.000000000000000000, 0.8660254037844387076, 1.000000000000000000, 0.8660254037844387076, 1.000000000000000000, 0.8660254037844387076, 1.000000000000000000, 0.8660254037844387076, 1.000000000000000000, 0.8660254037844387076, 1.000000000000000000, 0.8660254037844387076, 1.000000000000000000, 0.8660254037844387076, 1.000000000000000000, 0.8660254037844387076, 1.000000000000000000, 0.8660254037844387076, 1.000000000000000000, 0.8660254037844387076, 1.000000000000000000, 0.8660254037844387076, 1.000000000000000000, 0.8660254037844387076, 1.000000000000000000) ) ) 
 REPRESENTATION_ITEM ( '' )  SURFACE ( )  );
#8541 = DIRECTION ( 'NONE',  ( -7.147005652999508048E-36, 5.642372883946980038E-36, 1.000000000000000000 ) ) ;
#8542 = VERTEX_POINT ( 'NONE', #4267 ) ;
#8543 = EDGE_LOOP ( 'NONE', ( #1369, #17511, #19146 ) ) ;
#8544 = EDGE_CURVE ( 'NONE', #17032, #28335, #27572, .T. ) ;
#8545 = CARTESIAN_POINT ( 'NONE',  ( 4.763139720814407951, 2.750000000000002665, -97.75000000000000000 ) ) ;
#8546 = CARTESIAN_POINT ( 'NONE',  ( 16.18750000000008527, 1.097466725451559322, -2.649519052838358757 ) ) ;
#8547 = CARTESIAN_POINT ( 'NONE',  ( 6.000000000000000888, -1.607695154586752384, -89.23066243270261566 ) ) ;
#8548 = CARTESIAN_POINT ( 'NONE',  ( 2.775557561562891351E-14, -6.250000000000061284, -113.6830127018922383 ) ) ;
#8549 = VERTEX_POINT ( 'NONE', #20724 ) ;
#8550 = CARTESIAN_POINT ( 'NONE',  ( 3.464101615137757051, -5.999999999999979572, -123.9136751345947971 ) ) ;
#8551 = DIRECTION ( 'NONE',  ( 0.000000000000000000, 0.000000000000000000, -1.000000000000000000 ) ) ;
#8552 = CARTESIAN_POINT ( 'NONE',  ( -5.412658773652684552, -3.125000000000099920, -55.43301270189226670 ) ) ;
#8553 = ORIENTED_EDGE ( 'NONE', *, *, #22038, .T. ) ;
#8554 = EDGE_CURVE ( 'NONE', #27945, #17372, #13846, .T. ) ;
#8555 = FACE_OUTER_BOUND ( 'NONE', #12024, .T. ) ;
#8556 = CARTESIAN_POINT ( 'NONE',  ( 6.000000000000000888, 5.577813053751546416E-15, -177.6636751345948255 ) ) ;
#8557 = CARTESIAN_POINT ( 'NONE',  ( 155.9925748654052313, 2.278174593051927044, 5.500000000000096811 ) ) ;
#8558 = CARTESIAN_POINT ( 'NONE',  ( 0.000000000000000000, 5.499999999999991118, -162.0000000000000284 ) ) ;
#8559 = CARTESIAN_POINT ( 'NONE',  ( 115.7499999999998153, -1.110223024625156540E-13, -2.499999999999946709 ) ) ;
#8560 = CYLINDRICAL_SURFACE ( 'NONE', #6861, 6.000000000000000888 ) ;
#8561 = CARTESIAN_POINT ( 'NONE',  ( -6.350852961085760029, -1.281975124255709124E-13, -107.6250000000000426 ) ) ;
#8562 = CARTESIAN_POINT ( 'NONE',  ( 13.35117513459477401, 2.500000000000084821, 1.035533905932689347 ) ) ;
#8563 = CARTESIAN_POINT ( 'NONE',  ( 4.763139720814407951, 2.750000000000002665, -103.7500000000000142 ) ) ;
#8564 = CARTESIAN_POINT ( 'NONE',  ( 116.0000000000000142, 0.000000000000000000, 0.000000000000000000 ) ) ;
#8565 = CARTESIAN_POINT ( 'NONE',  ( -5.999999999999962697, 3.323446944526963891E-14, -161.9136751345948539 ) ) ;
#8566 = CARTESIAN_POINT ( 'NONE',  ( -5.196152422706601826, 2.999999999999975131, -144.9613248654052597 ) ) ;
#8567 = VERTEX_POINT ( 'NONE', #15849 ) ;
#8568 = STYLED_ITEM ( 'NONE', ( #17698 ), #24254 ) ;
#8569 = CARTESIAN_POINT ( 'NONE',  ( 115.3749999999999574, -1.767766952966320915, 1.767766952966431937 ) ) ;
#8570 = CARTESIAN_POINT ( 'NONE',  ( 23.53867513459495342, 1.665334536937734811E-13, 2.499999999999835687 ) ) ;
#8571 = ORIENTED_EDGE ( 'NONE', *, *, #2958, .F. ) ;
#8572 = CARTESIAN_POINT ( 'NONE',  ( 3.175426480543072749, -5.500000000000105693, -158.1250000000000284 ) ) ;
#8573 = CARTESIAN_POINT ( 'NONE',  ( 6.000000000000000888, 1.743066579297358182E-13, -106.5863248654052313 ) ) ;
#8574 = CARTESIAN_POINT ( 'NONE',  ( 5.412658773652739619, 3.124999999999988898, -88.31698729810783277 ) ) ;
#8575 = CARTESIAN_POINT ( 'NONE',  ( 22.96132486540528106, 1.665334536937734811E-13, 2.499999999999946709 ) ) ;
#8576 = VERTEX_POINT ( 'NONE', #30227 ) ;
#8577 = CARTESIAN_POINT ( 'NONE',  ( 3.464101615137757051, -5.999999999999979572, -75.33632486540520290 ) ) ;
#8578 =( BOUNDED_CURVE ( )  B_SPLINE_CURVE ( 2, ( #9096, #18493, #14354, #25518, #23398, #2188, #16357, #9247, #28269 ),
 .UNSPECIFIED., .F., .T. ) 
 B_SPLINE_CURVE_WITH_KNOTS ( ( 3, 2, 2, 2, 3 ),
 ( 0.7875000000000001998, 0.7937499999999999556, 0.7999999999999998224, 0.8062499999999995781, 0.8124999999999993339 ),
 .UNSPECIFIED. ) 
 CURVE ( )  GEOMETRIC_REPRESENTATION_ITEM ( )  RATIONAL_B_SPLINE_CURVE ( ( 0.9999999999999973355, 0.9238795325112894030, 1.000000000000000000, 0.9238795325112867385, 1.000000000000000000, 0.9238795325112867385, 1.000000000000000000, 0.9238795325112948431, 0.9999999999999918954 ) ) 
 REPRESENTATION_ITEM ( '' )  );
#8579 = VECTOR ( 'NONE', #22361, 1000.000000000000000 ) ;
#8580 = CARTESIAN_POINT ( 'NONE',  ( 0.000000000000000000, 5.499999999999991118, -151.5000000000000284 ) ) ;
#8581 = ORIENTED_EDGE ( 'NONE', *, *, #7251, .F. ) ;
#8582 = ORIENTED_EDGE ( 'NONE', *, *, #6053, .F. ) ;
#8583 = CARTESIAN_POINT ( 'NONE',  ( 158.8125000000000284, 4.242640687119298093, -4.242640687119298093 ) ) ;
#8584 = EDGE_CURVE ( 'NONE', #10268, #17372, #5656, .T. ) ;
#8585 = CARTESIAN_POINT ( 'NONE',  ( -2.775557561562891351E-14, -5.500000000000115463, -122.2500000000000284 ) ) ;
#8586 = EDGE_CURVE ( 'NONE', #14303, #15775, #22681, .T. ) ;
#8587 = ORIENTED_EDGE ( 'NONE', *, *, #15384, .T. ) ;
#8588 = CARTESIAN_POINT ( 'NONE',  ( 0.000000000000000000, -5.999999999999991118, -57.46132486540523132 ) ) ;
#8589 = CARTESIAN_POINT ( 'NONE',  ( -7.216878364870328078, 0.000000000000000000, -123.6919872981078043 ) ) ;
#8590 = CARTESIAN_POINT ( 'NONE',  ( -3.608439182435052128, -6.250000000000110134, -180.4419872981078470 ) ) ;
#8591 = CARTESIAN_POINT ( 'NONE',  ( -4.763139720814407951, 2.749999999999946709, -175.2500000000000284 ) ) ;
#8592 = CARTESIAN_POINT ( 'NONE',  ( 116.0000000000000142, 0.000000000000000000, 0.000000000000000000 ) ) ;
#8593 =( NAMED_UNIT ( * ) PLANE_ANGLE_UNIT ( ) SI_UNIT ( $, .RADIAN. ) );
#8594 = ORIENTED_EDGE ( 'NONE', *, *, #25054, .F. ) ;
#8595 = CARTESIAN_POINT ( 'NONE',  ( 13.62500000000016520, -1.414213562372923505, -1.414213562373145550 ) ) ;
#8596 =( GEOMETRIC_REPRESENTATION_CONTEXT ( 3 ) GLOBAL_UNCERTAINTY_ASSIGNED_CONTEXT ( ( #418 ) ) GLOBAL_UNIT_ASSIGNED_CONTEXT ( ( #11834, #11365, #2272 ) ) REPRESENTATION_CONTEXT ( 'NONE', 'WORKASPACE' ) );
#8597 = CARTESIAN_POINT ( 'NONE',  ( -5.999999999999956479, -1.607695154586745057, -55.34668783648704249 ) ) ;
#8598 = CARTESIAN_POINT ( 'NONE',  ( 6.000000000000000888, -1.607695154586752384, -46.65331216351298593 ) ) ;
#8599 = CARTESIAN_POINT ( 'NONE',  ( 111.9377832217620465, -1.849990392679441875, -0.7662911109075883909 ) ) ;
#8600 = CARTESIAN_POINT ( 'NONE',  ( -3.608439182435052128, -6.250000000000110134, -70.94198729810781856 ) ) ;
#8601 = CARTESIAN_POINT ( 'NONE',  ( 5.412658773652712085, -3.125000000000086153, -55.56698729810782567 ) ) ;
#8602 = CARTESIAN_POINT ( 'NONE',  ( 6.000000000000000888, -1.607695154586752384, -170.2306624327026441 ) ) ;
#8603 = CARTESIAN_POINT ( 'NONE',  ( -3.175426480542816510, -5.500000000000057732, -50.37500000000001421 ) ) ;
#8604 = CARTESIAN_POINT ( 'NONE',  ( 6.000000000000000888, 1.743066579297358182E-13, -48.66367513459482552 ) ) ;
#8605 = CARTESIAN_POINT ( 'NONE',  ( -4.763139720814407951, -2.750000000000016431, -130.0000000000000000 ) ) ;
#8606 = CYLINDRICAL_SURFACE ( 'NONE', #20086, 2.499999999999999112 ) ;
#8607 = CARTESIAN_POINT ( 'NONE',  ( 104.7401757384973990, -1.393188515088598312, -1.223208600277094993 ) ) ;
#8608 = ORIENTED_EDGE ( 'NONE', *, *, #26434, .F. ) ;
#8609 = CARTESIAN_POINT ( 'NONE',  ( 23.43750000000004619, 1.097466725451619718, -2.649519052838238409 ) ) ;
#8610 = AXIS2_PLACEMENT_3D ( 'NONE', #4183, #13296, #20182 ) ;
#8611 = CARTESIAN_POINT ( 'NONE',  ( 159.8363248654052313, 0.000000000000000000, -5.500000000000005329 ) ) ;
#8612 = CARTESIAN_POINT ( 'NONE',  ( 141.1086002691896226, -2.071067811865468400, -4.999999999999989342 ) ) ;
#8613 = ORIENTED_EDGE ( 'NONE', *, *, #9184, .F. ) ;
#8614 = CARTESIAN_POINT ( 'NONE',  ( 113.4372167782374277, 0.7662911109077987781, -1.849990392679291551 ) ) ;
#8615 = CARTESIAN_POINT ( 'NONE',  ( 5.000000000000087930, 5.551115123125782702E-14, -5.551115123125782702E-14 ) ) ;
#8616 = LINE ( 'NONE', #9344, #1355 ) ;
#8617 = CARTESIAN_POINT ( 'NONE',  ( 2.775557561562891351E-14, -6.250000000000061284, -118.8169872981078612 ) ) ;
#8618 = CARTESIAN_POINT ( 'NONE',  ( 140.0000000000000284, -11.48520880827726032, -4.868161254798472726 ) ) ;
#8619 = AXIS2_PLACEMENT_3D ( 'NONE', #1789, #18564, #14135 ) ;
#8620 = CARTESIAN_POINT ( 'NONE',  ( 104.7401757384974275, 1.849990392679526918, 0.1116904995936761485 ) ) ;
#8621 = ORIENTED_EDGE ( 'NONE', *, *, #28913, .T. ) ;
#8622 = DIRECTION ( 'NONE',  ( -1.000000000000000000, -1.665334536937736783E-16, -2.220446049250315546E-16 ) ) ;
#8623 = CARTESIAN_POINT ( 'NONE',  ( 144.8437500000000000, -6.000000000000005329, -2.485281374238555774 ) ) ;
#8624 = ADVANCED_FACE ( 'NONE', ( #1505 ), #10917, .T. ) ;
#8625 = ORIENTED_EDGE ( 'NONE', *, *, #19530, .F. ) ;
#8626 = VERTEX_POINT ( 'NONE', #17983 ) ;
#8627 = CARTESIAN_POINT ( 'NONE',  ( 23.46132486540525264, 1.110223024625156540E-13, -2.500000000000002220 ) ) ;
#8628 = STYLED_ITEM ( 'NONE', ( #2043 ), #19286 ) ;
#8629 = CARTESIAN_POINT ( 'NONE',  ( -2.775557561562891351E-14, -5.500000000000115463, -53.25000000000002132 ) ) ;
#8630 =( BOUNDED_CURVE ( )  B_SPLINE_CURVE ( 2, ( #21602, #28930, #24187, #12857, #17609, #3279, #19884, #14843, #22197 ),
 .UNSPECIFIED., .F., .F. ) 
 B_SPLINE_CURVE_WITH_KNOTS ( ( 3, 2, 2, 2, 3 ),
 ( 0.04166666666666667129, 0.04259259259259259162, 0.04444444444444444614, 0.04629629629629629373, 0.04722222222222221405 ),
 .UNSPECIFIED. ) 
 CURVE ( )  GEOMETRIC_REPRESENTATION_ITEM ( )  RATIONAL_B_SPLINE_CURVE ( ( 0.9330127018922194093, 0.9330127018922196314, 1.000000000000000000, 0.8660254037844388186, 1.000000000000000000, 0.8660254037844388186, 1.000000000000000000, 0.9330127018922199644, 0.9330127018922194093 ) ) 
 REPRESENTATION_ITEM ( '' )  );
#8631 = CARTESIAN_POINT ( 'NONE',  ( 24.37500000000014566, -1.414213562373034527, 1.414213562373034527 ) ) ;
#8632 = CARTESIAN_POINT ( 'NONE',  ( 161.0000000000000284, -11.67610212985248452, -2.769230769230773603 ) ) ;
#8633 = CARTESIAN_POINT ( 'NONE',  ( 0.000000000000000000, -5.999999999999991118, -79.96132486540518869 ) ) ;
#8634 = CARTESIAN_POINT ( 'NONE',  ( 3.608439182435180470, -6.249999999999997335, -65.55801270189225249 ) ) ;
#8635 = CYLINDRICAL_SURFACE ( 'NONE', #16236, 1.000000000000000000 ) ;
#8636 = CARTESIAN_POINT ( 'NONE',  ( 147.4538997308104058, -2.071067811865468400, -4.999999999999989342 ) ) ;
#8637 = CARTESIAN_POINT ( 'NONE',  ( 0.000000000000000000, -5.999999999999991118, -178.0386751345948255 ) ) ;
#8638 = DIRECTION ( 'NONE',  ( 1.067522139062651411E-16, -1.000000000000000000, 0.000000000000000000 ) ) ;
#8639 = FACE_OUTER_BOUND ( 'NONE', #4901, .T. ) ;
#8640 = FILL_AREA_STYLE ('',( #18189 ) ) ;
#8641 = CARTESIAN_POINT ( 'NONE',  ( 4.763139720814407951, -2.749999999999988454, -134.0000000000000000 ) ) ;
#8642 = CARTESIAN_POINT ( 'NONE',  ( -5.412658773652684552, -3.125000000000099920, -148.4330127018922383 ) ) ;
#8643 = CARTESIAN_POINT ( 'NONE',  ( 16.41367513459479710, 1.767766952966376426, 1.767766952966209892 ) ) ;
#8644 = ORIENTED_EDGE ( 'NONE', *, *, #5834, .F. ) ;
#8645 = COLOUR_RGB ( '', 0.40784314, 0.44705882, 0.49803922) ;
#8646 = CARTESIAN_POINT ( 'NONE',  ( 6.350852961086080661, -9.614813431917819062E-14, -60.37500000000000000 ) ) ;
#8647 = CARTESIAN_POINT ( 'NONE',  ( 1.110223024625164183E-16, -2.000000000000012879, -1.776356839400262692E-15 ) ) ;
#8648 = B_SPLINE_CURVE_WITH_KNOTS ( 'NONE', 3,
 ( #9294, #9142, #30177, #16697, #13951, #12091, #26018, #21432, #363, #7293 ),
 .UNSPECIFIED., .F., .F.,
 ( 4, 2, 2, 2, 4 ),
 ( 0.000000000000000000, 0.0005899865232072658413, 0.0008849797848109120435, 0.001032476415612737638, 0.001179973046414563558 ),
 .UNSPECIFIED. ) ;
#8649 = FILL_AREA_STYLE_COLOUR ( '', #2716 ) ;
#8650 = CIRCLE ( 'NONE', #12606, 6.000000000000009770 ) ;
#8651 = STYLED_ITEM ( 'NONE', ( #24165 ), #24848 ) ;
#8652 =( LENGTH_UNIT ( ) NAMED_UNIT ( * ) SI_UNIT ( .MILLI., .METRE. ) );
#8653 = ORIENTED_EDGE ( 'NONE', *, *, #7772, .T. ) ;
#8654 = CARTESIAN_POINT ( 'NONE',  ( 108.4374999999998863, -2.499999999999934719, 1.035533905932929599 ) ) ;
#8655 = CARTESIAN_POINT ( 'NONE',  ( 144.7500000000000568, -6.000000000000005329, 0.000000000000000000 ) ) ;
#8656 = CARTESIAN_POINT ( 'NONE',  ( 142.3199251345948539, -2.278174593052058938, -5.499999999999964473 ) ) ;
#8657 = VECTOR ( 'NONE', #28350, 1000.000000000000000 ) ;
#8658 = EDGE_CURVE ( 'NONE', #567, #8702, #17138, .T. ) ;
#8659 = CARTESIAN_POINT ( 'NONE',  ( 124.9999999999999432, -71.00000000000001421, -4.000000000000003553 ) ) ;
#8660 = CARTESIAN_POINT ( 'NONE',  ( 138.9375000000000568, -4.242640687119298093, -4.242640687119298093 ) ) ;
#8661 = CYLINDRICAL_SURFACE ( 'NONE', #8700, 2.000000000000012879 ) ;
#8662 = VECTOR ( 'NONE', #23249, 1000.000000000000000 ) ;
#8663 = ORIENTED_EDGE ( 'NONE', *, *, #28060, .F. ) ;
#8664 = CARTESIAN_POINT ( 'NONE',  ( -4.763139720814407951, -2.750000000000016431, -146.5000000000000284 ) ) ;
#8665 = ADVANCED_FACE ( 'NONE', ( #14594 ), #28375, .T. ) ;
#8666 = EDGE_LOOP ( 'NONE', ( #14150, #20737, #18158, #24900 ) ) ;
#8667 = CARTESIAN_POINT ( 'NONE',  ( 13.87500000000011013, 1.414213562373312083, -1.414213562373145550 ) ) ;
#8668 = ORIENTED_EDGE ( 'NONE', *, *, #8046, .T. ) ;
#8669 = AXIS2_PLACEMENT_3D ( 'NONE', #7533, #10465, #17389 ) ;
#8670 = CARTESIAN_POINT ( 'NONE',  ( 3.175426480543072749, 5.499999999999865885, -76.62500000000001421 ) ) ;
#8671 = DIRECTION ( 'NONE',  ( -0.7371541402007405486, 1.202626523861922663E-16, -0.6757246285173472700 ) ) ;
#8672 =( BOUNDED_CURVE ( )  B_SPLINE_CURVE ( 2, ( #5116, #7295, #14536, #21433, #8138, #26020, #15089, #19689, #2525 ),
 .UNSPECIFIED., .F., .T. ) 
 B_SPLINE_CURVE_WITH_KNOTS ( ( 3, 2, 2, 2, 3 ),
 ( 0.2058823529411765163, 0.2132352941176470784, 0.2205882352941176405, 0.2279411764705882026, 0.2352941176470587648 ),
 .UNSPECIFIED. ) 
 CURVE ( )  GEOMETRIC_REPRESENTATION_ITEM ( )  RATIONAL_B_SPLINE_CURVE ( ( 1.000000000000000000, 0.9238795325112867385, 1.000000000000000000, 0.9238795325112867385, 1.000000000000000000, 0.9238795325112867385, 1.000000000000000000, 0.9238795325112867385, 1.000000000000000000 ) ) 
 REPRESENTATION_ITEM ( '' )  );
#8673 = CARTESIAN_POINT ( 'NONE',  ( 5.000000000000087041, 5.538625114098749691E-14, 5.999999999999945821 ) ) ;
#8674 = CARTESIAN_POINT ( 'NONE',  ( 6.000000000000000888, 1.743066579297358182E-13, -69.08632486540523132 ) ) ;
#8675 = CARTESIAN_POINT ( 'NONE',  ( -4.999999999999879208, -9.000000000000007105, -4.000000000000003553 ) ) ;
#8676 = CARTESIAN_POINT ( 'NONE',  ( 121.1877832217620750, 0.7662911109077987781, -1.849990392679291551 ) ) ;
#8677 = DIRECTION ( 'NONE',  ( 0.000000000000000000, 0.000000000000000000, 1.000000000000000000 ) ) ;
#8678 =( BOUNDED_CURVE ( )  B_SPLINE_CURVE ( 2, ( #13572, #3841, #22913, #29805, #10956, #22614, #29955, #1853, #17713 ),
 .UNSPECIFIED., .F., .T. ) 
 B_SPLINE_CURVE_WITH_KNOTS ( ( 3, 2, 2, 2, 3 ),
 ( 0.4694444444444444420, 0.4703703703703703276, 0.4722222222222222099, 0.4740740740740740922, 0.4750000000000000888 ),
 .UNSPECIFIED. ) 
 CURVE ( )  GEOMETRIC_REPRESENTATION_ITEM ( )  RATIONAL_B_SPLINE_CURVE ( ( 0.9330127018922194093, 0.9330127018922194093, 1.000000000000000000, 0.8660254037844388186, 1.000000000000000000, 0.8660254037844388186, 1.000000000000000000, 0.9330127018922154125, 0.9330127018922194093 ) ) 
 REPRESENTATION_ITEM ( '' )  );
#8679 = CARTESIAN_POINT ( 'NONE',  ( -6.350852961085760029, -1.281975124255709124E-13, -160.1250000000000284 ) ) ;
#8680 = CARTESIAN_POINT ( 'NONE',  ( 136.6800748654052313, -2.278174593051950136, 5.500000000000074607 ) ) ;
#8681 = CARTESIAN_POINT ( 'NONE',  ( -5.061300234009625143, 3.091548682366505485, -180.0000000000000568 ) ) ;
#8682 = PRODUCT_DEFINITION_SHAPE ( 'NONE', 'NONE',  #20816 ) ;
#8683 = CARTESIAN_POINT ( 'NONE',  ( 4.763139720814407951, -2.749999999999988454, -90.50000000000002842 ) ) ;
#8684 = DIRECTION ( 'NONE',  ( -0.000000000000000000, -0.000000000000000000, -1.000000000000000000 ) ) ;
#8685 = CARTESIAN_POINT ( 'NONE',  ( -9.999999999999980460, -60.00000000000001421, -4.000000000000003553 ) ) ;
#8686 = CARTESIAN_POINT ( 'NONE',  ( -2.775557561562891351E-14, -5.500000000000115463, -77.25000000000004263 ) ) ;
#8687 = DIRECTION ( 'NONE',  ( -7.147005652999508048E-36, 5.642372883946980038E-36, 1.000000000000000000 ) ) ;
#8688 = CARTESIAN_POINT ( 'NONE',  ( 148.5148502691896510, -3.535533905932725318, -3.535533905932725318 ) ) ;
#8689 = CARTESIAN_POINT ( 'NONE',  ( 0.000000000000000000, 5.999999999999977796, -106.2113248654051887 ) ) ;
#8690 = CARTESIAN_POINT ( 'NONE',  ( 124.9999999999999432, -65.50000000000000000, 7.500000000000007105 ) ) ;
#8691 = CIRCLE ( 'NONE', #1813, 12.00000000000000178 ) ;
#8692 = CARTESIAN_POINT ( 'NONE',  ( 140.5000000000000284, -10.99818166789401275, -4.799999999999998934 ) ) ;
#8693 = EDGE_CURVE ( 'NONE', #24844, #9038, #4687, .T. ) ;
#8694 = CARTESIAN_POINT ( 'NONE',  ( 139.3199251345948255, -2.278174593052098018, -5.499999999999928058 ) ) ;
#8695 = CARTESIAN_POINT ( 'NONE',  ( 140.0000000000000284, -54.99999999999990763, -5.000000000000004441 ) ) ;
#8696 = DIRECTION ( 'NONE',  ( 1.000000000000000000, -5.551115123125773458E-17, -1.260129944081490338E-35 ) ) ;
#8697 = EDGE_LOOP ( 'NONE', ( #16530, #7062, #18334, #14442 ) ) ;
#8698 = CARTESIAN_POINT ( 'NONE',  ( 156.1875000000000284, 4.242640687119269671, 4.242640687119298093 ) ) ;
#8699 = CARTESIAN_POINT ( 'NONE',  ( -4.999999999999886313, -10.00000000000000888, 5.000000000000004441 ) ) ;
#8700 = AXIS2_PLACEMENT_3D ( 'NONE', #11134, #20485, #23112 ) ;
#8701 = CARTESIAN_POINT ( 'NONE',  ( 116.3127832217621034, 1.849990392679532247, -0.7662911109075883909 ) ) ;
#8702 = VERTEX_POINT ( 'NONE', #14883 ) ;
#8703 = ADVANCED_FACE ( 'NONE', ( #16760 ), #24224, .T. ) ;
#8704 = ORIENTED_EDGE ( 'NONE', *, *, #28675, .T. ) ;
#8705 = CARTESIAN_POINT ( 'NONE',  ( 3.175426480543072749, 5.499999999999865885, -97.62500000000004263 ) ) ;
#8706 = MECHANICAL_DESIGN_GEOMETRIC_PRESENTATION_REPRESENTATION (  '', ( #16097 ), #26799 ) ;
#8707 = CARTESIAN_POINT ( 'NONE',  ( 16.62500000000011369, 1.110223024625156540E-13, 2.649519052838056332 ) ) ;
#8708 = CYLINDRICAL_SURFACE ( 'NONE', #11140, 2.000000000000012879 ) ;
#8709 = CARTESIAN_POINT ( 'NONE',  ( -5.412658773652684552, -3.125000000000099920, -113.9330127018922667 ) ) ;
#8710 = ORIENTED_EDGE ( 'NONE', *, *, #9438, .T. ) ;
#8711 = CARTESIAN_POINT ( 'NONE',  ( -5.999999999999963585, 8.134310703387671600E-14, -140.3363248654052313 ) ) ;
#8712 = CARTESIAN_POINT ( 'NONE',  ( 140.1564095343160830, -9.003322169323498159, -7.934381245738292954 ) ) ;
#8713 = CARTESIAN_POINT ( 'NONE',  ( 5.999999999999949374, 1.607695154586804565, -52.51933756729741987 ) ) ;
#8714 = CARTESIAN_POINT ( 'NONE',  ( -5.412658773652684552, -3.125000000000099920, -53.93301270189220986 ) ) ;
#8715 = VERTEX_POINT ( 'NONE', #23792 ) ;
#8716 =( NAMED_UNIT ( * ) SI_UNIT ( $, .STERADIAN. ) SOLID_ANGLE_UNIT ( ) );
#8717 = CARTESIAN_POINT ( 'NONE',  ( -0.5000000000000004441, -10.50000000000000888, -7.500000000000007105 ) ) ;
#8718 = STYLED_ITEM ( 'NONE', ( #30172 ), #18784 ) ;
#8719 = CARTESIAN_POINT ( 'NONE',  ( 3.175426480543072749, 5.499999999999865885, -166.6249999999999716 ) ) ;
#8720 = CARTESIAN_POINT ( 'NONE',  ( 117.2499999999998721, 0.000000000000000000, 2.499999999999946709 ) ) ;
#8721 = CARTESIAN_POINT ( 'NONE',  ( 0.000000000000000000, -5.999999999999991118, -157.9613248654052597 ) ) ;
#8722 = CARTESIAN_POINT ( 'NONE',  ( -4.763139720814407951, 2.749999999999946709, -110.7500000000000142 ) ) ;
#8723 = CARTESIAN_POINT ( 'NONE',  ( 13.03867513459488947, 5.551115123125782702E-14, -2.500000000000002220 ) ) ;
#8724 = DIRECTION ( 'NONE',  ( 0.000000000000000000, 0.000000000000000000, 1.000000000000000000 ) ) ;
#8725 = CARTESIAN_POINT ( 'NONE',  ( 4.763139720814407951, -2.749999999999988454, -99.50000000000002842 ) ) ;
#8726 = CARTESIAN_POINT ( 'NONE',  ( 3.464101615137757051, -5.999999999999979572, -111.9136751345948113 ) ) ;
#8727 = DIRECTION ( 'NONE',  ( -7.147005652999508048E-36, 5.642372883946980038E-36, 1.000000000000000000 ) ) ;
#8728 = CARTESIAN_POINT ( 'NONE',  ( 3.464101615137757051, -5.999999999999979572, -81.91367513459479710 ) ) ;
#8729 = ORIENTED_EDGE ( 'NONE', *, *, #11968, .F. ) ;
#8730 = CARTESIAN_POINT ( 'NONE',  ( 16.50000000000018119, 1.873492889145067508, -1.873492889144956486 ) ) ;
#8731 = CARTESIAN_POINT ( 'NONE',  ( 118.2499999999997584, -8.326672684688674053E-14, 2.500000000000057732 ) ) ;
#8732 = EDGE_CURVE ( 'NONE', #6912, #4935, #7756, .T. ) ;
#8733 =( GEOMETRIC_REPRESENTATION_CONTEXT ( 3 ) GLOBAL_UNCERTAINTY_ASSIGNED_CONTEXT ( ( #21743 ) ) GLOBAL_UNIT_ASSIGNED_CONTEXT ( ( #19254, #10026, #14797 ) ) REPRESENTATION_CONTEXT ( 'NONE', 'WORKASPACE' ) );
#8734 = CARTESIAN_POINT ( 'NONE',  ( 110.6877832217622739, -0.7662911109076785410, 1.849990392679712103 ) ) ;
#8735 = CARTESIAN_POINT ( 'NONE',  ( 0.000000000000000000, 4.000000000000017764, -180.0000000000000568 ) ) ;
#8736 = ORIENTED_EDGE ( 'NONE', *, *, #10027, .F. ) ;
#8737 =( LENGTH_UNIT ( ) NAMED_UNIT ( * ) SI_UNIT ( .MILLI., .METRE. ) );
#8738 = CARTESIAN_POINT ( 'NONE',  ( -3.608439182435115633, 6.249999999999965361, -86.44198729810783277 ) ) ;
#8739 = CARTESIAN_POINT ( 'NONE',  ( -6.000000000000007105, -1.607695154586655129, -103.3466878364870212 ) ) ;
#8740 = ORIENTED_EDGE ( 'NONE', *, *, #29699, .T. ) ;
#8741 = EDGE_CURVE ( 'NONE', #15355, #4337, #5775, .T. ) ;
#8742 = CARTESIAN_POINT ( 'NONE',  ( 106.7738248654051603, 2.000000000000061728, 0.8284271247464157772 ) ) ;
#8743 = ADVANCED_FACE ( 'NONE', ( #8235 ), #29203, .F. ) ;
#8744 = VECTOR ( 'NONE', #2665, 1000.000000000000000 ) ;
#8745 = EDGE_LOOP ( 'NONE', ( #25780, #3846, #2274, #20528 ) ) ;
#8746 = CARTESIAN_POINT ( 'NONE',  ( 156.5625000000000284, -4.242640687119298093, 4.242640687119298093 ) ) ;
#8747 = CARTESIAN_POINT ( 'NONE',  ( 0.000000000000000000, 5.499999999999991118, -118.5000000000000568 ) ) ;
#8748 = CARTESIAN_POINT ( 'NONE',  ( -5.412658773652684552, -3.125000000000099920, -140.9330127018922383 ) ) ;
#8749 = ORIENTED_EDGE ( 'NONE', *, *, #24622, .T. ) ;
#8750 = CARTESIAN_POINT ( 'NONE',  ( 150.7574251345948539, -2.278174593051764951, 5.500000000000262013 ) ) ;
#8751 = CARTESIAN_POINT ( 'NONE',  ( 3.608439182435180470, -6.249999999999997335, -123.1919872981078043 ) ) ;
#8752 = CARTESIAN_POINT ( 'NONE',  ( -7.216878364870328078, 0.000000000000000000, -176.1919872981077901 ) ) ;
#8753 = CARTESIAN_POINT ( 'NONE',  ( -6.350852961085760029, -1.281975124255709124E-13, -172.1250000000000284 ) ) ;
#8754 = CARTESIAN_POINT ( 'NONE',  ( 160.7532596262684592, -11.42128382377059737, 3.688773085009012576 ) ) ;
#8755 = CYLINDRICAL_SURFACE ( 'NONE', #15260, 2.000000000000003109 ) ;
#8756 = ORIENTED_EDGE ( 'NONE', *, *, #21609, .F. ) ;
#8757 = CARTESIAN_POINT ( 'NONE',  ( 11.93750000000008527, 2.000000000000091926, -0.8284271247462354770 ) ) ;
#8758 = CARTESIAN_POINT ( 'NONE',  ( 5.196152422706629359, 3.000000000000002665, -148.4613248654052029 ) ) ;
#8759 = CARTESIAN_POINT ( 'NONE',  ( 159.1340520995980228, -12.00000000044276227, -4.000000000000002665 ) ) ;
#8760 = CARTESIAN_POINT ( 'NONE',  ( 0.000000000000000000, 5.999999999999977796, -171.2886751345948255 ) ) ;
#8761 = CARTESIAN_POINT ( 'NONE',  ( 157.6800748654052313, -2.278174593052104679, 5.499999999999918288 ) ) ;
#8762 = CARTESIAN_POINT ( 'NONE',  ( 111.8752832217622881, -1.849990392679579099, 1.110223024625156540E-13 ) ) ;
#8763 = CARTESIAN_POINT ( 'NONE',  ( 5.412658773652712085, -3.125000000000086153, -75.06698729810784698 ) ) ;
#8764 = CARTESIAN_POINT ( 'NONE',  ( -3.608439182435115633, 6.249999999999965361, -59.44198729810781856 ) ) ;
#8765 = CARTESIAN_POINT ( 'NONE',  ( -4.999999999999990230, -24.99999999999999289, -7.500000000000007105 ) ) ;
#8766 = CARTESIAN_POINT ( 'NONE',  ( 6.350852961086080661, -9.614813431917819062E-14, -48.37500000000000711 ) ) ;
#8767 = CARTESIAN_POINT ( 'NONE',  ( -5.999999999999919176, 1.607695154586804565, -102.9033121635129788 ) ) ;
#8768 = DIRECTION ( 'NONE',  ( -5.551115123125774074E-17, -1.000000000000000000, -6.394689268473234689E-36 ) ) ;
#8769 = CARTESIAN_POINT ( 'NONE',  ( -4.763139720814407951, -2.750000000000016431, -121.0000000000000000 ) ) ;
#8770 = CARTESIAN_POINT ( 'NONE',  ( 5.999999999999949374, 1.607695154586804565, -51.01933756729744118 ) ) ;
#8771 = VERTEX_POINT ( 'NONE', #29122 ) ;
#8772 = CARTESIAN_POINT ( 'NONE',  ( 5.196152422706629359, 3.000000000000002665, -158.0386751345948539 ) ) ;
#8773 = EDGE_CURVE ( 'NONE', #15213, #5324, #15057, .T. ) ;
#8774 = CARTESIAN_POINT ( 'NONE',  ( 6.000000000000000888, 1.743066579297358182E-13, -69.66367513459482552 ) ) ;
#8775 = DIRECTION ( 'NONE',  ( -7.147005652999508048E-36, 5.642372883946980038E-36, 1.000000000000000000 ) ) ;
#8776 = CARTESIAN_POINT ( 'NONE',  ( 136.7023502691896510, 0.000000000000000000, -5.000000000000004441 ) ) ;
#8777 = LINE ( 'NONE', #1388, #10069 ) ;
#8778 =( BOUNDED_CURVE ( )  B_SPLINE_CURVE ( 2, ( #5044, #12724, #14475, #22062, #19075, #24344, #14330, #14184, #19750 ),
 .UNSPECIFIED., .F., .F. ) 
 B_SPLINE_CURVE_WITH_KNOTS ( ( 3, 2, 2, 2, 3 ),
 ( 0.8083333333333333481, 0.8092592592592592338, 0.8111111111111111160, 0.8129629629629629983, 0.8138888888888888840 ),
 .UNSPECIFIED. ) 
 CURVE ( )  GEOMETRIC_REPRESENTATION_ITEM ( )  RATIONAL_B_SPLINE_CURVE ( ( 0.9330127018922194093, 0.9330127018922234061, 1.000000000000000000, 0.8660254037844388186, 1.000000000000000000, 0.8660254037844388186, 1.000000000000000000, 0.9330127018922234061, 0.9330127018922194093 ) ) 
 REPRESENTATION_ITEM ( '' )  );
#8779 = EDGE_LOOP ( 'NONE', ( #23647, #11231, #3878, #15090 ) ) ;
#8780 = CARTESIAN_POINT ( 'NONE',  ( 109.2497167782375413, -1.308140751793585022, -1.308140751793640533 ) ) ;
#8781 = DIRECTION ( 'NONE',  ( 1.000000000000000000, -5.551115123125774074E-17, 7.147005652999508048E-36 ) ) ;
#8782 = CARTESIAN_POINT ( 'NONE',  ( 3.608439182435180470, 6.249999999999982236, -116.6919872981078328 ) ) ;
#8783 = CARTESIAN_POINT ( 'NONE',  ( 140.5384615384615756, -11.07692307692309264, -4.615384615384626521 ) ) ;
#8784 = EDGE_CURVE ( 'NONE', #27945, #23810, #4199, .T. ) ;
#8785 = CARTESIAN_POINT ( 'NONE',  ( 113.7113248654051034, 2.000000000000057288, 0.000000000000000000 ) ) ;
#8786 = ORIENTED_EDGE ( 'NONE', *, *, #22255, .T. ) ;
#8787 = VERTEX_POINT ( 'NONE', #8556 ) ;
#8788 = CARTESIAN_POINT ( 'NONE',  ( 105.9136751345946976, -1.414213562373145550, -1.414213562373034527 ) ) ;
#8789 = CARTESIAN_POINT ( 'NONE',  ( 141.3750000000000284, 0.000000000000000000, 6.000000000000005329 ) ) ;
#8790 = ORIENTED_EDGE ( 'NONE', *, *, #4185, .T. ) ;
#8791 = EDGE_LOOP ( 'NONE', ( #18974, #26963, #23991, #7347 ) ) ;
#8792 =( LENGTH_UNIT ( ) NAMED_UNIT ( * ) SI_UNIT ( .MILLI., .METRE. ) );
#8793 = CARTESIAN_POINT ( 'NONE',  ( -3.175426480542816510, -5.500000000000057732, -47.37500000000000000 ) ) ;
#8794 = CARTESIAN_POINT ( 'NONE',  ( 24.31250000000015632, -0.8284271247461152399, 2.000000000000031530 ) ) ;
#8795 = CARTESIAN_POINT ( 'NONE',  ( 117.3511751345945981, 2.000000000000061728, 0.8284271247463557142 ) ) ;
#8796 = FACE_OUTER_BOUND ( 'NONE', #19659, .T. ) ;
#8797 = CARTESIAN_POINT ( 'NONE',  ( 3.608439182435180470, -6.249999999999997335, -64.05801270189225249 ) ) ;
#8798 = CARTESIAN_POINT ( 'NONE',  ( 150.1726497308104058, -5.000000000000004441, 0.000000000000000000 ) ) ;
#8799 = CARTESIAN_POINT ( 'NONE',  ( 160.5863248654052597, 0.000000000000000000, 5.500000000000005329 ) ) ;
#8800 = CARTESIAN_POINT ( 'NONE',  ( 15.96132486540519047, 1.665334536937734811E-13, 2.500000000000057732 ) ) ;
#8801 = CARTESIAN_POINT ( 'NONE',  ( 16.91367513459490723, -1.767766952966209892, -1.767766952966487448 ) ) ;
#8802 = LINE ( 'NONE', #18191, #21160 ) ;
#8803 = AXIS2_PLACEMENT_3D ( 'NONE', #18101, #13051, #23861 ) ;
#8804 = CARTESIAN_POINT ( 'NONE',  ( -3.175426480542816066, 5.499999999999865885, -127.3749999999999858 ) ) ;
#8805 = CARTESIAN_POINT ( 'NONE',  ( 0.000000000000000000, -5.999999999999991118, -92.53867513459479710 ) ) ;
#8806 = CARTESIAN_POINT ( 'NONE',  ( 5.412658773652739619, 3.124999999999988898, -144.6830127018922099 ) ) ;
#8807 = CARTESIAN_POINT ( 'NONE',  ( -5.999999999999963585, -1.487416814333745711E-14, -113.9136751345948255 ) ) ;
#8808 = VERTEX_POINT ( 'NONE', #24832 ) ;
#8809 = EDGE_CURVE ( 'NONE', #12588, #22616, #3438, .T. ) ;
#8810 = CARTESIAN_POINT ( 'NONE',  ( -2.775557561562891351E-14, -5.500000000000115463, -60.75000000000002842 ) ) ;
#8811 = CARTESIAN_POINT ( 'NONE',  ( 6.000000000000000888, -1.859271017917181981E-14, -124.5863248654052171 ) ) ;
#8812 = FACE_OUTER_BOUND ( 'NONE', #17833, .T. ) ;
#8813 = EDGE_CURVE ( 'NONE', #25259, #15491, #21525, .T. ) ;
#8814 = CARTESIAN_POINT ( 'NONE',  ( 0.000000000000000000, 5.999999999999977796, -170.7113248654052029 ) ) ;
#8815 = ORIENTED_EDGE ( 'NONE', *, *, #11716, .T. ) ;
#8816 = CARTESIAN_POINT ( 'NONE',  ( 120.4372167782375271, 0.7662911109078588412, -1.849990392679291551 ) ) ;
#8817 = CARTESIAN_POINT ( 'NONE',  ( 147.7500000000000284, -6.000000000000005329, 0.000000000000000000 ) ) ;
#8818 = CARTESIAN_POINT ( 'NONE',  ( 160.9999999872065644, -11.61885033700936987, -3.010625523247188351 ) ) ;
#8819 = CARTESIAN_POINT ( 'NONE',  ( 12.87500000000008171, 1.414213562373312083, -1.414213562373034527 ) ) ;
#8820 = DIRECTION ( 'NONE',  ( -7.147005652999508048E-36, 5.642372883946980038E-36, 1.000000000000000000 ) ) ;
#8821 = CARTESIAN_POINT ( 'NONE',  ( 139.0312500000000853, -2.485281374238555774, -6.000000000000005329 ) ) ;
#8822 = CARTESIAN_POINT ( 'NONE',  ( 21.60117513459502092, -1.035533905932629173, 2.499999999999904521 ) ) ;
#8823 = ORIENTED_EDGE ( 'NONE', *, *, #8809, .F. ) ;
#8824 =( BOUNDED_CURVE ( )  B_SPLINE_CURVE ( 2, ( #23389, #14201, #2337, #13, #9398, #7085, #2477, #23538, #24560 ),
 .UNSPECIFIED., .F., .F. ) 
 B_SPLINE_CURVE_WITH_KNOTS ( ( 3, 2, 2, 2, 3 ),
 ( 0.9250000000000000444, 0.9259259259259259300, 0.9277777777777778123, 0.9296296296296295836, 0.9305555555555555802 ),
 .UNSPECIFIED. ) 
 CURVE ( )  GEOMETRIC_REPRESENTATION_ITEM ( )  RATIONAL_B_SPLINE_CURVE ( ( 0.9330127018922194093, 0.9330127018922234061, 1.000000000000000000, 0.8660254037844388186, 1.000000000000000000, 0.8660254037844388186, 1.000000000000000000, 0.9330127018922154125, 0.9330127018922194093 ) ) 
 REPRESENTATION_ITEM ( '' )  );
#8825 = AXIS2_PLACEMENT_3D ( 'NONE', #4474, #2182, #25510 ) ;
#8826 = CARTESIAN_POINT ( 'NONE',  ( 4.763139720814407951, -2.749999999999988454, -138.5000000000000000 ) ) ;
#8827 = CARTESIAN_POINT ( 'NONE',  ( 11.68750000000000000, -0.8284271247461753029, -1.999999999999971800 ) ) ;
#8828 = ORIENTED_EDGE ( 'NONE', *, *, #17310, .F. ) ;
#8829 = CARTESIAN_POINT ( 'NONE',  ( 3.175426480543072749, -5.500000000000105693, -74.12500000000007105 ) ) ;
#8830 = CARTESIAN_POINT ( 'NONE',  ( 18.22617513459500671, 2.500000000000144773, -1.035533905932869425 ) ) ;
#8831 = CARTESIAN_POINT ( 'NONE',  ( -0.1999138633143323907, -11.00000000000000711, -19.00000000000000711 ) ) ;
#8832 = CARTESIAN_POINT ( 'NONE',  ( -5.999999999999957367, 1.607695154586737507, -149.9806624327026157 ) ) ;
#8833 = CARTESIAN_POINT ( 'NONE',  ( 113.1011751345946266, 0.8284271247462654530, -1.999999999999791278 ) ) ;
#8834 = CARTESIAN_POINT ( 'NONE',  ( -5.999999999999963585, 8.134310703387671600E-14, -121.4136751345948255 ) ) ;
#8835 = CARTESIAN_POINT ( 'NONE',  ( 0.000000000000000000, 0.000000000000000000, 0.000000000000000000 ) ) ;
#8836 =( NAMED_UNIT ( * ) PLANE_ANGLE_UNIT ( ) SI_UNIT ( $, .RADIAN. ) );
#8837 = CARTESIAN_POINT ( 'NONE',  ( 3.175426480543072749, -5.500000000000105693, -159.6250000000000284 ) ) ;
#8838 = DIRECTION ( 'NONE',  ( -1.000000000000000000, -1.665334536937731113E-16, 1.526556658859586792E-16 ) ) ;
#8839 = CARTESIAN_POINT ( 'NONE',  ( 19.71132486540533435, 2.500000000000224265, -1.110223024625156540E-13 ) ) ;
#8840 = VECTOR ( 'NONE', #23000, 1000.000000000000000 ) ;
#8841 = CARTESIAN_POINT ( 'NONE',  ( 6.350852961086080661, -9.614813431917819062E-14, -84.37500000000004263 ) ) ;
#8842 =( NAMED_UNIT ( * ) PLANE_ANGLE_UNIT ( ) SI_UNIT ( $, .RADIAN. ) );
#8843 = CARTESIAN_POINT ( 'NONE',  ( 0.000000000000000000, 5.499999999999991118, -70.50000000000000000 ) ) ;
#8844 = EDGE_CURVE ( 'NONE', #6568, #25854, #25815, .T. ) ;
#8845 = AXIS2_PLACEMENT_3D ( 'NONE', #15705, #20282, #29630 ) ;
#8846 = CARTESIAN_POINT ( 'NONE',  ( 5.999999999999897859, 1.607695154586893826, -142.5193375672974128 ) ) ;
#8847 = CARTESIAN_POINT ( 'NONE',  ( 3.464101615137757051, -5.999999999999979572, -174.9136751345948539 ) ) ;
#8848 = CYLINDRICAL_SURFACE ( 'NONE', #25717, 1.000000000000000888 ) ;
#8849 = CARTESIAN_POINT ( 'NONE',  ( 6.000000000000014211, -1.607695154586730180, -149.2306624327026441 ) ) ;
#8850 = CARTESIAN_POINT ( 'NONE',  ( 18.50000000000012790, -1.999999999999835243, 0.000000000000000000 ) ) ;
#8851 = CARTESIAN_POINT ( 'NONE',  ( 0.000000000000000000, 5.999999999999977796, -118.7886751345948397 ) ) ;
#8852 = CYLINDRICAL_SURFACE ( 'NONE', #15122, 2.499999999999999112 ) ;
#8853 = CARTESIAN_POINT ( 'NONE',  ( -5.196152422706601826, 2.999999999999975131, -169.5386751345948539 ) ) ;
#8854 = ORIENTED_EDGE ( 'NONE', *, *, #1861, .T. ) ;
#8855 = CARTESIAN_POINT ( 'NONE',  ( 159.0937500000000284, 6.000000000000005329, 2.485281374238585972 ) ) ;
#8856 = DIRECTION ( 'NONE',  ( -7.147005652999508048E-36, 5.642372883946980038E-36, 1.000000000000000000 ) ) ;
#8857 = CARTESIAN_POINT ( 'NONE',  ( 118.1877832217622029, 0.7662911109078588412, -1.849990392679351725 ) ) ;
#8858 = CARTESIAN_POINT ( 'NONE',  ( 5.196152422706629359, 3.000000000000002665, -157.4613248654052029 ) ) ;
#8859 = EDGE_LOOP ( 'NONE', ( #15695, #6854, #28172, #461, #11182 ) ) ;
#8860 = ORIENTED_EDGE ( 'NONE', *, *, #11015, .F. ) ;
#8861 =( BOUNDED_CURVE ( )  B_SPLINE_CURVE ( 2, ( #25483, #23516, #4599, #6907, #20594, #7214, #18460, #25648, #14179 ),
 .UNSPECIFIED., .F., .T. ) 
 B_SPLINE_CURVE_WITH_KNOTS ( ( 3, 2, 2, 2, 3 ),
 ( 0.5588235294117647189, 0.5661764705882352811, 0.5735294117647058432, 0.5808823529411764053, 0.5882352941176470784 ),
 .UNSPECIFIED. ) 
 CURVE ( )  GEOMETRIC_REPRESENTATION_ITEM ( )  RATIONAL_B_SPLINE_CURVE ( ( 1.000000000000000000, 0.9238795325112867385, 1.000000000000000000, 0.9238795325112867385, 1.000000000000000000, 0.9238795325112867385, 1.000000000000000000, 0.9238795325112867385, 1.000000000000000000 ) ) 
 REPRESENTATION_ITEM ( '' )  );
#8862 = VERTEX_POINT ( 'NONE', #10422 ) ;
#8863 = CARTESIAN_POINT ( 'NONE',  ( -3.175426480542816510, 5.499999999999865885, -97.37499999999998579 ) ) ;
#8864 =( GEOMETRIC_REPRESENTATION_CONTEXT ( 3 ) GLOBAL_UNCERTAINTY_ASSIGNED_CONTEXT ( ( #7211 ) ) GLOBAL_UNIT_ASSIGNED_CONTEXT ( ( #22543, #6703, #15966 ) ) REPRESENTATION_CONTEXT ( 'NONE', 'WORKASPACE' ) );
#8865 = FACE_OUTER_BOUND ( 'NONE', #26, .T. ) ;
#8866 = CARTESIAN_POINT ( 'NONE',  ( -7.216878364870328078, 0.000000000000000000, -111.0580127018922241 ) ) ;
#8867 = CARTESIAN_POINT ( 'NONE',  ( 0.8029667472979687970, 10.97248951867538125, -19.05056182979571133 ) ) ;
#8868 = DIRECTION ( 'NONE',  ( 0.000000000000000000, 0.8570991287109669399, 0.5151515151515151381 ) ) ;
#8869 = EDGE_CURVE ( 'NONE', #24823, #14484, #15358, .T. ) ;
#8870 = CARTESIAN_POINT ( 'NONE',  ( 159.0863248654052597, 0.000000000000000000, 5.500000000000005329 ) ) ;
#8871 = ORIENTED_EDGE ( 'NONE', *, *, #25362, .F. ) ;
#8872 = CARTESIAN_POINT ( 'NONE',  ( -3.464101615137725076, 5.999999999999979572, -153.1636751345947971 ) ) ;
#8873 = DIRECTION ( 'NONE',  ( -1.000000000000000000, -1.665334536937736783E-16, -2.220446049250315546E-16 ) ) ;
#8874 = CARTESIAN_POINT ( 'NONE',  ( 147.3675748654052029, -5.500000000000012434, 2.278174593052012309 ) ) ;
#8875 = CARTESIAN_POINT ( 'NONE',  ( -6.350852961085760029, -1.281975124255709124E-13, -163.1249999999999716 ) ) ;
#8876 = CARTESIAN_POINT ( 'NONE',  ( 117.4999999999999574, -2.499999999999891198, 0.000000000000000000 ) ) ;
#8877 = CARTESIAN_POINT ( 'NONE',  ( 6.350852961086080661, -9.614813431917819062E-14, -105.3750000000000426 ) ) ;
#8878 = LINE ( 'NONE', #3478, #19310 ) ;
#8879 = CARTESIAN_POINT ( 'NONE',  ( -5.196152422706573404, -3.000000000000002665, -122.7886751345948539 ) ) ;
#8880 = CARTESIAN_POINT ( 'NONE',  ( 3.175426480543072749, -5.500000000000105693, -99.62500000000007105 ) ) ;
#8881 = ADVANCED_FACE ( 'NONE', ( #19774 ), #22239, .T. ) ;
#8882 = CARTESIAN_POINT ( 'NONE',  ( 159.9523502691896510, 0.000000000000000000, 5.000000000000004441 ) ) ;
#8883 = CARTESIAN_POINT ( 'NONE',  ( -0.06476833834507110532, -14.68192379133359715, 8.233483135134466835 ) ) ;
#8884 = ORIENTED_EDGE ( 'NONE', *, *, #14613, .F. ) ;
#8885 = CARTESIAN_POINT ( 'NONE',  ( 11.68750000000009059, 2.649519052838478661, 1.097466725451439196 ) ) ;
#8886 = CARTESIAN_POINT ( 'NONE',  ( 115.7499999999998153, -1.110223024625156540E-13, -2.499999999999946709 ) ) ;
#8887 = CARTESIAN_POINT ( 'NONE',  ( 112.0627832217620750, -0.7662911109077388261, -1.849990392679231599 ) ) ;
#8888 = CARTESIAN_POINT ( 'NONE',  ( 161.0439367657379819, 2.138417669162241186, 5.124551926995916773 ) ) ;
#8889 = ORIENTED_EDGE ( 'NONE', *, *, #18932, .T. ) ;
#8890 = CARTESIAN_POINT ( 'NONE',  ( -3.464101615137725076, 5.999999999999979572, -112.0863248654051887 ) ) ;
#8891 = CARTESIAN_POINT ( 'NONE',  ( 5.412658773652739619, 3.124999999999988898, -86.81698729810783277 ) ) ;
#8892 = ORIENTED_EDGE ( 'NONE', *, *, #29666, .F. ) ;
#8893 = CARTESIAN_POINT ( 'NONE',  ( 0.000000000000000000, -5.999999999999991118, -65.53867513459482552 ) ) ;
#8894 = ORIENTED_EDGE ( 'NONE', *, *, #21263, .F. ) ;
#8895 = ORIENTED_EDGE ( 'NONE', *, *, #17918, .T. ) ;
#8896 = CARTESIAN_POINT ( 'NONE',  ( 158.1562500000000284, -6.000000000000005329, 2.485281374238555774 ) ) ;
#8897 = ORIENTED_EDGE ( 'NONE', *, *, #22385, .F. ) ;
#8898 = CARTESIAN_POINT ( 'NONE',  ( -4.763139720814407951, -2.750000000000016431, -121.0000000000000000 ) ) ;
#8899 = CARTESIAN_POINT ( 'NONE',  ( 21.37500000000011724, 2.649519052838500421, -5.551115123125782702E-14 ) ) ;
#8900 = CARTESIAN_POINT ( 'NONE',  ( -5.412658773652739619, 3.124999999999975131, -132.1830127018922667 ) ) ;
#8901 = ORIENTED_EDGE ( 'NONE', *, *, #2366, .T. ) ;
#8902 = LINE ( 'NONE', #25156, #25352 ) ;
#8903 = CARTESIAN_POINT ( 'NONE',  ( 3.608439182435180470, 6.249999999999982236, -124.1919872981078043 ) ) ;
#8904 = CARTESIAN_POINT ( 'NONE',  ( -3.608439182435052128, -6.250000000000110134, -175.9419872981078754 ) ) ;
#8905 = DIRECTION ( 'NONE',  ( 1.000000000000000000, -0.000000000000000000, -0.000000000000000000 ) ) ;
#8906 = APPLICATION_CONTEXT ( 'automotive_design' ) ;
#8907 = DIRECTION ( 'NONE',  ( 0.000000000000000000, 0.000000000000000000, -1.000000000000000000 ) ) ;
#8908 = EDGE_CURVE ( 'NONE', #12739, #27786, #13058, .T. ) ;
#8909 = EDGE_LOOP ( 'NONE', ( #12577, #26661, #1558, #238 ) ) ;
#8910 = CARTESIAN_POINT ( 'NONE',  ( 125.0000000000000568, -55.00000000000000711, 8.000000000000007105 ) ) ;
#8911 = CARTESIAN_POINT ( 'NONE',  ( 159.6672377553881574, -12.19842965096654552, -3.747663857213427541 ) ) ;
#8912 = DIRECTION ( 'NONE',  ( 0.000000000000000000, 0.000000000000000000, 1.000000000000000000 ) ) ;
#8913 = AXIS2_PLACEMENT_3D ( 'NONE', #24157, #12371, #10043 ) ;
#8914 = CARTESIAN_POINT ( 'NONE',  ( 111.8127832217621460, -1.849990392679441875, 0.7662911109079489913 ) ) ;
#8915 = CARTESIAN_POINT ( 'NONE',  ( -3.608439182435115633, 6.249999999999965361, -74.44198729810783277 ) ) ;
#8916 = CARTESIAN_POINT ( 'NONE',  ( 5.412658773652712085, -3.125000000000086153, -63.06698729810783277 ) ) ;
#8917 = DIRECTION ( 'NONE',  ( 1.000000000000000000, 6.938893903907222067E-15, 0.000000000000000000 ) ) ;
#8918 = CARTESIAN_POINT ( 'NONE',  ( 3.175426480543072749, -5.500000000000105693, -47.12500000000006395 ) ) ;
#8919 = DIRECTION ( 'NONE',  ( -1.000000000000000000, 0.000000000000000000, -0.000000000000000000 ) ) ;
#8920 = CARTESIAN_POINT ( 'NONE',  ( 3.464101615137757051, -5.999999999999979572, -123.3363248654051745 ) ) ;
#8921 = EDGE_CURVE ( 'NONE', #27307, #7379, #17809, .T. ) ;
#8922 = CARTESIAN_POINT ( 'NONE',  ( -6.350852961085760029, -1.281975124255709124E-13, -122.6250000000000426 ) ) ;
#8923 = CARTESIAN_POINT ( 'NONE',  ( -5.999999999999963585, 8.134310703387671600E-14, -145.4136751345948539 ) ) ;
#8924 = ORIENTED_EDGE ( 'NONE', *, *, #23918, .F. ) ;
#8925 = CARTESIAN_POINT ( 'NONE',  ( 20.50000000000004619, 1.873492889144956486, -1.873492889144900975 ) ) ;
#8926 = CARTESIAN_POINT ( 'NONE',  ( 24.50000000000010658, 5.551115123125782702E-14, -5.551115123125782702E-14 ) ) ;
#8927 = DIRECTION ( 'NONE',  ( 0.000000000000000000, 0.000000000000000000, -1.000000000000000000 ) ) ;
#8928 = CARTESIAN_POINT ( 'NONE',  ( 137.5461002691896510, -2.071067811865468400, 4.999999999999989342 ) ) ;
#8929 = CARTESIAN_POINT ( 'NONE',  ( 5.196152422706629359, -2.999999999999988898, -147.7886751345948255 ) ) ;
#8930 = ORIENTED_EDGE ( 'NONE', *, *, #26063, .F. ) ;
#8931 = CARTESIAN_POINT ( 'NONE',  ( 108.9372167782374987, -0.7662911109077087390, 1.849990392679591977 ) ) ;
#8932 = CARTESIAN_POINT ( 'NONE',  ( -5.999999999999944933, 1.607695154586759934, -121.4806624327025872 ) ) ;
#8933 = CARTESIAN_POINT ( 'NONE',  ( 112.8747167782376124, 2.775557561562891351E-14, 1.849990392679634610 ) ) ;
#8934 = CARTESIAN_POINT ( 'NONE',  ( -7.216878364870328078, 0.000000000000000000, -113.1919872981078186 ) ) ;
#8935 = AXIS2_PLACEMENT_3D ( 'NONE', #24225, #9669, #5027 ) ;
#8936 = CARTESIAN_POINT ( 'NONE',  ( 22.39882486540529172, -1.035533905932568999, -2.499999999999904521 ) ) ;
#8937 = CARTESIAN_POINT ( 'NONE',  ( 110.2113248654050608, -1.999999999999946265, 0.000000000000000000 ) ) ;
#8938 = ORIENTED_EDGE ( 'NONE', *, *, #683, .F. ) ;
#8939 = VERTEX_POINT ( 'NONE', #27732 ) ;
#8940 = CARTESIAN_POINT ( 'NONE',  ( 6.000000000000000888, -3.330669073875464691E-16, -7.560779664488942560E-35 ) ) ;
#8941 = CARTESIAN_POINT ( 'NONE',  ( 141.0000000000000284, 6.000000000000005329, 0.000000000000000000 ) ) ;
#8942 = CARTESIAN_POINT ( 'NONE',  ( 2.775557561562891351E-14, 6.250000000000033751, -143.5669872981077901 ) ) ;
#8943 = AXIS2_PLACEMENT_3D ( 'NONE', #13706, #11395, #4438 ) ;
#8944 = CARTESIAN_POINT ( 'NONE',  ( 2.775557561562891351E-14, -11.00000000000001066, -31.00000000000002842 ) ) ;
#8945 = EDGE_CURVE ( 'NONE', #11342, #25384, #9760, .T. ) ;
#8946 = CARTESIAN_POINT ( 'NONE',  ( 22.37500000000011724, -1.414213562372979016, 1.414213562372979016 ) ) ;
#8947 = CARTESIAN_POINT ( 'NONE',  ( -5.999999999999963585, 8.134310703387671600E-14, -119.9136751345948397 ) ) ;
#8948 = CARTESIAN_POINT ( 'NONE',  ( -3.608439182435115633, 6.249999999999965361, -70.80801270189222407 ) ) ;
#8949 = CARTESIAN_POINT ( 'NONE',  ( 135.0029060396527996, -6.966976446506110143, -8.000000000000007105 ) ) ;
#8950 = CARTESIAN_POINT ( 'NONE',  ( 141.9226497308104342, 5.000000000000004441, 0.000000000000000000 ) ) ;
#8951 = CARTESIAN_POINT ( 'NONE',  ( 6.055081547227420202, 0.000000000000000000, 0.000000000000000000 ) ) ;
#8952 = CARTESIAN_POINT ( 'NONE',  ( -5.196152422706601826, 2.999999999999975131, -73.53867513459483973 ) ) ;
#8953 = CARTESIAN_POINT ( 'NONE',  ( 116.0000000000000142, 6.735557395310442023E-16, 5.500000000000000000 ) ) ;
#8954 = CARTESIAN_POINT ( 'NONE',  ( 16.78867513459492145, -2.499999999999891198, -2.775557561562891351E-13 ) ) ;
#8955 = CARTESIAN_POINT ( 'NONE',  ( 111.4374999999997300, -2.499999999999904521, 1.035533905932869425 ) ) ;
#8956 = EDGE_CURVE ( 'NONE', #13611, #20342, #25753, .T. ) ;
#8957 =( BOUNDED_CURVE ( )  B_SPLINE_CURVE ( 2, ( #9629, #21758, #5290, #7460, #19022, #7317, #3138, #14699, #16871 ),
 .UNSPECIFIED., .F., .F. ) 
 B_SPLINE_CURVE_WITH_KNOTS ( ( 3, 2, 2, 2, 3 ),
 ( 0.9375000000000004441, 0.9437500000000003109, 0.9500000000000000666, 0.9562500000000000444, 0.9570852465708525880 ),
 .UNSPECIFIED. ) 
 CURVE ( )  GEOMETRIC_REPRESENTATION_ITEM ( )  RATIONAL_B_SPLINE_CURVE ( ( 0.9999999999999945599, 0.9238795325112921786, 1.000000000000000000, 0.9238795325112867385, 1.000000000000000000, 0.9238795325112867385, 1.000000000000000000, 0.9898273024893375904, 0.9823735524065475566 ) ) 
 REPRESENTATION_ITEM ( '' )  );
#8958 = CARTESIAN_POINT ( 'NONE',  ( 6.350852961086080661, -9.614813431917819062E-14, -127.8749999999999858 ) ) ;
#8959 = CARTESIAN_POINT ( 'NONE',  ( 2.775557561562891351E-14, -6.250000000000061284, -145.1830127018922667 ) ) ;
#8960 = FACE_OUTER_BOUND ( 'NONE', #12610, .T. ) ;
#8961 = VERTEX_POINT ( 'NONE', #9484 ) ;
#8962 = CIRCLE ( 'NONE', #27556, 11.00000000000001599 ) ;
#8963 = CARTESIAN_POINT ( 'NONE',  ( 6.350852961086080661, -9.614813431917819062E-14, -52.87500000000002842 ) ) ;
#8964 = DIRECTION ( 'NONE',  ( 0.000000000000000000, 0.000000000000000000, 1.000000000000000000 ) ) ;
#8965 = CARTESIAN_POINT ( 'NONE',  ( 0.000000000000000000, 0.000000000000000000, 0.000000000000000000 ) ) ;
#8966 = LINE ( 'NONE', #30147, #28781 ) ;
#8967 = ORIENTED_EDGE ( 'NONE', *, *, #716, .T. ) ;
#8968 = CARTESIAN_POINT ( 'NONE',  ( 104.7499999999998295, 5.551115123125782702E-14, -2.499999999999835687 ) ) ;
#8969 = CARTESIAN_POINT ( 'NONE',  ( 138.0000000000000284, 6.000000000000005329, 0.000000000000000000 ) ) ;
#8970 = CARTESIAN_POINT ( 'NONE',  ( 138.8437500000000568, -6.000000000000005329, -2.485281374238555774 ) ) ;
#8971 = LINE ( 'NONE', #11613, #21963 ) ;
#8972 = EDGE_LOOP ( 'NONE', ( #8258, #2091, #26561, #28027 ) ) ;
#8973 = CARTESIAN_POINT ( 'NONE',  ( 6.350852961086080661, -9.614813431917819062E-14, -135.3750000000000284 ) ) ;
#8974 = CARTESIAN_POINT ( 'NONE',  ( 14.87500000000011013, 1.414213562373201061, -1.414213562373090038 ) ) ;
#8975 = VERTEX_POINT ( 'NONE', #4848 ) ;
#8976 = CARTESIAN_POINT ( 'NONE',  ( 4.763139720814407951, 2.750000000000002665, -69.25000000000002842 ) ) ;
#8977 = ADVANCED_FACE ( 'NONE', ( #6711 ), #4701, .T. ) ;
#8978 = CARTESIAN_POINT ( 'NONE',  ( 18.10117513459491789, 1.035533905932809473, -2.499999999999964473 ) ) ;
#8979 = EDGE_CURVE ( 'NONE', #10444, #23217, #20893, .T. ) ;
#8980 = ORIENTED_EDGE ( 'NONE', *, *, #9084, .T. ) ;
#8981 = DIRECTION ( 'NONE',  ( 1.665334536937731113E-16, -1.000000000000000000, -2.081668171172166973E-17 ) ) ;
#8982 = CARTESIAN_POINT ( 'NONE',  ( -5.196152422706573404, -3.000000000000002665, -83.78867513459481131 ) ) ;
#8983 = CARTESIAN_POINT ( 'NONE',  ( 113.0386751345947687, 0.000000000000000000, -1.999999999999890754 ) ) ;
#8984 = CARTESIAN_POINT ( 'NONE',  ( 118.5002832217622171, 1.308140751793723799, 1.308140751793862577 ) ) ;
#8985 = CARTESIAN_POINT ( 'NONE',  ( 4.763139720814407951, -2.749999999999988454, -150.5000000000000284 ) ) ;
#8986 = DIRECTION ( 'NONE',  ( -7.147005652999508048E-36, 5.642372883946980038E-36, 1.000000000000000000 ) ) ;
#8987 = CARTESIAN_POINT ( 'NONE',  ( -4.763139720814407951, -2.750000000000016431, -142.0000000000000284 ) ) ;
#8988 = CARTESIAN_POINT ( 'NONE',  ( 2.775557561562891351E-14, 6.250000000000033751, -157.9330127018922383 ) ) ;
#8989 = CARTESIAN_POINT ( 'NONE',  ( -0.8012806810451077455, -9.198719318954825752, 4.013103574300091125 ) ) ;
#8990 = CARTESIAN_POINT ( 'NONE',  ( 156.7425748654052029, -2.278174593052183283, -5.499999999999842792 ) ) ;
#8991 = CARTESIAN_POINT ( 'NONE',  ( 3.175426480543072749, 5.499999999999865885, -76.62500000000001421 ) ) ;
#8992 = FACE_OUTER_BOUND ( 'NONE', #21595, .T. ) ;
#8993 = CARTESIAN_POINT ( 'NONE',  ( 3.175426480543072749, 5.499999999999865885, -70.62500000000004263 ) ) ;
#8994 = VECTOR ( 'NONE', #3071, 1000.000000000000000 ) ;
#8995 = CARTESIAN_POINT ( 'NONE',  ( -5.196152422706573404, -3.000000000000002665, -74.78867513459486815 ) ) ;
#8996 = CARTESIAN_POINT ( 'NONE',  ( -4.999999999999886313, -10.00000000000000888, 8.000000000000007105 ) ) ;
#8997 = DIRECTION ( 'NONE',  ( 1.000000000000000000, 0.000000000000000000, 0.000000000000000000 ) ) ;
#8998 = CARTESIAN_POINT ( 'NONE',  ( 3.464101615137757051, -5.999999999999979572, -75.91367513459483973 ) ) ;
#8999 = CARTESIAN_POINT ( 'NONE',  ( 21.06250000000004619, 2.000000000000151879, 0.8284271247461152399 ) ) ;
#9000 = CARTESIAN_POINT ( 'NONE',  ( 141.0000000000000284, -12.00000000000001066, -4.000000000000003553 ) ) ;
#9001 =( BOUNDED_CURVE ( )  B_SPLINE_CURVE ( 2, ( #10049, #19428, #28905, #28755, #3251, #7724, #22017, #22173, #17429 ),
 .UNSPECIFIED., .F., .F. ) 
 B_SPLINE_CURVE_WITH_KNOTS ( ( 3, 2, 2, 2, 3 ),
 ( 0.1527777777777777901, 0.1537037037037036757, 0.1555555555555555580, 0.1574074074074074403, 0.1583333333333333259 ),
 .UNSPECIFIED. ) 
 CURVE ( )  GEOMETRIC_REPRESENTATION_ITEM ( )  RATIONAL_B_SPLINE_CURVE ( ( 0.9330127018922194093, 0.9330127018922194093, 1.000000000000000000, 0.8660254037844388186, 1.000000000000000000, 0.8660254037844388186, 1.000000000000000000, 0.9330127018922194093, 0.9330127018922194093 ) ) 
 REPRESENTATION_ITEM ( '' )  );
#9002 = CARTESIAN_POINT ( 'NONE',  ( 116.1872167782374987, -1.849990392679532247, -0.7662911109077087390 ) ) ;
#9003 = CARTESIAN_POINT ( 'NONE',  ( 101.5358983848621932, 1.203706215242021998E-32, 1.069105884036878258E-47 ) ) ;
#9004 = ORIENTED_EDGE ( 'NONE', *, *, #27026, .F. ) ;
#9005 = CARTESIAN_POINT ( 'NONE',  ( 157.8750000000000568, 0.000000000000000000, 6.000000000000005329 ) ) ;
#9006 = CARTESIAN_POINT ( 'NONE',  ( 14.89882486540530593, 1.035533905932869425, 2.499999999999904521 ) ) ;
#9007 = CARTESIAN_POINT ( 'NONE',  ( 116.0002832217622171, -1.308140751793585022, -1.308140751793640533 ) ) ;
#9008 = ORIENTED_EDGE ( 'NONE', *, *, #6509, .F. ) ;
#9009 = ORIENTED_EDGE ( 'NONE', *, *, #8693, .T. ) ;
#9010 = ORIENTED_EDGE ( 'NONE', *, *, #16133, .T. ) ;
#9011 = CARTESIAN_POINT ( 'NONE',  ( -4.763139720814407951, -2.750000000000016431, -95.50000000000002842 ) ) ;
#9012 = EDGE_CURVE ( 'NONE', #22842, #1806, #18209, .T. ) ;
#9013 = CARTESIAN_POINT ( 'NONE',  ( 2.775557561562891351E-14, 6.250000000000033751, -105.4330127018922525 ) ) ;
#9014 = ORIENTED_EDGE ( 'NONE', *, *, #2191, .F. ) ;
#9015 = DIRECTION ( 'NONE',  ( -7.147005652999508048E-36, 5.642372883946980038E-36, 1.000000000000000000 ) ) ;
#9016 = COLOUR_RGB ( '', 0.08235294, 0.09019608, 0.10196078) ;
#9017 = CARTESIAN_POINT ( 'NONE',  ( 0.000000000000000000, 0.000000000000000000, 0.000000000000000000 ) ) ;
#9018 = CARTESIAN_POINT ( 'NONE',  ( 2.691259848637810315, -10.67213569177517485, -30.37695071776536793 ) ) ;
#9019 = ORIENTED_EDGE ( 'NONE', *, *, #11446, .F. ) ;
#9020 = DIRECTION ( 'NONE',  ( 0.000000000000000000, 0.000000000000000000, -1.000000000000000000 ) ) ;
#9021 = CARTESIAN_POINT ( 'NONE',  ( 0.000000000000000000, 5.499999999999991118, -175.5000000000000000 ) ) ;
#9022 = DIRECTION ( 'NONE',  ( 0.000000000000000000, 1.000000000000000000, -0.000000000000000000 ) ) ;
#9023 = CARTESIAN_POINT ( 'NONE',  ( -3.175426480542816510, 5.499999999999865885, -164.8750000000000568 ) ) ;
#9024 = CARTESIAN_POINT ( 'NONE',  ( 116.9374999999998295, 2.500000000000024425, -1.035533905932629173 ) ) ;
#9025 = CARTESIAN_POINT ( 'NONE',  ( -3.175426480542816066, -5.500000000000057732, -108.8750000000000426 ) ) ;
#9026 = SURFACE_SIDE_STYLE ('',( #9635 ) ) ;
#9027 = CARTESIAN_POINT ( 'NONE',  ( 5.196152422706629359, -2.999999999999988898, -122.2886751345948539 ) ) ;
#9028 = CARTESIAN_POINT ( 'NONE',  ( 3.175426480543072749, -5.500000000000105693, -93.62500000000002842 ) ) ;
#9029 = CARTESIAN_POINT ( 'NONE',  ( 159.1086002691896226, -2.071067811865468400, -4.999999999999989342 ) ) ;
#9030 = CARTESIAN_POINT ( 'NONE',  ( 0.7577100060955550553, -15.57040985681421219, 7.988286010711783014 ) ) ;
#9031 = ORIENTED_EDGE ( 'NONE', *, *, #23349, .F. ) ;
#9032 = CARTESIAN_POINT ( 'NONE',  ( 11.75000000000009415, 1.873492889145067508, 1.873492889144734441 ) ) ;
#9033 = CARTESIAN_POINT ( 'NONE',  ( 116.1249999999999574, 1.767766952966265404, 1.767766952966431937 ) ) ;
#9034 = CARTESIAN_POINT ( 'NONE',  ( -5.999999999999962697, 3.323446944526963891E-14, -161.9136751345948539 ) ) ;
#9035 = CARTESIAN_POINT ( 'NONE',  ( 108.3752832217622739, 1.849990392679523588, 0.000000000000000000 ) ) ;
#9036 = CARTESIAN_POINT ( 'NONE',  ( -5.999999999999964473, 9.063946212346262433E-15, -173.9136751345948255 ) ) ;
#9037 =( BOUNDED_CURVE ( )  B_SPLINE_CURVE ( 2, ( #28385, #11712, #9680, #4598, #6906, #16625, #21209, #14029, #27781 ),
 .UNSPECIFIED., .F., .T. ) 
 B_SPLINE_CURVE_WITH_KNOTS ( ( 3, 2, 2, 2, 3 ),
 ( 0.8861111111111110716, 0.8870370370370370683, 0.8888888888888888395, 0.8907407407407407218, 0.8916666666666666075 ),
 .UNSPECIFIED. ) 
 CURVE ( )  GEOMETRIC_REPRESENTATION_ITEM ( )  RATIONAL_B_SPLINE_CURVE ( ( 0.9330127018922194093, 0.9330127018922154125, 1.000000000000000000, 0.8660254037844388186, 1.000000000000000000, 0.8660254037844388186, 1.000000000000000000, 0.9330127018922234061, 0.9330127018922194093 ) ) 
 REPRESENTATION_ITEM ( '' )  );
#9038 = VERTEX_POINT ( 'NONE', #7012 ) ;
#9039 = EDGE_CURVE ( 'NONE', #11924, #21660, #4557, .T. ) ;
#9040 = CARTESIAN_POINT ( 'NONE',  ( 5.412658773652712085, -3.125000000000086153, -90.06698729810780435 ) ) ;
#9041 = ORIENTED_EDGE ( 'NONE', *, *, #20256, .T. ) ;
#9042 = CARTESIAN_POINT ( 'NONE',  ( 6.000000000000052403, -1.607695154586662678, -65.23066243270255882 ) ) ;
#9043 = ORIENTED_EDGE ( 'NONE', *, *, #9291, .T. ) ;
#9044 = CARTESIAN_POINT ( 'NONE',  ( 148.4062500000000568, 6.000000000000005329, -2.485281374238555774 ) ) ;
#9045 = EDGE_LOOP ( 'NONE', ( #30033, #27066, #21826, #29681 ) ) ;
#9046 = CARTESIAN_POINT ( 'NONE',  ( 6.350852961086080661, -9.614813431917819062E-14, -124.8749999999999858 ) ) ;
#9047 = CARTESIAN_POINT ( 'NONE',  ( 22.06250000000009237, -1.097466725451379244, -2.649519052838538613 ) ) ;
#9048 = EDGE_CURVE ( 'NONE', #18703, #1706, #26243, .T. ) ;
#9049 = CARTESIAN_POINT ( 'NONE',  ( -7.216878364870328078, 0.000000000000000000, -127.5580127018922241 ) ) ;
#9050 = ORIENTED_EDGE ( 'NONE', *, *, #29771, .T. ) ;
#9051 = DIRECTION ( 'NONE',  ( 1.000000000000000000, -5.551115123125773458E-17, -1.260129944081490338E-35 ) ) ;
#9052 = CARTESIAN_POINT ( 'NONE',  ( 5.412658773652739619, 3.124999999999988898, -170.8169872981077901 ) ) ;
#9053 = CARTESIAN_POINT ( 'NONE',  ( -5.412658773652739619, 3.124999999999975131, -173.3169872981078470 ) ) ;
#9054 = SURFACE_STYLE_USAGE ( .BOTH. , #29626 ) ;
#9055 = DIRECTION ( 'NONE',  ( -7.147005652999508048E-36, 5.642372883946980038E-36, 1.000000000000000000 ) ) ;
#9056 = CARTESIAN_POINT ( 'NONE',  ( 13.06249999999998046, 2.000000000000151879, 0.8284271247461152399 ) ) ;
#9057 = DIRECTION ( 'NONE',  ( -0.000000000000000000, -0.5151515151515151381, -0.8570991287109668288 ) ) ;
#9058 = CARTESIAN_POINT ( 'NONE',  ( -2.081668171172168020E-16, -5.204170427930420051E-17, 2.499999999999999112 ) ) ;
#9059 = CARTESIAN_POINT ( 'NONE',  ( 111.5627832217621744, 0.7662911109078588412, 1.849990392679712103 ) ) ;
#9060 = CARTESIAN_POINT ( 'NONE',  ( 2.775557561562891351E-14, -6.250000000000061284, -73.81698729810781856 ) ) ;
#9061 = CARTESIAN_POINT ( 'NONE',  ( -5.412658773652739619, 3.124999999999975131, -63.81698729810780435 ) ) ;
#9062 = CARTESIAN_POINT ( 'NONE',  ( -3.175426480542816510, 5.499999999999865885, -49.37500000000000711 ) ) ;
#9063 = CARTESIAN_POINT ( 'NONE',  ( -0.5631067912581171342, -9.873786417483785272, -4.496381089953987775 ) ) ;
#9064 = CARTESIAN_POINT ( 'NONE',  ( 5.196152422706629359, -2.999999999999988898, -123.2113248654052029 ) ) ;
#9065 = DIRECTION ( 'NONE',  ( 1.000000000000000000, 0.000000000000000000, 0.000000000000000000 ) ) ;
#9066 = CARTESIAN_POINT ( 'NONE',  ( -2.775557561562891351E-14, -5.500000000000115463, -117.7500000000000284 ) ) ;
#9067 = CARTESIAN_POINT ( 'NONE',  ( 154.3988248654052313, 3.889087296526011706, 3.889087296526011706 ) ) ;
#9068 = VERTEX_POINT ( 'NONE', #25434 ) ;
#9069 = CARTESIAN_POINT ( 'NONE',  ( 20.25000000000001776, -1.873492889144900975, -1.873492889145178530 ) ) ;
#9070 = CARTESIAN_POINT ( 'NONE',  ( -1.110223024625164676E-16, 2.000000000000012879, 2.021286199229734960E-15 ) ) ;
#9071 = CARTESIAN_POINT ( 'NONE',  ( 6.000000000000000888, -3.330669073875464691E-16, -7.560779664488942560E-35 ) ) ;
#9072 = VERTEX_POINT ( 'NONE', #20702 ) ;
#9073 = CARTESIAN_POINT ( 'NONE',  ( 110.6247167782374987, 1.849990392679551343, 0.000000000000000000 ) ) ;
#9074 = CARTESIAN_POINT ( 'NONE',  ( 0.000000000000000000, 5.999999999999977796, -121.7886751345948539 ) ) ;
#9075 = CARTESIAN_POINT ( 'NONE',  ( 111.3122167782374277, -0.7662911109076785410, -1.849990392679291551 ) ) ;
#9076 = ADVANCED_FACE ( 'NONE', ( #30052 ), #15518, .F. ) ;
#9077 = CARTESIAN_POINT ( 'NONE',  ( -5.412658773652684552, -3.125000000000099920, -110.0669872981078186 ) ) ;
#9078 = CARTESIAN_POINT ( 'NONE',  ( 5.999999999999949374, 1.607695154586804565, -108.5966878364870496 ) ) ;
#9079 = CARTESIAN_POINT ( 'NONE',  ( 110.7113248654050182, 2.000000000000057288, 0.000000000000000000 ) ) ;
#9080 = ORIENTED_EDGE ( 'NONE', *, *, #27707, .T. ) ;
#9081 = ORIENTED_EDGE ( 'NONE', *, *, #5378, .T. ) ;
#9082 = CARTESIAN_POINT ( 'NONE',  ( 20.66367513459499605, -1.767766952966265404, 1.767766952966320915 ) ) ;
#9083 = CARTESIAN_POINT ( 'NONE',  ( 135.5625000000000284, -4.242640687119298093, 4.242640687119298093 ) ) ;
#9084 = EDGE_CURVE ( 'NONE', #2061, #7050, #13823, .T. ) ;
#9085 = AXIS2_PLACEMENT_3D ( 'NONE', #646, #10030, #19407 ) ;
#9086 = CARTESIAN_POINT ( 'NONE',  ( -5.412658773652684552, -3.125000000000099920, -140.0669872981078470 ) ) ;
#9087 = CARTESIAN_POINT ( 'NONE',  ( -5.196152422706601826, 2.999999999999975131, -150.9613248654052597 ) ) ;
#9088 = CARTESIAN_POINT ( 'NONE',  ( 21.62500000000017053, -1.414213562372979016, -1.414213562373090038 ) ) ;
#9089 = FILL_AREA_STYLE ('',( #13900 ) ) ;
#9090 = CARTESIAN_POINT ( 'NONE',  ( 0.000000000000000000, -5.999999999999991118, -137.5386751345948255 ) ) ;
#9091 = CARTESIAN_POINT ( 'NONE',  ( 5.412658773652739619, 3.124999999999988898, -68.18301270189225249 ) ) ;
#9092 = CARTESIAN_POINT ( 'NONE',  ( 146.9851497308104342, -3.535533905932725318, 3.535533905932725318 ) ) ;
#9093 = CARTESIAN_POINT ( 'NONE',  ( 111.7886751345948255, -1.999999999999974021, 0.000000000000000000 ) ) ;
#9094 = CARTESIAN_POINT ( 'NONE',  ( 3.464101615137852974, 5.999999999999884537, -73.91367513459483973 ) ) ;
#9095 = CARTESIAN_POINT ( 'NONE',  ( 3.464101615137852974, 5.999999999999884537, -165.4136751345947687 ) ) ;
#9096 = CARTESIAN_POINT ( 'NONE',  ( 155.9136751345948539, 0.000000000000000000, -5.500000000000005329 ) ) ;
#9097 = CARTESIAN_POINT ( 'NONE',  ( 16.66367513459490723, -1.767766952966265404, 1.767766952966376426 ) ) ;
#9098 = CARTESIAN_POINT ( 'NONE',  ( 109.8124999999997868, 1.035533905932779275, -2.499999999999784173 ) ) ;
#9099 = DIRECTION ( 'NONE',  ( -7.147005652999508048E-36, 5.642372883946980038E-36, 1.000000000000000000 ) ) ;
#9100 = CARTESIAN_POINT ( 'NONE',  ( -6.350852961085760029, -1.281975124255709124E-13, -127.1249999999999858 ) ) ;
#9101 = CARTESIAN_POINT ( 'NONE',  ( -5.999999999999963585, 1.780251999655701777E-13, -53.33632486540522422 ) ) ;
#9102 = CARTESIAN_POINT ( 'NONE',  ( -7.216878364870328078, 0.000000000000000000, -142.5580127018922667 ) ) ;
#9103 = FACE_OUTER_BOUND ( 'NONE', #27751, .T. ) ;
#9104 = CARTESIAN_POINT ( 'NONE',  ( 0.000000000000000000, 0.000000000000000000, 0.000000000000000000 ) ) ;
#9105 = EDGE_LOOP ( 'NONE', ( #9735, #24788, #5949, #7998 ) ) ;
#9106 = CARTESIAN_POINT ( 'NONE',  ( 4.763139720814407951, 2.750000000000002665, -51.25000000000001421 ) ) ;
#9107 = CARTESIAN_POINT ( 'NONE',  ( 125.0000000000000568, -55.00000000000000711, 5.000000000000004441 ) ) ;
#9108 = CARTESIAN_POINT ( 'NONE',  ( 13.99999999999999822, 0.000000000000000000, 0.000000000000000000 ) ) ;
#9109 = DIRECTION ( 'NONE',  ( -0.000000000000000000, -0.000000000000000000, -1.000000000000000000 ) ) ;
#9110 = ORIENTED_EDGE ( 'NONE', *, *, #16274, .T. ) ;
#9111 = CARTESIAN_POINT ( 'NONE',  ( 106.9999999999999716, 2.500000000000030198, 0.000000000000000000 ) ) ;
#9112 = CARTESIAN_POINT ( 'NONE',  ( 138.6562500000000284, -6.000000000000005329, 2.485281374238556218 ) ) ;
#9113 = CARTESIAN_POINT ( 'NONE',  ( 160.8011092498555854, -11.45390509671190493, -3.580702321368915531 ) ) ;
#9114 = EDGE_CURVE ( 'NONE', #14484, #20574, #4632, .T. ) ;
#9115 = CARTESIAN_POINT ( 'NONE',  ( 137.0625000000000284, -4.242640687119298093, 4.242640687119298093 ) ) ;
#9116 = CARTESIAN_POINT ( 'NONE',  ( 21.85117513459487171, -2.499999999999844569, -1.035533905932809473 ) ) ;
#9117 = CIRCLE ( 'NONE', #12564, 0.9999999999999991118 ) ;
#9118 = EDGE_CURVE ( 'NONE', #13233, #2648, #28922, .T. ) ;
#9119 = CARTESIAN_POINT ( 'NONE',  ( 4.763139720814407951, 2.750000000000002665, -135.2500000000000284 ) ) ;
#9120 = EDGE_LOOP ( 'NONE', ( #28813, #7539, #7402, #2448, #5128, #23856, #5694, #23030, #15889 ) ) ;
#9121 = CARTESIAN_POINT ( 'NONE',  ( 13.18750000000006928, 0.8284271247462955401, 2.000000000000031530 ) ) ;
#9122 = ORIENTED_EDGE ( 'NONE', *, *, #4067, .F. ) ;
#9123 = CARTESIAN_POINT ( 'NONE',  ( 0.000000000000000000, 5.499999999999991118, -66.00000000000000000 ) ) ;
#9124 = CARTESIAN_POINT ( 'NONE',  ( 10.00000000000014566, 1.942114083715059225, -0.8533076016160290322 ) ) ;
#9125 =( BOUNDED_CURVE ( )  B_SPLINE_CURVE ( 2, ( #1065, #3061, #12779, #19524, #3201, #21824, #28858, #10454, #26847 ),
 .UNSPECIFIED., .F., .T. ) 
 B_SPLINE_CURVE_WITH_KNOTS ( ( 3, 2, 2, 2, 3 ),
 ( 0.9750000000000000888, 0.9759259259259259744, 0.9777777777777777457, 0.9796296296296296280, 0.9805555555555555136 ),
 .UNSPECIFIED. ) 
 CURVE ( )  GEOMETRIC_REPRESENTATION_ITEM ( )  RATIONAL_B_SPLINE_CURVE ( ( 0.9330127018922194093, 0.9330127018922234061, 1.000000000000000000, 0.8660254037844388186, 1.000000000000000000, 0.8660254037844388186, 1.000000000000000000, 0.9330127018922234061, 0.9330127018922194093 ) ) 
 REPRESENTATION_ITEM ( '' )  );
#9126 = EDGE_LOOP ( 'NONE', ( #2017, #13123, #12746, #15508 ) ) ;
#9127 = CARTESIAN_POINT ( 'NONE',  ( -5.999999999999963585, 1.780251999655701777E-13, -57.83632486540521711 ) ) ;
#9128 = STYLED_ITEM ( 'NONE', ( #14310 ), #7131 ) ;
#9129 = CARTESIAN_POINT ( 'NONE',  ( 5.999999999999988454, 1.607695154586737729, -150.5966878364870638 ) ) ;
#9130 = CARTESIAN_POINT ( 'NONE',  ( 140.5573082070725093, -11.11461641399627531, -4.524920606408968204 ) ) ;
#9131 = CARTESIAN_POINT ( 'NONE',  ( 119.1877832217621034, 0.7662911109078588412, -1.849990392679411677 ) ) ;
#9132 = CARTESIAN_POINT ( 'NONE',  ( -2.775557561562891351E-14, -5.500000000000115463, -146.2500000000000000 ) ) ;
#9133 = CARTESIAN_POINT ( 'NONE',  ( 139.8004524783788725, -8.830548176177012820, -8.125740240671891712 ) ) ;
#9134 = CARTESIAN_POINT ( 'NONE',  ( 3.175426480543072749, 5.499999999999865885, -142.6250000000000000 ) ) ;
#9135 = CARTESIAN_POINT ( 'NONE',  ( 5.412658773652739619, 3.124999999999988898, -162.6830127018922383 ) ) ;
#9136 = CARTESIAN_POINT ( 'NONE',  ( 20.99177011976446749, 10.49588505988222842, 1.500282997124228146E-34 ) ) ;
#9137 = CARTESIAN_POINT ( 'NONE',  ( 5.196152422706629359, 3.000000000000002665, -89.96132486540520290 ) ) ;
#9138 = VECTOR ( 'NONE', #17735, 1000.000000000000000 ) ;
#9139 = CARTESIAN_POINT ( 'NONE',  ( -3.175426480542816066, -5.500000000000057732, -75.87500000000001421 ) ) ;
#9140 = CARTESIAN_POINT ( 'NONE',  ( -10.00000000000000178, -89.00000000000001421, 3.000000000000002665 ) ) ;
#9141 = CARTESIAN_POINT ( 'NONE',  ( -2.775557561562891351E-14, -5.500000000000115463, -74.25000000000004263 ) ) ;
#9142 = CARTESIAN_POINT ( 'NONE',  ( 140.0000000000000284, -9.835770062369604716, 7.609486625086941736 ) ) ;
#9143 = CARTESIAN_POINT ( 'NONE',  ( -5.196152422706573404, -3.000000000000002665, -88.28867513459482552 ) ) ;
#9144 = DIRECTION ( 'NONE',  ( -1.000000000000000000, -0.000000000000000000, -0.000000000000000000 ) ) ;
#9145 = CARTESIAN_POINT ( 'NONE',  ( 156.5625000000000284, -4.242640687119298093, 4.242640687119298093 ) ) ;
#9146 = FILL_AREA_STYLE_COLOUR ( '', #6934 ) ;
#9147 = CARTESIAN_POINT ( 'NONE',  ( 20.25000000000015632, 1.110223024625156540E-13, 1.999999999999946265 ) ) ;
#9148 = CARTESIAN_POINT ( 'NONE',  ( 5.999999999999949374, 1.607695154586804565, -95.09668783648706381 ) ) ;
#9149 = EDGE_CURVE ( 'NONE', #12427, #17415, #245, .T. ) ;
#9150 = DIRECTION ( 'NONE',  ( 1.000000000000000000, 0.000000000000000000, 0.000000000000000000 ) ) ;
#9151 = EDGE_CURVE ( 'NONE', #23842, #30226, #4809, .T. ) ;
#9152 = VERTEX_POINT ( 'NONE', #840 ) ;
#9153 = CARTESIAN_POINT ( 'NONE',  ( 155.1562500000000284, -6.000000000000005329, 2.485281374238555774 ) ) ;
#9154 = CARTESIAN_POINT ( 'NONE',  ( 3.464101615137757051, -5.999999999999979572, -156.9136751345947971 ) ) ;
#9155 = CARTESIAN_POINT ( 'NONE',  ( 113.7502832217623023, -1.308140751793585022, 1.308140751793640533 ) ) ;
#9156 = CARTESIAN_POINT ( 'NONE',  ( 11.46132486540535389, 1.110223024625156540E-13, -2.500000000000002220 ) ) ;
#9157 = ORIENTED_EDGE ( 'NONE', *, *, #1011, .T. ) ;
#9158 = ORIENTED_EDGE ( 'NONE', *, *, #12894, .F. ) ;
#9159 = VERTEX_POINT ( 'NONE', #19308 ) ;
#9160 = CARTESIAN_POINT ( 'NONE',  ( -6.350852961085760029, -1.281975124255709124E-13, -88.12500000000000000 ) ) ;
#9161 = CARTESIAN_POINT ( 'NONE',  ( 2.775557561562891351E-14, 6.250000000000033751, -108.4330127018922099 ) ) ;
#9162 = VERTEX_POINT ( 'NONE', #19160 ) ;
#9163 = CARTESIAN_POINT ( 'NONE',  ( 3.979146954363714350, 10.25926384964410509, -20.49296196285818894 ) ) ;
#9164 = CARTESIAN_POINT ( 'NONE',  ( 6.000000000000000888, -3.330669073875464691E-16, -7.560779664488942560E-35 ) ) ;
#9165 = CARTESIAN_POINT ( 'NONE',  ( 5.959171229995800623, -9.246457381727758218, -25.80348449789765297 ) ) ;
#9166 = ORIENTED_EDGE ( 'NONE', *, *, #22818, .F. ) ;
#9167 = DIRECTION ( 'NONE',  ( 1.000000000000000000, -5.551115123125773458E-17, -1.260129944081490338E-35 ) ) ;
#9168 = CARTESIAN_POINT ( 'NONE',  ( 0.000000000000000000, 5.499999999999991118, -169.4999999999999716 ) ) ;
#9169 = CARTESIAN_POINT ( 'NONE',  ( 147.1800748654052597, -2.278174593051996322, 5.500000000000026645 ) ) ;
#9170 = CARTESIAN_POINT ( 'NONE',  ( 4.763139720814407951, -2.749999999999988454, -165.4999999999999716 ) ) ;
#9171 = CIRCLE ( 'NONE', #17523, 10.49999999999999822 ) ;
#9172 = CARTESIAN_POINT ( 'NONE',  ( 113.1874999999998295, 1.035533905932779275, 2.500000000000205169 ) ) ;
#9173 = CARTESIAN_POINT ( 'NONE',  ( -6.350852961085760029, -1.281975124255709124E-13, -100.1250000000000568 ) ) ;
#9174 = CARTESIAN_POINT ( 'NONE',  ( 3.464101615137757051, -5.999999999999979572, -165.9136751345947403 ) ) ;
#9175 = CARTESIAN_POINT ( 'NONE',  ( 6.350852961086080661, -9.614813431917819062E-14, -100.8750000000000000 ) ) ;
#9176 = CARTESIAN_POINT ( 'NONE',  ( 116.0000000000000142, 0.000000000000000000, -5.500000000000000000 ) ) ;
#9177 = CARTESIAN_POINT ( 'NONE',  ( 158.4523502691896510, 0.000000000000000000, 5.000000000000004441 ) ) ;
#9178 = CARTESIAN_POINT ( 'NONE',  ( 0.7669223171414714102, -15.58766199952932041, 7.954545454545456806 ) ) ;
#9179 = CIRCLE ( 'NONE', #13646, 11.00000000000001599 ) ;
#9180 = VERTEX_POINT ( 'NONE', #21612 ) ;
#9181 = CARTESIAN_POINT ( 'NONE',  ( 10.00000000000017586, -1.873492889144789952, 1.873492889145011997 ) ) ;
#9182 = CARTESIAN_POINT ( 'NONE',  ( 117.1249999999999432, 1.767766952966320915, 1.767766952966431937 ) ) ;
#9183 = CARTESIAN_POINT ( 'NONE',  ( 3.464101615137852974, 5.999999999999884537, -130.3363248654052029 ) ) ;
#9184 = EDGE_CURVE ( 'NONE', #18727, #29595, #26342, .T. ) ;
#9185 = CARTESIAN_POINT ( 'NONE',  ( 105.6252832217623592, 0.000000000000000000, 1.849990392679523588 ) ) ;
#9186 = CARTESIAN_POINT ( 'NONE',  ( 157.6011751345948255, 3.889087296526011706, -3.889087296526011706 ) ) ;
#9187 = EDGE_CURVE ( 'NONE', #22372, #27165, #8957, .T. ) ;
#9188 = EDGE_LOOP ( 'NONE', ( #22454, #19334 ) ) ;
#9189 = ORIENTED_EDGE ( 'NONE', *, *, #676, .F. ) ;
#9190 = AXIS2_PLACEMENT_3D ( 'NONE', #17704, #22451, #22605 ) ;
#9191 = CARTESIAN_POINT ( 'NONE',  ( 6.000000000000052403, -1.607695154586662678, -75.15331216351297883 ) ) ;
#9192 = ORIENTED_EDGE ( 'NONE', *, *, #6855, .T. ) ;
#9193 = CARTESIAN_POINT ( 'NONE',  ( 148.1250000000000284, 0.000000000000000000, -6.000000000000005329 ) ) ;
#9194 = ORIENTED_EDGE ( 'NONE', *, *, #25421, .T. ) ;
#9195 = CARTESIAN_POINT ( 'NONE',  ( -4.763139720814407951, -2.750000000000016431, -111.9999999999999858 ) ) ;
#9196 = CARTESIAN_POINT ( 'NONE',  ( 21.12500000000011724, 1.665334536937734811E-13, -2.649519052838444910 ) ) ;
#9197 = CARTESIAN_POINT ( 'NONE',  ( 3.608439182435180470, -6.249999999999997335, -133.0580127018922667 ) ) ;
#9198 = ORIENTED_EDGE ( 'NONE', *, *, #6923, .T. ) ;
#9199 = DIRECTION ( 'NONE',  ( -7.147005652999508048E-36, 5.642372883946980038E-36, 1.000000000000000000 ) ) ;
#9200 = CARTESIAN_POINT ( 'NONE',  ( 3.608439182435180470, -6.249999999999997335, -168.1919872981078470 ) ) ;
#9201 = CARTESIAN_POINT ( 'NONE',  ( -3.608439182435052128, -6.250000000000110134, -178.9419872981078470 ) ) ;
#9202 = VECTOR ( 'NONE', #10748, 1000.000000000000000 ) ;
#9203 = CARTESIAN_POINT ( 'NONE',  ( 0.000000000000000000, 0.000000000000000000, 0.000000000000000000 ) ) ;
#9204 = ORIENTED_EDGE ( 'NONE', *, *, #5209, .T. ) ;
#9205 = CARTESIAN_POINT ( 'NONE',  ( -19.99999999999998224, -54.99999999999990763, 8.000000000000007105 ) ) ;
#9206 = CARTESIAN_POINT ( 'NONE',  ( -5.999999999999963585, -1.487416814333745711E-14, -128.9136751345948539 ) ) ;
#9207 = DIRECTION ( 'NONE',  ( -1.000000000000000000, -1.665334536937736783E-16, -2.220446049250315546E-16 ) ) ;
#9208 = CARTESIAN_POINT ( 'NONE',  ( 112.3988248654050039, -0.8284271247461453269, -1.999999999999731104 ) ) ;
#9209 = VECTOR ( 'NONE', #14944, 1000.000000000000000 ) ;
#9210 = CARTESIAN_POINT ( 'NONE',  ( 112.1877832217621886, 0.7662911109079189043, -1.849990392679291551 ) ) ;
#9211 = CARTESIAN_POINT ( 'NONE',  ( 2.775557561562891351E-14, 6.250000000000033751, -73.06698729810784698 ) ) ;
#9212 = CARTESIAN_POINT ( 'NONE',  ( -5.412658773652684552, -3.125000000000099920, -63.56698729810783277 ) ) ;
#9213 = EDGE_CURVE ( 'NONE', #14750, #891, #21335, .T. ) ;
#9214 = CARTESIAN_POINT ( 'NONE',  ( 3.175426480543072749, 5.499999999999865885, -49.62500000000001421 ) ) ;
#9215 = CARTESIAN_POINT ( 'NONE',  ( -38.99999999999998579, -59.99999999999980105, -3.000000000000002665 ) ) ;
#9216 = CARTESIAN_POINT ( 'NONE',  ( 118.2113248654050466, -1.999999999999946265, 2.220446049250313081E-13 ) ) ;
#9217 = CARTESIAN_POINT ( 'NONE',  ( 160.3062030939346130, -11.25163267815772805, -4.172369835259413406 ) ) ;
#9218 =( BOUNDED_CURVE ( )  B_SPLINE_CURVE ( 2, ( #26792, #5756, #24503, #1932, #30188, #9154, #18547, #11338, #23453 ),
 .UNSPECIFIED., .F., .T. ) 
 B_SPLINE_CURVE_WITH_KNOTS ( ( 3, 2, 2, 2, 3 ),
 ( 0.1805555555555555525, 0.1814814814814814936, 0.1833333333333333204, 0.1851851851851851749, 0.1861111111111111160 ),
 .UNSPECIFIED. ) 
 CURVE ( )  GEOMETRIC_REPRESENTATION_ITEM ( )  RATIONAL_B_SPLINE_CURVE ( ( 0.9330127018922196314, 0.9330127018922185211, 1.000000000000000000, 0.8660254037844388186, 1.000000000000000000, 0.8660254037844388186, 1.000000000000000000, 0.9330127018922184101, 0.9330127018922194093 ) ) 
 REPRESENTATION_ITEM ( '' )  );
#9219 = CARTESIAN_POINT ( 'NONE',  ( 4.763139720814407951, -2.749999999999988454, -123.5000000000000568 ) ) ;
#9220 = CARTESIAN_POINT ( 'NONE',  ( 135.0586387269457305, -7.769283529832271995, -8.294211448155943245 ) ) ;
#9221 = ORIENTED_EDGE ( 'NONE', *, *, #12507, .F. ) ;
#9222 = CARTESIAN_POINT ( 'NONE',  ( 20.87500000000008882, 1.110223024625156540E-13, 2.649519052838333888 ) ) ;
#9223 = EDGE_CURVE ( 'NONE', #28281, #1984, #1483, .T. ) ;
#9224 = ORIENTED_EDGE ( 'NONE', *, *, #18509, .F. ) ;
#9225 = VECTOR ( 'NONE', #121, 1000.000000000000000 ) ;
#9226 = CARTESIAN_POINT ( 'NONE',  ( 110.4372167782375840, 0.7662911109078888172, -1.849990392679231599 ) ) ;
#9227 = CARTESIAN_POINT ( 'NONE',  ( 3.464101615137757051, -5.999999999999979572, -114.9136751345948255 ) ) ;
#9228 = CARTESIAN_POINT ( 'NONE',  ( -3.608439182435115633, 6.249999999999965361, -108.9419872981077901 ) ) ;
#9229 = CARTESIAN_POINT ( 'NONE',  ( -5.999999999999962697, 3.323446944526963891E-14, -158.3363248654052313 ) ) ;
#9230 = CYLINDRICAL_SURFACE ( 'NONE', #9859, 2.499999999999999112 ) ;
#9231 = ORIENTED_EDGE ( 'NONE', *, *, #29804, .T. ) ;
#9232 = CARTESIAN_POINT ( 'NONE',  ( -5.196152422706573404, -3.000000000000002665, -142.2886751345948539 ) ) ;
#9233 = CARTESIAN_POINT ( 'NONE',  ( 133.5000000000000284, 6.000000000000005329, 0.000000000000000000 ) ) ;
#9234 = ORIENTED_EDGE ( 'NONE', *, *, #28099, .F. ) ;
#9235 = CARTESIAN_POINT ( 'NONE',  ( 2.775557561562891351E-14, 6.250000000000033751, -136.0669872981078470 ) ) ;
#9236 = CARTESIAN_POINT ( 'NONE',  ( 10.75000000000006573, -1.873492889144789952, 1.873492889144845464 ) ) ;
#9237 = CARTESIAN_POINT ( 'NONE',  ( 6.000000000000000888, -1.859271017917181981E-14, -93.08632486540523132 ) ) ;
#9238 = CARTESIAN_POINT ( 'NONE',  ( 21.87500000000011724, 1.414213562373201061, -1.414213562373090038 ) ) ;
#9239 = CARTESIAN_POINT ( 'NONE',  ( -4.999999999999990230, -24.99999999999999289, 8.000000000000007105 ) ) ;
#9240 = CARTESIAN_POINT ( 'NONE',  ( 3.608439182435180470, 6.249999999999982236, -68.05801270189226670 ) ) ;
#9241 = CARTESIAN_POINT ( 'NONE',  ( 146.3288997308104342, 4.999999999999989342, -2.071067811865468400 ) ) ;
#9242 = CARTESIAN_POINT ( 'NONE',  ( 11.78867513459488947, -2.499999999999891198, -2.220446049250313081E-13 ) ) ;
#9243 = CARTESIAN_POINT ( 'NONE',  ( 16.03867513459497474, 5.551115123125782702E-14, -2.500000000000057732 ) ) ;
#9244 = EDGE_CURVE ( 'NONE', #25491, #6464, #26760, .T. ) ;
#9245 = FILL_AREA_STYLE_COLOUR ( '', #12953 ) ;
#9246 = ADVANCED_FACE ( 'NONE', ( #10537 ), #6062, .T. ) ;
#9247 = CARTESIAN_POINT ( 'NONE',  ( 156.5699251345948255, 2.278174593052198382, 5.499999999999826805 ) ) ;
#9248 = CARTESIAN_POINT ( 'NONE',  ( 16.72617513459490723, -2.499999999999904521, 1.035533905932749299 ) ) ;
#9249 = CARTESIAN_POINT ( 'NONE',  ( 111.8749999999998437, 1.767766952966348670, -1.767766952966209892 ) ) ;
#9250 = CARTESIAN_POINT ( 'NONE',  ( 6.000000000000000888, 1.743066579297358182E-13, -94.58632486540521711 ) ) ;
#9251 = CARTESIAN_POINT ( 'NONE',  ( 4.763139720814407951, 2.750000000000002665, -123.2500000000000284 ) ) ;
#9252 = CARTESIAN_POINT ( 'NONE',  ( 15.58632486540523132, 1.767766952966487448, -1.767766952966431937 ) ) ;
#9253 = CARTESIAN_POINT ( 'NONE',  ( -3.608439182435052128, -6.250000000000110134, -143.8080127018922667 ) ) ;
#9254 = CARTESIAN_POINT ( 'NONE',  ( -5.196152422706601826, 2.999999999999975131, -148.5386751345948539 ) ) ;
#9255 = LINE ( 'NONE', #18650, #16137 ) ;
#9256 = ORIENTED_EDGE ( 'NONE', *, *, #14220, .T. ) ;
#9257 = CARTESIAN_POINT ( 'NONE',  ( 3.175426480543072749, -5.500000000000105693, -56.12500000000004263 ) ) ;
#9258 = CARTESIAN_POINT ( 'NONE',  ( 3.464101615137757051, -5.999999999999979572, -154.8363248654052029 ) ) ;
#9259 = EDGE_CURVE ( 'NONE', #283, #7046, #11959, .T. ) ;
#9260 = CARTESIAN_POINT ( 'NONE',  ( -3.464101615137725076, 5.999999999999979572, -121.0863248654051461 ) ) ;
#9261 = EDGE_CURVE ( 'NONE', #15213, #899, #3433, .T. ) ;
#9262 = AXIS2_PLACEMENT_3D ( 'NONE', #19243, #18955, #26276 ) ;
#9263 = EDGE_LOOP ( 'NONE', ( #8223, #6965, #28842, #28387 ) ) ;
#9264 = CARTESIAN_POINT ( 'NONE',  ( 106.6874999999998010, -1.035533905932689347, -2.499999999999784173 ) ) ;
#9265 = CARTESIAN_POINT ( 'NONE',  ( 142.5000000000000568, 6.000000000000005329, 0.000000000000000000 ) ) ;
#9266 = CARTESIAN_POINT ( 'NONE',  ( 3.608439182435180470, 6.249999999999982236, -106.1919872981078612 ) ) ;
#9267 = DIRECTION ( 'NONE',  ( -1.000000000000000000, -0.000000000000000000, -0.000000000000000000 ) ) ;
#9268 = CARTESIAN_POINT ( 'NONE',  ( 133.5937500000000284, 6.000000000000005329, 2.485281374238585972 ) ) ;
#9269 = CYLINDRICAL_SURFACE ( 'NONE', #18046, 6.000000000000000888 ) ;
#9270 = CARTESIAN_POINT ( 'NONE',  ( 3.175426480543072749, 5.499999999999865885, -139.6250000000000000 ) ) ;
#9271 = VERTEX_POINT ( 'NONE', #8199 ) ;
#9272 = CARTESIAN_POINT ( 'NONE',  ( 11.31250000000006573, -0.8284271247460553989, 2.000000000000031530 ) ) ;
#9273 = ORIENTED_EDGE ( 'NONE', *, *, #29373, .T. ) ;
#9274 = CARTESIAN_POINT ( 'NONE',  ( 4.763139720814407951, -2.749999999999988454, -65.00000000000000000 ) ) ;
#9275 = DIRECTION ( 'NONE',  ( -7.147005652999508048E-36, 5.642372883946980038E-36, 1.000000000000000000 ) ) ;
#9276 = CARTESIAN_POINT ( 'NONE',  ( 5.196152422706629359, -2.999999999999988898, -123.7886751345948539 ) ) ;
#9277 = VERTEX_POINT ( 'NONE', #27243 ) ;
#9278 = DIRECTION ( 'NONE',  ( 0.000000000000000000, 0.000000000000000000, 1.000000000000000000 ) ) ;
#9279 = ADVANCED_FACE ( 'NONE', ( #19891 ), #1748, .F. ) ;
#9280 = CARTESIAN_POINT ( 'NONE',  ( 105.8747167782375271, -2.775557561562891351E-14, 1.849990392679523588 ) ) ;
#9281 = CARTESIAN_POINT ( 'NONE',  ( 0.000000000000000000, 0.000000000000000000, 0.000000000000000000 ) ) ;
#9282 = CARTESIAN_POINT ( 'NONE',  ( 118.1252832217622881, -2.775557561562891351E-14, -1.849990392679523588 ) ) ;
#9283 = CARTESIAN_POINT ( 'NONE',  ( 0.000000000000000000, 5.499999999999991118, -148.5000000000000284 ) ) ;
#9284 = DIRECTION ( 'NONE',  ( 0.000000000000000000, 1.000000000000000000, -6.695352868347764161E-17 ) ) ;
#9285 = CARTESIAN_POINT ( 'NONE',  ( 0.000000000000000000, 5.499999999999991118, -135.0000000000000000 ) ) ;
#9286 = CARTESIAN_POINT ( 'NONE',  ( -3.608439182435115633, 6.249999999999965361, -163.8080127018922667 ) ) ;
#9287 = CARTESIAN_POINT ( 'NONE',  ( 20.99177011976446394, -10.49588505988223730, 2.684716942222302368E-34 ) ) ;
#9288 = CARTESIAN_POINT ( 'NONE',  ( 0.000000000000000000, 5.999999999999977796, -89.71132486540523132 ) ) ;
#9289 = CARTESIAN_POINT ( 'NONE',  ( -6.350852961085760029, -1.281975124255709124E-13, -79.12500000000001421 ) ) ;
#9290 = CARTESIAN_POINT ( 'NONE',  ( -6.000000000000023093, 1.607695154586625819, -173.4033121635129646 ) ) ;
#9291 = EDGE_CURVE ( 'NONE', #856, #18552, #94, .T. ) ;
#9292 = CARTESIAN_POINT ( 'NONE',  ( -3.175426480542816510, -5.500000000000057732, -66.87500000000002842 ) ) ;
#9293 = EDGE_CURVE ( 'NONE', #25418, #18127, #22203, .T. ) ;
#9294 = CARTESIAN_POINT ( 'NONE',  ( 140.0000000000000284, -10.00000000000000888, 7.500000000000007105 ) ) ;
#9295 = CARTESIAN_POINT ( 'NONE',  ( 148.7023502691896510, 0.000000000000000000, -5.000000000000004441 ) ) ;
#9296 = FACE_OUTER_BOUND ( 'NONE', #23818, .T. ) ;
#9297 = CARTESIAN_POINT ( 'NONE',  ( -4.999999999999984013, -65.50000000000001421, -8.000000000000007105 ) ) ;
#9298 = CARTESIAN_POINT ( 'NONE',  ( 160.2187500000000284, 2.485281374238556218, -6.000000000000005329 ) ) ;
#9299 = FILL_AREA_STYLE ('',( #9146 ) ) ;
#9300 = CARTESIAN_POINT ( 'NONE',  ( -5.999999999999919176, 1.607695154586804565, -94.48066243270258724 ) ) ;
#9301 = VECTOR ( 'NONE', #5617, 1000.000000000000000 ) ;
#9302 = DIRECTION ( 'NONE',  ( 0.000000000000000000, 0.000000000000000000, -1.000000000000000000 ) ) ;
#9303 = CARTESIAN_POINT ( 'NONE',  ( 117.1872167782373708, -1.849990392679441875, -0.7662911109077087390 ) ) ;
#9304 =( BOUNDED_CURVE ( )  B_SPLINE_CURVE ( 2, ( #7397, #4921, #28268, #24123, #21690, #179, #2773, #23837, #23692 ),
 .UNSPECIFIED., .F., .F. ) 
 B_SPLINE_CURVE_WITH_KNOTS ( ( 3, 2, 2, 2, 3 ),
 ( 0.7416666666666666963, 0.7425925925925925819, 0.7444444444444444642, 0.7462962962962962354, 0.7472222222222222321 ),
 .UNSPECIFIED. ) 
 CURVE ( )  GEOMETRIC_REPRESENTATION_ITEM ( )  RATIONAL_B_SPLINE_CURVE ( ( 0.9330127018922194093, 0.9330127018922234061, 1.000000000000000000, 0.8660254037844388186, 1.000000000000000000, 0.8660254037844388186, 1.000000000000000000, 0.9330127018922194093, 0.9330127018922194093 ) ) 
 REPRESENTATION_ITEM ( '' )  );
#9305 = EDGE_LOOP ( 'NONE', ( #309, #10357, #2403, #1728 ) ) ;
#9306 = VECTOR ( 'NONE', #13098, 1000.000000000000000 ) ;
#9307 = CARTESIAN_POINT ( 'NONE',  ( 151.8750000000000284, 0.000000000000000000, 6.000000000000005329 ) ) ;
#9308 = CARTESIAN_POINT ( 'NONE',  ( 9.999999999999980460, 2.500000000000002220, 0.000000000000000000 ) ) ;
#9309 = CARTESIAN_POINT ( 'NONE',  ( 113.1877832217620892, 0.7662911109079189043, -1.849990392679291551 ) ) ;
#9310 = CYLINDRICAL_SURFACE ( 'NONE', #13653, 6.000000000000000888 ) ;
#9311 = VERTEX_POINT ( 'NONE', #15319 ) ;
#9312 = ORIENTED_EDGE ( 'NONE', *, *, #18397, .T. ) ;
#9313 =( BOUNDED_CURVE ( )  B_SPLINE_CURVE ( 2, ( #7970, #12332, #12937, #24555, #29005, #17232, #17533, #29313, #22273 ),
 .UNSPECIFIED., .F., .T. ) 
 B_SPLINE_CURVE_WITH_KNOTS ( ( 3, 2, 2, 2, 3 ),
 ( 0.1027777777777777735, 0.1037037037037037007, 0.1055555555555555552, 0.1074074074074074098, 0.1083333333333333370 ),
 .UNSPECIFIED. ) 
 CURVE ( )  GEOMETRIC_REPRESENTATION_ITEM ( )  RATIONAL_B_SPLINE_CURVE ( ( 0.9330127018922194093, 0.9330127018922194093, 1.000000000000000000, 0.8660254037844388186, 1.000000000000000000, 0.8660254037844388186, 1.000000000000000000, 0.9330127018922194093, 0.9330127018922194093 ) ) 
 REPRESENTATION_ITEM ( '' )  );
#9314 = ORIENTED_EDGE ( 'NONE', *, *, #5980, .F. ) ;
#9315 = CARTESIAN_POINT ( 'NONE',  ( 3.175426480543072749, 5.499999999999865885, -91.62500000000001421 ) ) ;
#9316 = CARTESIAN_POINT ( 'NONE',  ( -3.608439182435115633, 6.249999999999965361, -103.8080127018922525 ) ) ;
#9317 = ORIENTED_EDGE ( 'NONE', *, *, #7241, .T. ) ;
#9318 = CARTESIAN_POINT ( 'NONE',  ( 4.763867271839615114, 9.917884865257411420, -21.33175192690179856 ) ) ;
#9319 = CARTESIAN_POINT ( 'NONE',  ( 155.1413997308104342, 2.071067811865468400, -4.999999999999989342 ) ) ;
#9320 = CARTESIAN_POINT ( 'NONE',  ( 0.000000000000000000, 5.499999999999991118, -165.0000000000000284 ) ) ;
#9321 = ADVANCED_FACE ( 'NONE', ( #3588 ), #10705, .T. ) ;
#9322 = CARTESIAN_POINT ( 'NONE',  ( 159.4613248654052029, -5.500000000000005329, 0.000000000000000000 ) ) ;
#9323 = ORIENTED_EDGE ( 'NONE', *, *, #11444, .F. ) ;
#9324 = SHAPE_REPRESENTATION_RELATIONSHIP ( 'NONE' , 'NONE' ,  #7189, #3017 ) ;
#9325 = VECTOR ( 'NONE', #5736, 1000.000000000000000 ) ;
#9326 = CARTESIAN_POINT ( 'NONE',  ( -4.763139720814407951, 2.749999999999946709, -175.2500000000000284 ) ) ;
#9327 = CARTESIAN_POINT ( 'NONE',  ( 3.175426480543072749, -5.500000000000105693, -152.1250000000000568 ) ) ;
#9328 = AXIS2_PLACEMENT_3D ( 'NONE', #29636, #24876, #22285 ) ;
#9329 = CARTESIAN_POINT ( 'NONE',  ( 110.9374999999997442, 2.500000000000055067, -1.035533905932388699 ) ) ;
#9330 = STYLED_ITEM ( 'NONE', ( #25122 ), #943 ) ;
#9331 = CARTESIAN_POINT ( 'NONE',  ( 0.000000000000000000, -5.999999999999991118, -166.0386751345947971 ) ) ;
#9332 = EDGE_CURVE ( 'NONE', #25088, #25878, #3622, .T. ) ;
#9333 = CARTESIAN_POINT ( 'NONE',  ( 4.763139720814407951, 2.750000000000002665, -94.75000000000000000 ) ) ;
#9334 = DIRECTION ( 'NONE',  ( 0.000000000000000000, -0.9730085108210397848, -0.2307692307692307265 ) ) ;
#9335 = FILL_AREA_STYLE ('',( #20712 ) ) ;
#9336 = CARTESIAN_POINT ( 'NONE',  ( 0.1053031288715569197, -15.23283975038563298, 8.619984219653423096 ) ) ;
#9337 = VERTEX_POINT ( 'NONE', #5589 ) ;
#9338 = CARTESIAN_POINT ( 'NONE',  ( 11.12500000000016342, -2.649519052838222866, 0.000000000000000000 ) ) ;
#9339 = CARTESIAN_POINT ( 'NONE',  ( 114.4999999999998721, -2.499999999999891198, 0.000000000000000000 ) ) ;
#9340 = CARTESIAN_POINT ( 'NONE',  ( 12.89882486540518336, 1.035533905932689347, 2.499999999999784173 ) ) ;
#9341 = CARTESIAN_POINT ( 'NONE',  ( 106.8752832217622739, -1.849990392679301543, 2.220446049250313081E-13 ) ) ;
#9342 = CARTESIAN_POINT ( 'NONE',  ( -1.000000000000000888, -19.99999999999998934, 5.000000000000004441 ) ) ;
#9343 = ORIENTED_EDGE ( 'NONE', *, *, #22445, .F. ) ;
#9344 = CARTESIAN_POINT ( 'NONE',  ( -6.000000000000000888, 1.067854986875958443E-15, 7.560779664488942560E-35 ) ) ;
#9345 = LINE ( 'NONE', #25775, #20185 ) ;
#9346 = CARTESIAN_POINT ( 'NONE',  ( 106.3122167782376124, -0.7662911109076184779, -1.849990392679351725 ) ) ;
#9347 = VECTOR ( 'NONE', #17343, 1000.000000000000000 ) ;
#9348 = ORIENTED_EDGE ( 'NONE', *, *, #4997, .T. ) ;
#9349 = FACE_OUTER_BOUND ( 'NONE', #25331, .T. ) ;
#9350 = AXIS2_PLACEMENT_3D ( 'NONE', #27640, #25188, #3998 ) ;
#9351 = CARTESIAN_POINT ( 'NONE',  ( 149.3437500000000284, -6.000000000000005329, -2.485281374238555774 ) ) ;
#9352 = VERTEX_POINT ( 'NONE', #24332 ) ;
#9353 = CARTESIAN_POINT ( 'NONE',  ( -2.775557561562891351E-14, -5.500000000000115463, -116.2500000000000142 ) ) ;
#9354 = CARTESIAN_POINT ( 'NONE',  ( 24.00000000000013145, -1.873492889144789952, -1.873492889144956486 ) ) ;
#9355 = CARTESIAN_POINT ( 'NONE',  ( -3.608439182435052128, -6.250000000000110134, -131.8080127018922383 ) ) ;
#9356 = ORIENTED_EDGE ( 'NONE', *, *, #3289, .T. ) ;
#9357 = CYLINDRICAL_SURFACE ( 'NONE', #8292, 6.000000000000000888 ) ;
#9358 = CARTESIAN_POINT ( 'NONE',  ( -5.412658773652684552, -3.125000000000099920, -168.5669872981078186 ) ) ;
#9359 = CARTESIAN_POINT ( 'NONE',  ( 107.4999999999999716, -2.499999999999891198, 3.330669073875469621E-13 ) ) ;
#9360 = EDGE_CURVE ( 'NONE', #12840, #17900, #3286, .T. ) ;
#9361 = EDGE_CURVE ( 'NONE', #13814, #25453, #7939, .T. ) ;
#9362 = CARTESIAN_POINT ( 'NONE',  ( 5.999999999999949374, 1.607695154586804565, -96.01933756729745539 ) ) ;
#9363 = CARTESIAN_POINT ( 'NONE',  ( 130.0000000000000284, -60.00000000000001421, 3.000000000000002665 ) ) ;
#9364 = CARTESIAN_POINT ( 'NONE',  ( 23.39882486540530593, -1.035533905932689347, -2.500000000000024425 ) ) ;
#9365 = CARTESIAN_POINT ( 'NONE',  ( 107.5002832217622881, 1.308140751793585022, 1.308140751793751555 ) ) ;
#9366 = CARTESIAN_POINT ( 'NONE',  ( -5.412658773652739619, 3.124999999999975131, -175.6830127018922383 ) ) ;
#9367 = CARTESIAN_POINT ( 'NONE',  ( -0.02602735246118789356, -9.486986323769393437, -4.738252045315884509 ) ) ;
#9368 = CARTESIAN_POINT ( 'NONE',  ( 3.464101615137757051, -5.999999999999979572, -48.33632486540521711 ) ) ;
#9369 = PRESENTATION_LAYER_ASSIGNMENT (  '', '', ( #23108 ) ) ;
#9370 = CARTESIAN_POINT ( 'NONE',  ( -5.999999999999957367, 1.607695154586737507, -158.9806624327025872 ) ) ;
#9371 = CARTESIAN_POINT ( 'NONE',  ( -3.175426480542816510, 5.499999999999865885, -122.8749999999999858 ) ) ;
#9372 = VECTOR ( 'NONE', #18872, 1000.000000000000000 ) ;
#9373 = CARTESIAN_POINT ( 'NONE',  ( 135.0102241059247774, -7.375790388331942893, -8.398163806897956718 ) ) ;
#9374 = CARTESIAN_POINT ( 'NONE',  ( 3.464101615137852974, 5.999999999999884537, -145.9136751345947687 ) ) ;
#9375 = ORIENTED_EDGE ( 'NONE', *, *, #4146, .F. ) ;
#9376 = CARTESIAN_POINT ( 'NONE',  ( 21.18750000000013500, -2.649519052838178457, -1.097466725451559322 ) ) ;
#9377 = CARTESIAN_POINT ( 'NONE',  ( -0.02669168755773660903, -15.33239425769398423, -6.888162703249225416 ) ) ;
#9378 = CARTESIAN_POINT ( 'NONE',  ( 143.2574251345948255, -2.278174593051702335, 5.500000000000323297 ) ) ;
#9379 = ORIENTED_EDGE ( 'NONE', *, *, #25394, .F. ) ;
#9380 = CARTESIAN_POINT ( 'NONE',  ( 110.9372167782374277, -0.7662911109077686911, 1.849990392679591977 ) ) ;
#9381 = DIRECTION ( 'NONE',  ( -7.147005652999508048E-36, 5.642372883946980038E-36, 1.000000000000000000 ) ) ;
#9382 = CARTESIAN_POINT ( 'NONE',  ( -5.412658773652684552, -3.125000000000099920, -111.5669872981078186 ) ) ;
#9383 = ORIENTED_EDGE ( 'NONE', *, *, #10474, .F. ) ;
#9384 = CARTESIAN_POINT ( 'NONE',  ( 0.000000000000000000, -5.999999999999991118, -95.53867513459479710 ) ) ;
#9385 = CARTESIAN_POINT ( 'NONE',  ( -4.999999999999886313, -70.00000000000001421, -5.000000000000004441 ) ) ;
#9386 = ORIENTED_EDGE ( 'NONE', *, *, #15018, .F. ) ;
#9387 = VERTEX_POINT ( 'NONE', #6673 ) ;
#9388 = CARTESIAN_POINT ( 'NONE',  ( 151.7738248654052597, -3.889087296526011706, 3.889087296526011706 ) ) ;
#9389 = CARTESIAN_POINT ( 'NONE',  ( 138.5625000000000284, -4.242640687119298093, 4.242640687119298093 ) ) ;
#9390 =( GEOMETRIC_REPRESENTATION_CONTEXT ( 3 ) GLOBAL_UNCERTAINTY_ASSIGNED_CONTEXT ( ( #23802 ) ) GLOBAL_UNIT_ASSIGNED_CONTEXT ( ( #29198, #27206, #24765 ) ) REPRESENTATION_CONTEXT ( 'NONE', 'WORKASPACE' ) );
#9391 = CARTESIAN_POINT ( 'NONE',  ( -5.412658773652739619, 3.124999999999975131, -140.3169872981078186 ) ) ;
#9392 = DIRECTION ( 'NONE',  ( 0.000000000000000000, 0.000000000000000000, -1.000000000000000000 ) ) ;
#9393 = AXIS2_PLACEMENT_3D ( 'NONE', #26992, #17216, #22569 ) ;
#9394 = AXIS2_PLACEMENT_3D ( 'NONE', #16620, #18761, #28672 ) ;
#9395 = CARTESIAN_POINT ( 'NONE',  ( 12.50000000000006750, 1.873492889145011997, 1.873492889144734441 ) ) ;
#9396 = CARTESIAN_POINT ( 'NONE',  ( 3.464101615137852974, 5.999999999999884537, -151.3363248654051745 ) ) ;
#9397 = CARTESIAN_POINT ( 'NONE',  ( 18.06250000000005684, 2.000000000000151879, 0.8284271247461152399 ) ) ;
#9398 = CARTESIAN_POINT ( 'NONE',  ( 0.000000000000000000, -5.999999999999991118, -171.4613248654052313 ) ) ;
#9399 = CARTESIAN_POINT ( 'NONE',  ( -5.999999999999963585, 8.134310703387671600E-14, -120.8363248654052171 ) ) ;
#9400 =( BOUNDED_CURVE ( )  B_SPLINE_CURVE ( 2, ( #8538, #22533, #15650, #27258, #10877, #6230, #13197, #29581, #597 ),
 .UNSPECIFIED., .F., .T. ) 
 B_SPLINE_CURVE_WITH_KNOTS ( ( 3, 2, 2, 2, 3 ),
 ( 0.06944444444444444753, 0.07037037037037037479, 0.07222222222222221544, 0.07407407407407406996, 0.07499999999999999722 ),
 .UNSPECIFIED. ) 
 CURVE ( )  GEOMETRIC_REPRESENTATION_ITEM ( )  RATIONAL_B_SPLINE_CURVE ( ( 0.9330127018922194093, 0.9330127018922194093, 1.000000000000000000, 0.8660254037844388186, 1.000000000000000000, 0.8660254037844388186, 1.000000000000000000, 0.9330127018922194093, 0.9330127018922194093 ) ) 
 REPRESENTATION_ITEM ( '' )  );
#9401 = EDGE_CURVE ( 'NONE', #21672, #4124, #30323, .T. ) ;
#9402 = CARTESIAN_POINT ( 'NONE',  ( 145.4851497308104342, -3.535533905932725318, 3.535533905932725318 ) ) ;
#9403 = CARTESIAN_POINT ( 'NONE',  ( 112.1011751345946124, 0.8284271247463257382, -1.999999999999851674 ) ) ;
#9404 =( GEOMETRIC_REPRESENTATION_CONTEXT ( 3 ) GLOBAL_UNCERTAINTY_ASSIGNED_CONTEXT ( ( #12147 ) ) GLOBAL_UNIT_ASSIGNED_CONTEXT ( ( #28013, #30336, #16555 ) ) REPRESENTATION_CONTEXT ( 'NONE', 'WORKASPACE' ) );
#9405 = CARTESIAN_POINT ( 'NONE',  ( 5.999999999999999112, 2.951592740943527306E-14, -160.5863248654052029 ) ) ;
#9406 = CARTESIAN_POINT ( 'NONE',  ( 6.000000000000000888, -1.607695154586752384, -146.2306624327026441 ) ) ;
#9407 = CARTESIAN_POINT ( 'NONE',  ( 24.57479769840429284, -1.155887468185555544, 2.137365870997824491 ) ) ;
#9408 = CARTESIAN_POINT ( 'NONE',  ( 109.2113248654051745, -1.999999999999946265, 0.000000000000000000 ) ) ;
#9409 = CARTESIAN_POINT ( 'NONE',  ( 111.2499999999999432, -1.110223024625156540E-13, 2.500000000000057732 ) ) ;
#9410 = FACE_OUTER_BOUND ( 'NONE', #17074, .T. ) ;
#9411 = DIRECTION ( 'NONE',  ( 0.000000000000000000, 0.000000000000000000, 1.000000000000000000 ) ) ;
#9412 = SURFACE_SIDE_STYLE ('',( #11749 ) ) ;
#9413 = ORIENTED_EDGE ( 'NONE', *, *, #19386, .T. ) ;
#9414 = AXIS2_PLACEMENT_3D ( 'NONE', #15073, #26566, #466 ) ;
#9415 = CARTESIAN_POINT ( 'NONE',  ( 4.763139720814407951, 2.750000000000002665, -57.25000000000002132 ) ) ;
#9416 = CYLINDRICAL_SURFACE ( 'NONE', #4600, 6.000000000000000888 ) ;
#9417 = CARTESIAN_POINT ( 'NONE',  ( 6.000000000000000888, 7.762456499804234384E-14, -121.5863248654052455 ) ) ;
#9418 = CARTESIAN_POINT ( 'NONE',  ( -0.5000000000000004441, -14.50000000000001243, 8.500000000000007105 ) ) ;
#9419 = ORIENTED_EDGE ( 'NONE', *, *, #1575, .F. ) ;
#9420 = CARTESIAN_POINT ( 'NONE',  ( 106.8124999999997016, 1.035533905932749299, -2.499999999999784173 ) ) ;
#9421 = CARTESIAN_POINT ( 'NONE',  ( 142.0312500000000284, -2.485281374238556218, -6.000000000000005329 ) ) ;
#9422 = CARTESIAN_POINT ( 'NONE',  ( 5.412658773652712085, -3.125000000000086153, -102.0669872981078186 ) ) ;
#9423 = DIRECTION ( 'NONE',  ( -0.000000000000000000, -1.000000000000000000, 0.000000000000000000 ) ) ;
#9424 = CARTESIAN_POINT ( 'NONE',  ( 159.9226497308104058, 5.000000000000004441, 0.000000000000000000 ) ) ;
#9425 = CARTESIAN_POINT ( 'NONE',  ( 117.0624999999998579, 2.500000000000234479, 1.035533905932989551 ) ) ;
#9426 = ORIENTED_EDGE ( 'NONE', *, *, #25113, .F. ) ;
#9427 = AXIS2_PLACEMENT_3D ( 'NONE', #5261, #7426, #2810 ) ;
#9428 = EDGE_CURVE ( 'NONE', #18612, #23931, #8424, .T. ) ;
#9429 = CARTESIAN_POINT ( 'NONE',  ( -6.350852961085760029, -1.281975124255709124E-13, -139.1250000000000000 ) ) ;
#9430 = ORIENTED_EDGE ( 'NONE', *, *, #4106, .F. ) ;
#9431 = DIRECTION ( 'NONE',  ( -1.000000000000000000, -1.665334536937736783E-16, -2.220446049250315546E-16 ) ) ;
#9432 = CARTESIAN_POINT ( 'NONE',  ( 3.175426480543072749, -5.500000000000105693, -66.62500000000002842 ) ) ;
#9433 = AXIS2_PLACEMENT_3D ( 'NONE', #5854, #25057, #27504 ) ;
#9434 = B_SPLINE_CURVE_WITH_KNOTS ( 'NONE', 3,
 ( #10856, #29856, #6058, #6352 ),
 .UNSPECIFIED., .F., .F.,
 ( 4, 4 ),
 ( 0.000000000000000000, 0.0006116782145977108518 ),
 .UNSPECIFIED. ) ;
#9435 = CARTESIAN_POINT ( 'NONE',  ( -3.464101615137757051, -5.999999999999979572, -179.6636751345948255 ) ) ;
#9436 = CARTESIAN_POINT ( 'NONE',  ( 108.9761751345945697, -0.8284271247461453269, -1.999999999999791278 ) ) ;
#9437 = CARTESIAN_POINT ( 'NONE',  ( -3.608439182435115633, 6.249999999999965361, -84.30801270189222407 ) ) ;
#9438 = EDGE_CURVE ( 'NONE', #14191, #17687, #17293, .T. ) ;
#9439 = CARTESIAN_POINT ( 'NONE',  ( 5.196152422706629359, -2.999999999999988898, -100.7113248654052313 ) ) ;
#9440 = CARTESIAN_POINT ( 'NONE',  ( -5.999999999999971578, 1.607695154586715303, -139.4806624327025872 ) ) ;
#9441 = CARTESIAN_POINT ( 'NONE',  ( 106.0622167782373708, -1.849990392679441875, 0.7662911109080090544 ) ) ;
#9442 = CARTESIAN_POINT ( 'NONE',  ( 0.000000000000000000, 0.000000000000000000, -43.99152654425658682 ) ) ;
#9443 = CARTESIAN_POINT ( 'NONE',  ( 0.000000000000000000, 0.000000000000000000, 0.000000000000000000 ) ) ;
#9444 = CARTESIAN_POINT ( 'NONE',  ( 117.8127832217621744, -1.849990392679501827, 0.7662911109078287542 ) ) ;
#9445 = CARTESIAN_POINT ( 'NONE',  ( -3.175426480542816066, -5.500000000000057732, -147.8750000000000284 ) ) ;
#9446 = CARTESIAN_POINT ( 'NONE',  ( 19.22617513459487171, 2.500000000000084821, -1.035533905932929599 ) ) ;
#9447 = CARTESIAN_POINT ( 'NONE',  ( -7.216878364870328078, 0.000000000000000000, -160.5580127018922099 ) ) ;
#9448 = CARTESIAN_POINT ( 'NONE',  ( 21.99999999999998934, 10.99999999999992184, -14.99152654425661879 ) ) ;
#9449 = AXIS2_PLACEMENT_3D ( 'NONE', #15289, #4029, #13448 ) ;
#9450 = PRODUCT_DEFINITION_SHAPE ( 'NONE', 'NONE',  #30416 ) ;
#9451 = CARTESIAN_POINT ( 'NONE',  ( 0.000000000000000000, 5.499999999999991118, -82.50000000000001421 ) ) ;
#9452 = CARTESIAN_POINT ( 'NONE',  ( 19.99999999999998934, 6.500000000000061284, 4.163336342344337027E-14 ) ) ;
#9453 = CARTESIAN_POINT ( 'NONE',  ( -3.175426480542816510, -5.500000000000057732, -62.37500000000001421 ) ) ;
#9454 = CARTESIAN_POINT ( 'NONE',  ( 5.999999999999988454, 1.607695154586737729, -155.0966878364871206 ) ) ;
#9455 = CARTESIAN_POINT ( 'NONE',  ( 6.000000000000000888, 1.743066579297358182E-13, -87.66367513459482552 ) ) ;
#9456 = CARTESIAN_POINT ( 'NONE',  ( 141.0000000000000284, -54.99999999999989342, -5.000000000000004441 ) ) ;
#9457 = CARTESIAN_POINT ( 'NONE',  ( 156.6562500000000284, -6.000000000000005329, 2.485281374238556218 ) ) ;
#9458 = CARTESIAN_POINT ( 'NONE',  ( 16.75000000000015277, 1.665334536937734811E-13, -2.000000000000001776 ) ) ;
#9459 = CARTESIAN_POINT ( 'NONE',  ( -5.999999999999956479, -1.607695154586745057, -50.26933756729746250 ) ) ;
#9460 = CARTESIAN_POINT ( 'NONE',  ( -4.999999999999990230, -55.00000000000002132, -5.000000000000004441 ) ) ;
#9461 = CARTESIAN_POINT ( 'NONE',  ( 117.3122167782375840, -0.7662911109077388261, -1.849990392679351725 ) ) ;
#9462 = DIRECTION ( 'NONE',  ( 0.000000000000000000, 0.000000000000000000, -1.000000000000000000 ) ) ;
#9463 = EDGE_LOOP ( 'NONE', ( #2683, #13497, #18665, #15176 ) ) ;
#9464 = CARTESIAN_POINT ( 'NONE',  ( 151.7812500000000284, 2.485281374238585972, 6.000000000000005329 ) ) ;
#9465 = SURFACE_STYLE_USAGE ( .BOTH. , #80 ) ;
#9466 = EDGE_CURVE ( 'NONE', #1664, #9581, #20665, .T. ) ;
#9467 = CYLINDRICAL_SURFACE ( 'NONE', #21020, 5.500000000000000000 ) ;
#9468 = ORIENTED_EDGE ( 'NONE', *, *, #16847, .T. ) ;
#9469 = ORIENTED_EDGE ( 'NONE', *, *, #1936, .T. ) ;
#9470 = CARTESIAN_POINT ( 'NONE',  ( 21.00000000000007461, 2.000000000000057288, 0.000000000000000000 ) ) ;
#9471 = EDGE_LOOP ( 'NONE', ( #27486, #27717 ) ) ;
#9472 = CARTESIAN_POINT ( 'NONE',  ( -6.350852961085760029, -1.281975124255709124E-13, -92.62500000000001421 ) ) ;
#9473 = ADVANCED_FACE ( 'NONE', ( #27390 ), #14284, .F. ) ;
#9474 = CARTESIAN_POINT ( 'NONE',  ( 5.412658773652712085, -3.125000000000086153, -110.4330127018922099 ) ) ;
#9475 = ORIENTED_EDGE ( 'NONE', *, *, #11589, .T. ) ;
#9476 = CARTESIAN_POINT ( 'NONE',  ( 5.196152422706629359, 3.000000000000002665, -68.03867513459482552 ) ) ;
#9477 = CARTESIAN_POINT ( 'NONE',  ( 157.4851497308104058, -3.535533905932725318, 3.535533905932725318 ) ) ;
#9478 = B_SPLINE_CURVE_WITH_KNOTS ( 'NONE', 3,
 ( #19711, #14320, #18608, #11561, #147, #4749, #9217, #1997, #23660, #6904, #2595, #23365, #5035, #11868, #21207, #9676 ),
 .UNSPECIFIED., .F., .F.,
 ( 4, 2, 2, 2, 2, 2, 2, 4 ),
 ( 0.000000000000000000, 0.0007767943629862210809, 0.001165191544479369894, 0.001553588725972518706, 0.001941985907465667736, 0.002330383088958817416, 0.002718780270451967313, 0.003107177451945116776 ),
 .UNSPECIFIED. ) ;
#9479 = CARTESIAN_POINT ( 'NONE',  ( -4.763139720814407951, -2.750000000000016431, -166.0000000000000284 ) ) ;
#9480 = CARTESIAN_POINT ( 'NONE',  ( -3.464101615137757051, -5.999999999999979572, -106.1636751345948539 ) ) ;
#9481 = CARTESIAN_POINT ( 'NONE',  ( 135.0000000000000284, -7.549834435270740940, 7.500000000000007105 ) ) ;
#9482 = CARTESIAN_POINT ( 'NONE',  ( 6.000000000000000888, -1.859271017917181981E-14, -67.58632486540523132 ) ) ;
#9483 = CARTESIAN_POINT ( 'NONE',  ( -6.350852961085760029, -1.281975124255709124E-13, -169.1249999999999716 ) ) ;
#9484 = CARTESIAN_POINT ( 'NONE',  ( 135.0863248654052313, 0.000000000000000000, 5.500000000000005329 ) ) ;
#9485 = CARTESIAN_POINT ( 'NONE',  ( -6.350852961085760029, -1.281975124255709124E-13, -151.1250000000000568 ) ) ;
#9486 = CARTESIAN_POINT ( 'NONE',  ( 111.3749999999999289, -1.767766952966320915, 1.767766952966431937 ) ) ;
#9487 = CARTESIAN_POINT ( 'NONE',  ( 3.175426480543072749, -5.500000000000105693, -101.1249999999999858 ) ) ;
#9488 = CARTESIAN_POINT ( 'NONE',  ( -5.196152422706573404, -3.000000000000002665, -159.7113248654052313 ) ) ;
#9489 = DIRECTION ( 'NONE',  ( 0.000000000000000000, 0.000000000000000000, 1.000000000000000000 ) ) ;
#9490 =( BOUNDED_CURVE ( )  B_SPLINE_CURVE ( 2, ( #22282, #1072, #18004, #8279, #14924 ),
 .UNSPECIFIED., .F., .F. ) 
 B_SPLINE_CURVE_WITH_KNOTS ( ( 3, 2, 3 ),
 ( 0.000000000000000000, 0.001851851851851882280, 0.002777777777777768343 ),
 .UNSPECIFIED. ) 
 CURVE ( )  GEOMETRIC_REPRESENTATION_ITEM ( )  RATIONAL_B_SPLINE_CURVE ( ( 1.000000000000000000, 0.8660254037844388186, 1.000000000000000000, 0.9330127018922194093, 0.9330127018922194093 ) ) 
 REPRESENTATION_ITEM ( '' )  );
#9492 = CARTESIAN_POINT ( 'NONE',  ( 0.000000000000000000, 5.499999999999991118, -88.50000000000002842 ) ) ;
#9491 = CARTESIAN_POINT ( 'NONE',  ( -6.350852961085760029, -1.281975124255709124E-13, -157.1250000000000284 ) ) ;
#9493 = CARTESIAN_POINT ( 'NONE',  ( 160.3273502691896510, -5.000000000000004441, 0.000000000000000000 ) ) ;
#9494 = CARTESIAN_POINT ( 'NONE',  ( 12.53867513459494631, 1.110223024625156540E-13, 2.500000000000002220 ) ) ;
#9495 = VERTEX_POINT ( 'NONE', #25094 ) ;
#9496 = CARTESIAN_POINT ( 'NONE',  ( 9.187500000000126121, -2.649519052838178457, -1.097466725451559322 ) ) ;
#9497 = APPLICATION_CONTEXT ( 'automotive_design' ) ;
#9498 = DIRECTION ( 'NONE',  ( 0.000000000000000000, 0.000000000000000000, 1.000000000000000000 ) ) ;
#9499 = CARTESIAN_POINT ( 'NONE',  ( 105.3752832217622739, 1.849990392679523588, 0.000000000000000000 ) ) ;
#9500 = CARTESIAN_POINT ( 'NONE',  ( 157.8824251345948539, 5.500000000000012434, 2.278174593052012309 ) ) ;
#9501 =( BOUNDED_CURVE ( )  B_SPLINE_CURVE ( 2, ( #25244, #20671, #8995, #30024, #27699, #24650, #3597, #15795, #1457 ),
 .UNSPECIFIED., .F., .T. ) 
 B_SPLINE_CURVE_WITH_KNOTS ( ( 3, 2, 2, 2, 3 ),
 ( 0.7916666666666666297, 0.7925925925925926263, 0.7944444444444443976, 0.7962962962962962798, 0.7972222222222222765 ),
 .UNSPECIFIED. ) 
 CURVE ( )  GEOMETRIC_REPRESENTATION_ITEM ( )  RATIONAL_B_SPLINE_CURVE ( ( 0.9330127018922194093, 0.9330127018922154125, 1.000000000000000000, 0.8660254037844388186, 1.000000000000000000, 0.8660254037844388186, 1.000000000000000000, 0.9330127018922154125, 0.9330127018922194093 ) ) 
 REPRESENTATION_ITEM ( '' )  );
#9502 = ORIENTED_EDGE ( 'NONE', *, *, #15131, .F. ) ;
#9503 = CARTESIAN_POINT ( 'NONE',  ( 10.00000000000009237, 2.000000000000112799, 0.000000000000000000 ) ) ;
#9504 = DIRECTION ( 'NONE',  ( -7.147005652999508048E-36, 5.642372883946980038E-36, 1.000000000000000000 ) ) ;
#9505 = EDGE_CURVE ( 'NONE', #25491, #21560, #4051, .T. ) ;
#9506 = CARTESIAN_POINT ( 'NONE',  ( -9.999999999999793943, 9.000000000000007105, 4.000000000000003553 ) ) ;
#9507 = ORIENTED_EDGE ( 'NONE', *, *, #15099, .F. ) ;
#9508 = CARTESIAN_POINT ( 'NONE',  ( 6.000000000000052403, -1.607695154586662678, -52.65331216351295041 ) ) ;
#9509 = AXIS2_PLACEMENT_3D ( 'NONE', #3631, #13068, #22399 ) ;
#9510 = CARTESIAN_POINT ( 'NONE',  ( 152.8125000000000568, 4.242640687119298093, -4.242640687119298093 ) ) ;
#9511 = VERTEX_POINT ( 'NONE', #25558 ) ;
#9512 = CARTESIAN_POINT ( 'NONE',  ( 3.175426480543072749, 5.499999999999865885, -114.1249999999999858 ) ) ;
#9513 = CARTESIAN_POINT ( 'NONE',  ( 24.12500000000009237, 1.665334536937734811E-13, -2.649519052838333888 ) ) ;
#9514 = EDGE_CURVE ( 'NONE', #26264, #7192, #29859, .T. ) ;
#9515 = CARTESIAN_POINT ( 'NONE',  ( 2.775557561562891351E-14, -6.250000000000061284, -130.1830127018922667 ) ) ;
#9516 = ORIENTED_EDGE ( 'NONE', *, *, #8222, .T. ) ;
#9517 = CARTESIAN_POINT ( 'NONE',  ( 0.000000000000000000, 0.000000000000000000, 0.000000000000000000 ) ) ;
#9518 = CARTESIAN_POINT ( 'NONE',  ( 5.412658773652712085, -3.125000000000086153, -168.0669872981078186 ) ) ;
#9519 = CARTESIAN_POINT ( 'NONE',  ( 108.8749999999999574, 1.767766952966265404, -1.767766952966320915 ) ) ;
#9520 = CARTESIAN_POINT ( 'NONE',  ( 133.2038997308104342, 2.071067811865468400, 4.999999999999989342 ) ) ;
#9521 = ORIENTED_EDGE ( 'NONE', *, *, #7201, .T. ) ;
#9522 = DIRECTION ( 'NONE',  ( -0.000000000000000000, -0.000000000000000000, -1.000000000000000000 ) ) ;
#9523 = CARTESIAN_POINT ( 'NONE',  ( -3.464101615137725076, 5.999999999999979572, -136.6636751345948539 ) ) ;
#9524 = CARTESIAN_POINT ( 'NONE',  ( 4.763139720814407951, 2.750000000000002665, -177.2500000000000284 ) ) ;
#9525 = CARTESIAN_POINT ( 'NONE',  ( 107.8752832217621602, -1.849990392679329299, 3.330669073875469621E-13 ) ) ;
#9526 = CARTESIAN_POINT ( 'NONE',  ( 2.775557561562891351E-14, 6.250000000000033751, -175.9330127018922099 ) ) ;
#9527 = CARTESIAN_POINT ( 'NONE',  ( -0.9345383689551295392, -9.130923262089551073, -4.000000000000005329 ) ) ;
#9528 = CARTESIAN_POINT ( 'NONE',  ( -3.464101615137725076, 5.999999999999979572, -123.1636751345947971 ) ) ;
#9529 = CARTESIAN_POINT ( 'NONE',  ( 6.350852961086080661, -9.614813431917819062E-14, -112.8750000000000568 ) ) ;
#9530 = CARTESIAN_POINT ( 'NONE',  ( -3.464101615137725076, 5.999999999999979572, -145.6636751345947687 ) ) ;
#9531 = ORIENTED_EDGE ( 'NONE', *, *, #25322, .F. ) ;
#9532 = CARTESIAN_POINT ( 'NONE',  ( 20.18750000000012079, -2.649519052838178457, -1.097466725451499370 ) ) ;
#9533 = FACE_OUTER_BOUND ( 'NONE', #25999, .T. ) ;
#9534 = CARTESIAN_POINT ( 'NONE',  ( -1.000000000000000888, -9.000000000000007105, -4.000000000000003553 ) ) ;
#9535 = CARTESIAN_POINT ( 'NONE',  ( -0.04562205425674009662, -14.50000000000001243, 8.291335958003937634 ) ) ;
#9536 = ORIENTED_EDGE ( 'NONE', *, *, #23492, .F. ) ;
#9537 = CARTESIAN_POINT ( 'NONE',  ( 129.9999999999998010, -89.00000000000001421, -4.000000000000003553 ) ) ;
#9538 = EDGE_CURVE ( 'NONE', #3881, #4074, #11925, .T. ) ;
#9539 = CARTESIAN_POINT ( 'NONE',  ( 3.464101615137757051, -5.999999999999979572, -176.4136751345947403 ) ) ;
#9540 = CARTESIAN_POINT ( 'NONE',  ( 0.000000000000000000, -5.999999999999991118, -125.5386751345948255 ) ) ;
#9541 = ADVANCED_FACE ( 'NONE', ( #27692 ), #19183, .F. ) ;
#9542 = PRODUCT_RELATED_PRODUCT_CATEGORY ( 'part', '', ( #10914 ) ) ;
#9543 = LINE ( 'NONE', #7378, #14301 ) ;
#9544 = ORIENTED_EDGE ( 'NONE', *, *, #2523, .F. ) ;
#9545 = EDGE_LOOP ( 'NONE', ( #4319, #25213, #27559, #2757 ) ) ;
#9546 = CARTESIAN_POINT ( 'NONE',  ( 152.2425748654052029, -2.278174593052229469, -5.499999999999796607 ) ) ;
#9547 = CARTESIAN_POINT ( 'NONE',  ( 135.4687500000000853, -2.485281374238585972, 6.000000000000005329 ) ) ;
#9548 = ORIENTED_EDGE ( 'NONE', *, *, #3918, .F. ) ;
#9549 = CARTESIAN_POINT ( 'NONE',  ( 5.412658773652739619, 3.124999999999988898, -136.3169872981078186 ) ) ;
#9550 = CARTESIAN_POINT ( 'NONE',  ( 6.000000000000000888, -3.330669073875464691E-16, -7.560779664488942560E-35 ) ) ;
#9551 = CARTESIAN_POINT ( 'NONE',  ( 10.12500000000002309, 1.110223024625156540E-13, -2.649519052838333888 ) ) ;
#9552 = CARTESIAN_POINT ( 'NONE',  ( -6.000000000000007105, -1.607695154586655129, -93.76933756729741276 ) ) ;
#9553 = CARTESIAN_POINT ( 'NONE',  ( 19.18750000000004263, 0.8284271247462955401, 2.000000000000031530 ) ) ;
#9554 = FACE_OUTER_BOUND ( 'NONE', #6038, .T. ) ;
#9555 = CARTESIAN_POINT ( 'NONE',  ( 6.000000000000000888, -1.859271017917181981E-14, -137.1636751345948255 ) ) ;
#9556 = DIRECTION ( 'NONE',  ( -7.147005652999508048E-36, 5.642372883946980038E-36, 1.000000000000000000 ) ) ;
#9557 = CARTESIAN_POINT ( 'NONE',  ( 142.9538997308104058, -2.071067811865468400, -4.999999999999989342 ) ) ;
#9558 = CARTESIAN_POINT ( 'NONE',  ( -5.999999999999963585, -1.487416814333745711E-14, -101.9136751345948397 ) ) ;
#9559 = CARTESIAN_POINT ( 'NONE',  ( 5.999999999999949374, 1.607695154586804565, -74.09668783648706381 ) ) ;
#9560 = CARTESIAN_POINT ( 'NONE',  ( -3.330669073875475045E-16, 6.000000000000005329, 6.063858597689169383E-15 ) ) ;
#9561 = CARTESIAN_POINT ( 'NONE',  ( -6.000000000000007105, -1.607695154586655129, -69.76933756729741276 ) ) ;
#9562 = CARTESIAN_POINT ( 'NONE',  ( 109.5624999999997016, -2.499999999999994671, -1.035533905932508825 ) ) ;
#9563 = CARTESIAN_POINT ( 'NONE',  ( 115.1636751345947545, 1.414213562373145550, -1.414213562372812483 ) ) ;
#9564 = CARTESIAN_POINT ( 'NONE',  ( -5.999999999999962697, 3.323446944526963891E-14, -148.4136751345948255 ) ) ;
#9565 = ORIENTED_EDGE ( 'NONE', *, *, #28445, .F. ) ;
#9566 = CARTESIAN_POINT ( 'NONE',  ( 6.350852961086080661, -9.614813431917819062E-14, -55.87500000000003553 ) ) ;
#9567 = CARTESIAN_POINT ( 'NONE',  ( -5.196152422706573404, -3.000000000000002665, -133.2886751345948539 ) ) ;
#9568 = CARTESIAN_POINT ( 'NONE',  ( -5.999999999999919176, 1.607695154586804565, -62.40331216351300725 ) ) ;
#9569 = DIRECTION ( 'NONE',  ( -7.147005652999508048E-36, 5.642372883946980038E-36, 1.000000000000000000 ) ) ;
#9570 = ORIENTED_EDGE ( 'NONE', *, *, #7172, .T. ) ;
#9571 = CARTESIAN_POINT ( 'NONE',  ( 117.7497167782374987, 1.308140751793723799, 1.308140751793640533 ) ) ;
#9572 = CARTESIAN_POINT ( 'NONE',  ( 140.0625000000000284, -4.242640687119298093, 4.242640687119298093 ) ) ;
#9573 = CARTESIAN_POINT ( 'NONE',  ( 12.37500000000013500, -1.414213562372979016, 1.414213562373034527 ) ) ;
#9574 = CARTESIAN_POINT ( 'NONE',  ( 5.412658773652739619, 3.124999999999988898, -101.8169872981078470 ) ) ;
#9575 = CARTESIAN_POINT ( 'NONE',  ( 138.1800748654051745, -2.278174593051950136, 5.500000000000074607 ) ) ;
#9576 = ADVANCED_FACE ( 'NONE', ( #28154 ), #23727, .F. ) ;
#9577 = CARTESIAN_POINT ( 'NONE',  ( 135.3750000000000284, 0.000000000000000000, 6.000000000000005329 ) ) ;
#9578 = CARTESIAN_POINT ( 'NONE',  ( 119.1874999999998010, 1.035533905932779275, 2.500000000000205169 ) ) ;
#9579 = CARTESIAN_POINT ( 'NONE',  ( -3.175426480542816510, -5.500000000000057732, -128.3750000000000000 ) ) ;
#9580 =( BOUNDED_CURVE ( )  B_SPLINE_CURVE ( 2, ( #3564, #1426, #8497, #17903, #12995, #25072, #24923, #10512, #22493 ),
 .UNSPECIFIED., .F., .T. ) 
 B_SPLINE_CURVE_WITH_KNOTS ( ( 3, 2, 2, 2, 3 ),
 ( 0.4694444444444444420, 0.4703703703703703831, 0.4722222222222222099, 0.4740740740740740922, 0.4750000000000000333 ),
 .UNSPECIFIED. ) 
 CURVE ( )  GEOMETRIC_REPRESENTATION_ITEM ( )  RATIONAL_B_SPLINE_CURVE ( ( 0.9330127018922194093, 0.9330127018922194093, 1.000000000000000000, 0.8660254037844388186, 1.000000000000000000, 0.8660254037844388186, 1.000000000000000000, 0.9330127018922174109, 0.9330127018922194093 ) ) 
 REPRESENTATION_ITEM ( '' )  );
#9581 = VERTEX_POINT ( 'NONE', #14668 ) ;
#9582 = VERTEX_POINT ( 'NONE', #7565 ) ;
#9583 = CARTESIAN_POINT ( 'NONE',  ( 5.999999999999999112, 2.951592740943527306E-14, -163.5863248654052313 ) ) ;
#9584 = AXIS2_PLACEMENT_3D ( 'NONE', #15332, #13189, #20224 ) ;
#9585 = CARTESIAN_POINT ( 'NONE',  ( -2.775557561562891351E-14, -5.500000000000115463, -66.75000000000002842 ) ) ;
#9586 = CARTESIAN_POINT ( 'NONE',  ( -3.464101615137725076, 5.999999999999979572, -115.6636751345948255 ) ) ;
#9587 = CARTESIAN_POINT ( 'NONE',  ( 159.8823591035255731, -12.38010379384060933, -3.486960716177708974 ) ) ;
#9588 = CARTESIAN_POINT ( 'NONE',  ( -7.216878364870328078, 0.000000000000000000, -79.55801270189225249 ) ) ;
#9589 = CARTESIAN_POINT ( 'NONE',  ( 0.000000000000000000, -5.999999999999991118, -113.5386751345948113 ) ) ;
#9590 = CARTESIAN_POINT ( 'NONE',  ( 104.4997167782375413, 1.308140751793668288, -1.308140751793640533 ) ) ;
#9591 = DIRECTION ( 'NONE',  ( 1.000000000000000000, -0.000000000000000000, -0.000000000000000000 ) ) ;
#9592 = CARTESIAN_POINT ( 'NONE',  ( 135.8363248654052029, 0.000000000000000000, -5.500000000000005329 ) ) ;
#9593 = CARTESIAN_POINT ( 'NONE',  ( 118.0627832217622455, -0.7662911109076485650, -1.849990392679171425 ) ) ;
#9594 = CARTESIAN_POINT ( 'NONE',  ( 4.763139720814407951, 2.750000000000002665, -139.7500000000000284 ) ) ;
#9595 = CARTESIAN_POINT ( 'NONE',  ( -3.464101615137757051, -5.999999999999979572, -105.5863248654052171 ) ) ;
#9596 = AXIS2_PLACEMENT_3D ( 'NONE', #11575, #20921, #27797 ) ;
#9597 = CARTESIAN_POINT ( 'NONE',  ( 5.412658773652739619, 3.124999999999988898, -155.1830127018922667 ) ) ;
#9598 = EDGE_CURVE ( 'NONE', #9799, #28361, #25096, .T. ) ;
#9599 = CARTESIAN_POINT ( 'NONE',  ( 3.175426480543072749, 5.499999999999865885, -82.62500000000004263 ) ) ;
#9600 = CARTESIAN_POINT ( 'NONE',  ( 5.999999999999949374, 1.607695154586804565, -174.0193375672974412 ) ) ;
#9601 = CARTESIAN_POINT ( 'NONE',  ( 4.763139720814407951, 2.750000000000002665, -61.75000000000002842 ) ) ;
#9602 = FILL_AREA_STYLE_COLOUR ( '', #10918 ) ;
#9603 = CARTESIAN_POINT ( 'NONE',  ( 142.9836002691896510, 4.999999999999989342, -2.071067811865468400 ) ) ;
#9604 = CARTESIAN_POINT ( 'NONE',  ( -5.999999999999962697, 3.323446944526963891E-14, -148.4136751345948255 ) ) ;
#9605 = CARTESIAN_POINT ( 'NONE',  ( 156.1875000000000284, 4.242640687119269671, 4.242640687119298093 ) ) ;
#9606 = CARTESIAN_POINT ( 'NONE',  ( 16.50000000000004263, -1.999999999999835243, 0.000000000000000000 ) ) ;
#9607 = CIRCLE ( 'NONE', #13564, 16.00000000000000000 ) ;
#9608 = LINE ( 'NONE', #16703, #27802 ) ;
#9609 = CARTESIAN_POINT ( 'NONE',  ( 117.4997167782374987, 1.308140751793696044, -1.308140751793640533 ) ) ;
#9610 = DIRECTION ( 'NONE',  ( 1.000000000000000000, -5.551115123125773458E-17, -1.260129944081490338E-35 ) ) ;
#9611 = ADVANCED_FACE ( 'NONE', ( #16546 ), #12235, .F. ) ;
#9612 = ORIENTED_EDGE ( 'NONE', *, *, #26937, .T. ) ;
#9613 = CARTESIAN_POINT ( 'NONE',  ( 147.1875000000000284, 4.242640687119269671, 4.242640687119298093 ) ) ;
#9614 = CARTESIAN_POINT ( 'NONE',  ( 140.0000000000000284, -11.45643923738959202, 5.000000000000004441 ) ) ;
#9615 = ORIENTED_EDGE ( 'NONE', *, *, #30294, .F. ) ;
#9616 = CARTESIAN_POINT ( 'NONE',  ( 22.81250000000002487, 0.8284271247461753029, -2.000000000000091926 ) ) ;
#9617 = VERTEX_POINT ( 'NONE', #14391 ) ;
#9618 = CARTESIAN_POINT ( 'NONE',  ( 3.175426480543072749, 5.499999999999865885, -93.12500000000002842 ) ) ;
#9619 = CARTESIAN_POINT ( 'NONE',  ( 15.93750000000014921, -2.649519052838238409, -1.097466725451559322 ) ) ;
#9620 = CARTESIAN_POINT ( 'NONE',  ( -3.608439182435052128, -6.250000000000110134, -100.3080127018922241 ) ) ;
#9621 = ORIENTED_EDGE ( 'NONE', *, *, #24746, .F. ) ;
#9622 = CARTESIAN_POINT ( 'NONE',  ( 154.0163997308104342, 4.999999999999989342, 2.071067811865468400 ) ) ;
#9623 = VECTOR ( 'NONE', #20326, 1000.000000000000000 ) ;
#9624 =( BOUNDED_CURVE ( )  B_SPLINE_CURVE ( 3, ( #25118, #30201, #23160, #6241 ),
 .UNSPECIFIED., .F., .F. ) 
 B_SPLINE_CURVE_WITH_KNOTS ( ( 4, 4 ),
 ( 3.141592653589793116, 4.712388980384689674 ),
 .UNSPECIFIED. ) 
 CURVE ( )  GEOMETRIC_REPRESENTATION_ITEM ( )  RATIONAL_B_SPLINE_CURVE ( ( 1.000000000000000000, 0.8047378541243649375, 0.8047378541243649375, 1.000000000000000000 ) ) 
 REPRESENTATION_ITEM ( '' )  );
#9625 = CARTESIAN_POINT ( 'NONE',  ( 0.000000000000000000, 0.000000000000000000, 0.000000000000000000 ) ) ;
#9626 = CARTESIAN_POINT ( 'NONE',  ( 0.000000000000000000, -5.999999999999991118, -67.96132486540523132 ) ) ;
#9627 = PRESENTATION_STYLE_ASSIGNMENT (( #14133 ) ) ;
#9628 = CARTESIAN_POINT ( 'NONE',  ( -2.775557561562891351E-14, -5.500000000000115463, -173.2500000000000284 ) ) ;
#9629 = CARTESIAN_POINT ( 'NONE',  ( 160.4136751345948824, 0.000000000000000000, -5.500000000000005329 ) ) ;
#9630 = CARTESIAN_POINT ( 'NONE',  ( 3.175426480543072749, -5.500000000000105693, -158.1250000000000284 ) ) ;
#9631 = CARTESIAN_POINT ( 'NONE',  ( 111.1874999999999858, 1.035533905932749299, 2.500000000000265121 ) ) ;
#9632 = CARTESIAN_POINT ( 'NONE',  ( -6.000000000000007105, -1.607695154586655129, -104.2693375672974128 ) ) ;
#9633 = EDGE_CURVE ( 'NONE', #20687, #11659, #21575, .T. ) ;
#9634 = CARTESIAN_POINT ( 'NONE',  ( -4.763139720814407951, -2.750000000000016431, -104.5000000000000426 ) ) ;
#9635 = SURFACE_STYLE_FILL_AREA ( #18569 ) ;
#9636 = CARTESIAN_POINT ( 'NONE',  ( 145.3199251345948539, -2.278174593052027408, -5.499999999999996447 ) ) ;
#9638 = CARTESIAN_POINT ( 'NONE',  ( -4.763139720814407951, -2.750000000000016431, -86.50000000000002842 ) ) ;
#9637 = CARTESIAN_POINT ( 'NONE',  ( 4.763139720814407951, -2.749999999999988454, -155.0000000000000284 ) ) ;
#9639 = CARTESIAN_POINT ( 'NONE',  ( 13.77382486540532014, 2.500000000000084821, 1.035533905932689347 ) ) ;
#9640 = DIRECTION ( 'NONE',  ( -7.147005652999508048E-36, 5.642372883946980038E-36, 1.000000000000000000 ) ) ;
#9641 = EDGE_LOOP ( 'NONE', ( #25227, #11847, #3577, #17335 ) ) ;
#9642 = CARTESIAN_POINT ( 'NONE',  ( 24.12500000000009237, 1.414213562373201061, 1.414213562373034527 ) ) ;
#9643 = UNCERTAINTY_MEASURE_WITH_UNIT (LENGTH_MEASURE( 1.000000000000000082E-05 ), #14009, 'distance_accuracy_value', 'NONE');
#9644 = CARTESIAN_POINT ( 'NONE',  ( 113.4999999999999147, -2.499999999999919176, 0.000000000000000000 ) ) ;
#9645 = CARTESIAN_POINT ( 'NONE',  ( 112.2113248654051176, -1.999999999999946265, 0.000000000000000000 ) ) ;
#9646 = CARTESIAN_POINT ( 'NONE',  ( 108.2502832217622029, 1.308140751793640533, -1.308140751793640533 ) ) ;
#9647 = EDGE_CURVE ( 'NONE', #448, #30239, #11120, .T. ) ;
#9648 = CARTESIAN_POINT ( 'NONE',  ( -3.464101615137725076, 5.999999999999979572, -78.16367513459485394 ) ) ;
#9649 = AXIS2_PLACEMENT_3D ( 'NONE', #18071, #3426, #3888 ) ;
#9650 = EDGE_CURVE ( 'NONE', #2096, #23551, #25633, .T. ) ;
#9651 = VERTEX_POINT ( 'NONE', #22481 ) ;
#9652 = FACE_OUTER_BOUND ( 'NONE', #5809, .T. ) ;
#9653 = ORIENTED_EDGE ( 'NONE', *, *, #27468, .T. ) ;
#9654 = ORIENTED_EDGE ( 'NONE', *, *, #23025, .F. ) ;
#9655 = CARTESIAN_POINT ( 'NONE',  ( 153.0000000000000284, 6.000000000000005329, 0.000000000000000000 ) ) ;
#9656 = ORIENTED_EDGE ( 'NONE', *, *, #9674, .T. ) ;
#9657 = CARTESIAN_POINT ( 'NONE',  ( 4.763139720814407951, 2.750000000000002665, -109.7500000000000142 ) ) ;
#9658 =( GEOMETRIC_REPRESENTATION_CONTEXT ( 3 ) GLOBAL_UNCERTAINTY_ASSIGNED_CONTEXT ( ( #19291 ) ) GLOBAL_UNIT_ASSIGNED_CONTEXT ( ( #16842, #10509, #10211 ) ) REPRESENTATION_CONTEXT ( 'NONE', 'WORKASPACE' ) );
#9659 = CARTESIAN_POINT ( 'NONE',  ( 18.93750000000008171, -2.649519052838238409, -1.097466725451379244 ) ) ;
#9660 = CARTESIAN_POINT ( 'NONE',  ( -3.608439182435052128, -6.250000000000110134, -124.3080127018922099 ) ) ;
#9661 = UNCERTAINTY_MEASURE_WITH_UNIT (LENGTH_MEASURE( 1.000000000000000082E-05 ), #29131, 'distance_accuracy_value', 'NONE');
#9662 = ORIENTED_EDGE ( 'NONE', *, *, #23072, .T. ) ;
#9663 = CARTESIAN_POINT ( 'NONE',  ( -7.216878364870328078, 0.000000000000000000, -165.6919872981078186 ) ) ;
#9664 = CARTESIAN_POINT ( 'NONE',  ( 106.4999999999999147, -2.499999999999946709, 1.110223024625156540E-13 ) ) ;
#9665 = COLOUR_RGB ( '', 0.72549020, 0.75294118, 0.79215686) ;
#9666 = ORIENTED_EDGE ( 'NONE', *, *, #22445, .T. ) ;
#9667 =( BOUNDED_CURVE ( )  B_SPLINE_CURVE ( 2, ( #3073, #12497, #22598, #24731, #1380, #13258, #13107, #1531, #25024 ),
 .UNSPECIFIED., .F., .T. ) 
 B_SPLINE_CURVE_WITH_KNOTS ( ( 3, 2, 2, 2, 3 ),
 ( 0.9305555555555555802, 0.9314814814814814659, 0.9333333333333333481, 0.9351851851851852304, 0.9361111111111111160 ),
 .UNSPECIFIED. ) 
 CURVE ( )  GEOMETRIC_REPRESENTATION_ITEM ( )  RATIONAL_B_SPLINE_CURVE ( ( 0.9330127018922194093, 0.9330127018922234061, 1.000000000000000000, 0.8660254037844388186, 1.000000000000000000, 0.8660254037844388186, 1.000000000000000000, 0.9330127018922194093, 0.9330127018922194093 ) ) 
 REPRESENTATION_ITEM ( '' )  );
#9668 = CARTESIAN_POINT ( 'NONE',  ( -4.871333033796909184, 9.863307416503793945, -21.49176472276548111 ) ) ;
#9669 = DIRECTION ( 'NONE',  ( -0.000000000000000000, -0.000000000000000000, -1.000000000000000000 ) ) ;
#9670 = CARTESIAN_POINT ( 'NONE',  ( -2.775557561562891351E-14, -5.500000000000115463, -176.2500000000000284 ) ) ;
#9671 = CARTESIAN_POINT ( 'NONE',  ( 107.8127832217621318, -1.849990392679472073, 0.7662911109079489913 ) ) ;
#9672 = CARTESIAN_POINT ( 'NONE',  ( 7.216878364870455975, -6.409875621278545621E-14, -173.3080127018922667 ) ) ;
#9673 = CARTESIAN_POINT ( 'NONE',  ( -5.999999999999971578, 1.607695154586715303, -75.90331216351297883 ) ) ;
#9674 = EDGE_CURVE ( 'NONE', #6464, #9159, #13715, .T. ) ;
#9675 = CARTESIAN_POINT ( 'NONE',  ( -3.464101615137757051, -5.999999999999979572, -101.6636751345948255 ) ) ;
#9676 = CARTESIAN_POINT ( 'NONE',  ( 161.0000000000000284, -11.67610212985248452, -2.769230769230773603 ) ) ;
#9677 = UNCERTAINTY_MEASURE_WITH_UNIT (LENGTH_MEASURE( 1.000000000000000082E-05 ), #14808, 'distance_accuracy_value', 'NONE');
#9678 = CARTESIAN_POINT ( 'NONE',  ( -4.763139720814407951, 2.749999999999946709, -110.7500000000000142 ) ) ;
#9679 =( BOUNDED_CURVE ( )  B_SPLINE_CURVE ( 2, ( #25328, #9378, #4755, #28090, #4603, #27630, #20910, #20438, #13879 ),
 .UNSPECIFIED., .F., .T. ) 
 B_SPLINE_CURVE_WITH_KNOTS ( ( 3, 2, 2, 2, 3 ),
 ( 0.3624999999999989342, 0.3687499999999991895, 0.3749999999999994449, 0.3812499999999996447, 0.3874999999999999001 ),
 .UNSPECIFIED. ) 
 CURVE ( )  GEOMETRIC_REPRESENTATION_ITEM ( )  RATIONAL_B_SPLINE_CURVE ( ( 1.000000000000013545, 0.9238795325112731938, 1.000000000000000000, 0.9238795325112867385, 1.000000000000000000, 0.9238795325112867385, 1.000000000000000000, 0.9238795325112874046, 0.9999999999999993339 ) ) 
 REPRESENTATION_ITEM ( '' )  );
#9680 = CARTESIAN_POINT ( 'NONE',  ( -5.196152422706601826, 2.999999999999975131, -165.9613248654052029 ) ) ;
#9681 = CARTESIAN_POINT ( 'NONE',  ( 3.464101615137852974, 5.999999999999884537, -88.91367513459483973 ) ) ;
#9682 = ORIENTED_EDGE ( 'NONE', *, *, #19452, .F. ) ;
#9683 = CARTESIAN_POINT ( 'NONE',  ( 17.25000000000015277, -1.873492889144845464, -1.873492889145123019 ) ) ;
#9684 = LINE ( 'NONE', #21059, #26069 ) ;
#9685 = CARTESIAN_POINT ( 'NONE',  ( 6.000000000000000888, -1.859271017917181981E-14, -168.6636751345947971 ) ) ;
#9686 = AXIS2_PLACEMENT_3D ( 'NONE', #14831, #24175, #28914 ) ;
#9687 = AXIS2_PLACEMENT_3D ( 'NONE', #1083, #10475, #17399 ) ;
#9688 = EDGE_CURVE ( 'NONE', #10444, #28521, #29056, .T. ) ;
#9689 = EDGE_CURVE ( 'NONE', #27181, #566, #17402, .T. ) ;
#9690 = ORIENTED_EDGE ( 'NONE', *, *, #2161, .F. ) ;
#9691 = DIRECTION ( 'NONE',  ( 1.000000000000000000, 0.000000000000000000, 0.000000000000000000 ) ) ;
#9692 = CARTESIAN_POINT ( 'NONE',  ( -5.999999999999963585, -1.487416814333745711E-14, -127.4136751345948113 ) ) ;
#9693 = FACE_OUTER_BOUND ( 'NONE', #22563, .T. ) ;
#9694 = CARTESIAN_POINT ( 'NONE',  ( 3.464101615137757051, -5.999999999999979572, -77.41367513459478289 ) ) ;
#9695 = CYLINDRICAL_SURFACE ( 'NONE', #24540, 6.000000000000000888 ) ;
#9696 =( GEOMETRIC_REPRESENTATION_CONTEXT ( 3 ) GLOBAL_UNCERTAINTY_ASSIGNED_CONTEXT ( ( #13185 ) ) GLOBAL_UNIT_ASSIGNED_CONTEXT ( ( #23922, #29255, #19910 ) ) REPRESENTATION_CONTEXT ( 'NONE', 'WORKASPACE' ) );
#9697 = VERTEX_POINT ( 'NONE', #4297 ) ;
#9698 = CARTESIAN_POINT ( 'NONE',  ( 0.000000000000000000, 5.999999999999977796, -141.2886751345947971 ) ) ;
#9699 = CARTESIAN_POINT ( 'NONE',  ( 134.3437500000000568, -6.000000000000005329, -2.485281374238555774 ) ) ;
#9700 = VERTEX_POINT ( 'NONE', #26742 ) ;
#9701 = CARTESIAN_POINT ( 'NONE',  ( -3.608439182435115633, 6.249999999999965361, -143.4419872981078470 ) ) ;
#9702 = FACE_OUTER_BOUND ( 'NONE', #800, .T. ) ;
#9703 = AXIS2_PLACEMENT_3D ( 'NONE', #20239, #15814, #15657 ) ;
#9704 = CARTESIAN_POINT ( 'NONE',  ( 10.43750000000004619, 2.649519052838419153, 1.097466725451559322 ) ) ;
#9705 = CARTESIAN_POINT ( 'NONE',  ( 6.000000000000000888, -1.607695154586752384, -116.2306624327026157 ) ) ;
#9706 = AXIS2_PLACEMENT_3D ( 'NONE', #11921, #9267, #27980 ) ;
#9707 = CARTESIAN_POINT ( 'NONE',  ( 6.000000000000000888, -3.330669073875464691E-16, -7.560779664488942560E-35 ) ) ;
#9708 = CARTESIAN_POINT ( 'NONE',  ( 136.0163997308104626, 4.999999999999989342, 2.071067811865468400 ) ) ;
#9709 = CARTESIAN_POINT ( 'NONE',  ( 5.196152422706629359, -2.999999999999988898, -56.28867513459484684 ) ) ;
#9710 = CARTESIAN_POINT ( 'NONE',  ( -3.464101615137725076, 5.999999999999979572, -92.58632486540521711 ) ) ;
#9711 = CARTESIAN_POINT ( 'NONE',  ( 15.16367513459498895, 1.767766952966487448, -1.767766952966431937 ) ) ;
#9712 = CARTESIAN_POINT ( 'NONE',  ( 0.000000000000000000, 5.999999999999977796, -60.28867513459484684 ) ) ;
#9713 = DIRECTION ( 'NONE',  ( -7.147005652999508048E-36, 5.642372883946980038E-36, 1.000000000000000000 ) ) ;
#9714 = CARTESIAN_POINT ( 'NONE',  ( 107.6249999999998721, -1.767766952966376426, -1.767766952966320915 ) ) ;
#9715 = EDGE_CURVE ( 'NONE', #9387, #12037, #27044, .T. ) ;
#9717 = CYLINDRICAL_SURFACE ( 'NONE', #26917, 5.500000000000000000 ) ;
#9716 = AXIS2_PLACEMENT_3D ( 'NONE', #22287, #3363, #29638 ) ;
#9718 = CARTESIAN_POINT ( 'NONE',  ( 3.464101615137852974, 5.999999999999884537, -148.9136751345947687 ) ) ;
#9719 = VERTEX_POINT ( 'NONE', #8325 ) ;
#9720 =( BOUNDED_CURVE ( )  B_SPLINE_CURVE ( 2, ( #25357, #25676, #4624, #14056, #11902, #2342, #11742, #21235, #178 ),
 .UNSPECIFIED., .F., .F. ) 
 B_SPLINE_CURVE_WITH_KNOTS ( ( 3, 2, 2, 2, 3 ),
 ( 0.1718750000000000000, 0.1796875000000000000, 0.1875000000000000000, 0.1953125000000000000, 0.2031250000000000000 ),
 .UNSPECIFIED. ) 
 CURVE ( )  GEOMETRIC_REPRESENTATION_ITEM ( )  RATIONAL_B_SPLINE_CURVE ( ( 1.000000000000000000, 0.9238795325112867385, 1.000000000000000000, 0.9238795325112867385, 1.000000000000000000, 0.9238795325112867385, 1.000000000000000000, 0.9238795325112867385, 1.000000000000000000 ) ) 
 REPRESENTATION_ITEM ( '' )  );
#9721 = CARTESIAN_POINT ( 'NONE',  ( 1.000000000000000888, 2.020667218593133494E-15, 16.50000000000000355 ) ) ;
#9722 = CARTESIAN_POINT ( 'NONE',  ( 3.464101615137852974, 5.999999999999884537, -88.33632486540521711 ) ) ;
#9723 = ADVANCED_FACE ( 'NONE', ( #12986 ), #27525, .T. ) ;
#9724 = CARTESIAN_POINT ( 'NONE',  ( -5.999999999999919176, 1.607695154586804565, -78.90331216351299304 ) ) ;
#9725 = CARTESIAN_POINT ( 'NONE',  ( -5.999999999999963585, 9.296355089585909904E-15, -164.3363248654052313 ) ) ;
#9726 = EDGE_LOOP ( 'NONE', ( #4985, #24699, #2281, #25776 ) ) ;
#9727 = CARTESIAN_POINT ( 'NONE',  ( 115.9997167782376266, -1.308140751793668288, 1.308140751793751555 ) ) ;
#9728 = CARTESIAN_POINT ( 'NONE',  ( 3.608439182435180470, -6.249999999999997335, -105.1919872981078470 ) ) ;
#9729 = CIRCLE ( 'NONE', #14175, 0.5000000000000004441 ) ;
#9730 = CARTESIAN_POINT ( 'NONE',  ( 138.6488248654052313, -3.889087296526011706, -3.889087296526011706 ) ) ;
#9731 = AXIS2_PLACEMENT_3D ( 'NONE', #22215, #13488, #11020 ) ;
#9732 = AXIS2_PLACEMENT_3D ( 'NONE', #14637, #627, #28270 ) ;
#9733 = CARTESIAN_POINT ( 'NONE',  ( 160.7663997308104058, -4.999999999999989342, -2.071067811865468400 ) ) ;
#9734 = CARTESIAN_POINT ( 'NONE',  ( -6.350852961085760029, -1.281975124255709124E-13, -125.6250000000000426 ) ) ;
#9735 = ORIENTED_EDGE ( 'NONE', *, *, #11335, .F. ) ;
#9736 = CARTESIAN_POINT ( 'NONE',  ( -4.763139720814407951, 2.749999999999946709, -56.75000000000002132 ) ) ;
#9737 = DIRECTION ( 'NONE',  ( 1.000000000000000000, -0.000000000000000000, -0.000000000000000000 ) ) ;
#9738 = CARTESIAN_POINT ( 'NONE',  ( 2.775557561562891351E-14, -6.250000000000061284, -85.18301270189220986 ) ) ;
#9739 = UNCERTAINTY_MEASURE_WITH_UNIT (LENGTH_MEASURE( 1.000000000000000082E-05 ), #1638, 'distance_accuracy_value', 'NONE');
#9740 = CARTESIAN_POINT ( 'NONE',  ( 10.06249999999967137, 2.000000000003780087, 0.8284271247425472051 ) ) ;
#9741 = CARTESIAN_POINT ( 'NONE',  ( 154.4136751345948539, 0.000000000000000000, -5.500000000000005329 ) ) ;
#9742 = CARTESIAN_POINT ( 'NONE',  ( 105.3747167782376550, -5.551115123125782702E-14, -1.849990392679523588 ) ) ;
#9743 = CARTESIAN_POINT ( 'NONE',  ( 119.7886751345947829, -1.999999999999946265, 3.330669073875469621E-13 ) ) ;
#9744 = EDGE_CURVE ( 'NONE', #25601, #10258, #325, .T. ) ;
#9745 = CARTESIAN_POINT ( 'NONE',  ( 113.5002832217622455, 1.308140751793696044, 1.308140751793640533 ) ) ;
#9746 = EDGE_CURVE ( 'NONE', #28423, #23930, #6611, .T. ) ;
#9747 = CARTESIAN_POINT ( 'NONE',  ( -6.350852961085760029, -1.281975124255709124E-13, -140.6250000000000000 ) ) ;
#9748 = DIRECTION ( 'NONE',  ( -3.469446951953694061E-16, -1.000000000000000000, 0.000000000000000000 ) ) ;
#9749 = CARTESIAN_POINT ( 'NONE',  ( 3.608439182435180470, 6.249999999999982236, -155.0580127018922383 ) ) ;
#9750 = SURFACE_STYLE_FILL_AREA ( #16247 ) ;
#9751 = CARTESIAN_POINT ( 'NONE',  ( 3.175426480543072749, -5.500000000000105693, -69.62500000000004263 ) ) ;
#9752 = CARTESIAN_POINT ( 'NONE',  ( 4.763139720814407951, -2.749999999999988454, -63.50000000000000000 ) ) ;
#9753 = CARTESIAN_POINT ( 'NONE',  ( 144.8586002691896510, 2.071067811865468400, 4.999999999999989342 ) ) ;
#9754 = CARTESIAN_POINT ( 'NONE',  ( 160.0000000000000284, -59.99999999999980105, -3.000000000000002665 ) ) ;
#9755 = CARTESIAN_POINT ( 'NONE',  ( 158.1562500000000284, -6.000000000000005329, 2.485281374238556218 ) ) ;
#9756 = CARTESIAN_POINT ( 'NONE',  ( 135.0000000000000284, -8.662318014469933658, -7.546724076495860523 ) ) ;
#9757 = CARTESIAN_POINT ( 'NONE',  ( 16.87500000000000000, 1.414213562373256572, -1.414213562373145550 ) ) ;
#9758 = CARTESIAN_POINT ( 'NONE',  ( 0.000000000000000000, 0.000000000000000000, 0.000000000000000000 ) ) ;
#9759 = CYLINDRICAL_SURFACE ( 'NONE', #11093, 1.000000000000000000 ) ;
#9760 =( BOUNDED_CURVE ( )  B_SPLINE_CURVE ( 2, ( #11823, #18261, #16429, #4243, #4397, #8874, #18867, #9169, #28188 ),
 .UNSPECIFIED., .F., .F. ) 
 B_SPLINE_CURVE_WITH_KNOTS ( ( 3, 2, 2, 2, 3 ),
 ( 0.4625000000000009104, 0.4687500000000006661, 0.4750000000000004219, 0.4812500000000002887, 0.4875000000000000444 ),
 .UNSPECIFIED. ) 
 CURVE ( )  GEOMETRIC_REPRESENTATION_ITEM ( )  RATIONAL_B_SPLINE_CURVE ( ( 0.9999999999999892308, 0.9238795325112975076, 1.000000000000000000, 0.9238795325112867385, 1.000000000000000000, 0.9238795325112867385, 1.000000000000000000, 0.9238795325112860723, 1.000000000000000666 ) ) 
 REPRESENTATION_ITEM ( '' )  );
#9761 = ORIENTED_EDGE ( 'NONE', *, *, #683, .T. ) ;
#9762 = CARTESIAN_POINT ( 'NONE',  ( 152.5312500000000000, -2.485281374238555774, -6.000000000000005329 ) ) ;
#9763 = CARTESIAN_POINT ( 'NONE',  ( 118.9761751345946266, -0.8284271247460250898, -1.999999999999851674 ) ) ;
#9764 = CARTESIAN_POINT ( 'NONE',  ( 113.0002832217622455, -1.308140751793585022, -1.308140751793640533 ) ) ;
#9765 = UNCERTAINTY_MEASURE_WITH_UNIT (LENGTH_MEASURE( 1.000000000000000082E-05 ), #8652, 'distance_accuracy_value', 'NONE');
#9766 = CARTESIAN_POINT ( 'NONE',  ( 5.999999999999999112, 2.951592740943527306E-14, -158.1636751345948539 ) ) ;
#9767 = COLOUR_RGB ( '', 0.40784314, 0.44705882, 0.49803922) ;
#9768 = CARTESIAN_POINT ( 'NONE',  ( -3.175426480542816510, 5.499999999999865885, -181.3750000000000000 ) ) ;
#9769 = CARTESIAN_POINT ( 'NONE',  ( 23.06250000000011013, 2.000000000000151879, 0.8284271247462354770 ) ) ;
#9770 = CARTESIAN_POINT ( 'NONE',  ( -3.608439182435115633, 6.249999999999965361, -153.9419872981078186 ) ) ;
#9771 = ORIENTED_EDGE ( 'NONE', *, *, #29842, .F. ) ;
#9772 = CARTESIAN_POINT ( 'NONE',  ( 4.763139720814407951, -2.749999999999988454, -80.00000000000001421 ) ) ;
#9773 = CARTESIAN_POINT ( 'NONE',  ( -3.608439182435115633, 6.249999999999965361, -102.3080127018922383 ) ) ;
#9774 = ORIENTED_EDGE ( 'NONE', *, *, #24019, .F. ) ;
#9775 = DIRECTION ( 'NONE',  ( -1.000000000000000000, -6.938893903907222067E-15, 0.000000000000000000 ) ) ;
#9776 = CARTESIAN_POINT ( 'NONE',  ( 155.4226497308104058, 5.000000000000004441, 0.000000000000000000 ) ) ;
#9777 = LINE ( 'NONE', #26187, #29424 ) ;
#9778 = CARTESIAN_POINT ( 'NONE',  ( 6.000000000000000888, -1.859271017917181981E-14, -72.66367513459482552 ) ) ;
#9779 = CARTESIAN_POINT ( 'NONE',  ( 140.5000000000000284, -10.99818166789400919, 4.800000000000004263 ) ) ;
#9780 = EDGE_CURVE ( 'NONE', #22988, #27301, #15324, .T. ) ;
#9781 = CARTESIAN_POINT ( 'NONE',  ( 4.763139720814407951, -2.749999999999988454, -161.0000000000000284 ) ) ;
#9782 = CARTESIAN_POINT ( 'NONE',  ( 5.196152422706629359, 3.000000000000002665, -58.46132486540523132 ) ) ;
#9783 = CARTESIAN_POINT ( 'NONE',  ( -2.775557561562891351E-14, -5.500000000000115463, -155.2500000000000000 ) ) ;
#9784 = CARTESIAN_POINT ( 'NONE',  ( 112.2499999999998153, -5.551115123125782702E-14, 2.500000000000168754 ) ) ;
#9785 = STYLED_ITEM ( 'NONE', ( #4429 ), #25177 ) ;
#9786 = CARTESIAN_POINT ( 'NONE',  ( -3.175426480542816066, 5.499999999999865885, -103.3750000000000142 ) ) ;
#9787 = DIRECTION ( 'NONE',  ( 0.000000000000000000, 0.000000000000000000, 1.000000000000000000 ) ) ;
#9788 = CARTESIAN_POINT ( 'NONE',  ( 3.175426480543072749, 5.499999999999865885, -88.62500000000001421 ) ) ;
#9789 = CARTESIAN_POINT ( 'NONE',  ( 0.000000000000000000, 0.000000000000000000, 0.000000000000000000 ) ) ;
#9790 = CARTESIAN_POINT ( 'NONE',  ( 24.75000000000010658, 1.665334536937734811E-13, -2.000000000000001776 ) ) ;
#9791 = CARTESIAN_POINT ( 'NONE',  ( 112.0624999999997868, 2.500000000000055067, 1.035533905932989551 ) ) ;
#9792 = CARTESIAN_POINT ( 'NONE',  ( 0.000000000000000000, -5.999999999999991118, -66.46132486540523132 ) ) ;
#9793 = FACE_OUTER_BOUND ( 'NONE', #4509, .T. ) ;
#9794 = CARTESIAN_POINT ( 'NONE',  ( 112.8988248654050892, 0.8284271247463257382, 2.000000000000271783 ) ) ;
#9795 = ORIENTED_EDGE ( 'NONE', *, *, #7508, .T. ) ;
#9796 = CYLINDRICAL_SURFACE ( 'NONE', #19538, 6.000000000000000888 ) ;
#9797 = CARTESIAN_POINT ( 'NONE',  ( -0.04562205425674009662, -14.50000000000001243, -8.291335958003937634 ) ) ;
#9798 = CARTESIAN_POINT ( 'NONE',  ( 107.3122167782375413, -0.7662911109077087390, -1.849990392679291551 ) ) ;
#9799 = VERTEX_POINT ( 'NONE', #3248 ) ;
#9800 = ORIENTED_EDGE ( 'NONE', *, *, #3778, .F. ) ;
#9801 = CARTESIAN_POINT ( 'NONE',  ( 146.9062500000000284, 6.000000000000005329, -2.485281374238555774 ) ) ;
#9802 = ORIENTED_EDGE ( 'NONE', *, *, #4170, .T. ) ;
#9803 = EDGE_CURVE ( 'NONE', #10990, #13661, #7298, .T. ) ;
#9804 = CARTESIAN_POINT ( 'NONE',  ( -2.775557561562891351E-14, -5.500000000000115463, -113.2500000000000142 ) ) ;
#9805 = CARTESIAN_POINT ( 'NONE',  ( 17.00000000000001421, -1.873492889144789952, -1.873492889144956486 ) ) ;
#9806 = CARTESIAN_POINT ( 'NONE',  ( 3.608439182435180470, 6.249999999999982236, -120.5580127018922667 ) ) ;
#9807 = VERTEX_POINT ( 'NONE', #12678 ) ;
#9808 = CARTESIAN_POINT ( 'NONE',  ( 0.000000000000000000, -5.999999999999991118, -68.53867513459482552 ) ) ;
#9809 = MECHANICAL_DESIGN_GEOMETRIC_PRESENTATION_REPRESENTATION (  '', ( #17673 ), #29892 ) ;
#9810 = CARTESIAN_POINT ( 'NONE',  ( 7.216878364870455975, -6.409875621278545621E-14, -158.9419872981077901 ) ) ;
#9811 = CARTESIAN_POINT ( 'NONE',  ( 109.5624999999997158, -2.499999999999994671, -1.035533905932508825 ) ) ;
#9812 = COLOUR_RGB ( '', 0.31764706, 0.68627451, 0.89019608) ;
#9813 = SURFACE_STYLE_FILL_AREA ( #26374 ) ;
#9814 = VERTEX_POINT ( 'NONE', #949 ) ;
#9815 = EDGE_CURVE ( 'NONE', #17555, #25961, #9478, .T. ) ;
#9816 = CARTESIAN_POINT ( 'NONE',  ( 158.8199251345948824, -2.278174593051888408, -5.500000000000135891 ) ) ;
#9817 = CARTESIAN_POINT ( 'NONE',  ( -5.196152422706601826, 2.999999999999975131, -137.4613248654051745 ) ) ;
#9818 = CARTESIAN_POINT ( 'NONE',  ( 6.350852961086080661, -9.614813431917819062E-14, -177.3750000000000284 ) ) ;
#9819 = CARTESIAN_POINT ( 'NONE',  ( 109.6877832217621318, -0.7662911109076485650, 1.849990392679652151 ) ) ;
#9820 = CARTESIAN_POINT ( 'NONE',  ( -5.999999999999956479, -1.607695154586745057, -113.2693375672974128 ) ) ;
#9821 = CARTESIAN_POINT ( 'NONE',  ( 2.775557561562891351E-14, -6.250000000000061284, -179.6830127018922383 ) ) ;
#9822 = CARTESIAN_POINT ( 'NONE',  ( 5.196152422706629359, 3.000000000000002665, -76.46132486540524553 ) ) ;
#9823 = CARTESIAN_POINT ( 'NONE',  ( 4.763139720814407951, -2.749999999999988454, -128.0000000000000000 ) ) ;
#9824 = FACE_OUTER_BOUND ( 'NONE', #21597, .T. ) ;
#9825 = CARTESIAN_POINT ( 'NONE',  ( -3.175426480542816510, 5.499999999999865885, -112.3750000000000426 ) ) ;
#9826 = CARTESIAN_POINT ( 'NONE',  ( 16.46132486540524553, 2.220446049250313081E-13, -2.500000000000002220 ) ) ;
#9827 = ORIENTED_EDGE ( 'NONE', *, *, #29732, .T. ) ;
#9828 = CARTESIAN_POINT ( 'NONE',  ( 18.25000000000012790, -1.873492889144789952, -1.873492889145067508 ) ) ;
#9829 = CARTESIAN_POINT ( 'NONE',  ( -0.004068020306998300362, -15.42148939562913945, -6.273618375958268878 ) ) ;
#9830 = AXIS2_PLACEMENT_3D ( 'NONE', #25968, #7671, #9392 ) ;
#9831 = CARTESIAN_POINT ( 'NONE',  ( -3.464101615137757051, -5.999999999999979572, -137.0863248654051745 ) ) ;
#9832 = CARTESIAN_POINT ( 'NONE',  ( 18.14882486540516737, -2.499999999999964473, 1.035533905932869425 ) ) ;
#9833 = ORIENTED_EDGE ( 'NONE', *, *, #15571, .F. ) ;
#9834 = CARTESIAN_POINT ( 'NONE',  ( 111.4761751345947260, 0.8284271247462354770, 2.000000000000212275 ) ) ;
#9835 = CARTESIAN_POINT ( 'NONE',  ( -4.763139720814407951, 2.749999999999946709, -178.2500000000000284 ) ) ;
#9836 = FILL_AREA_STYLE_COLOUR ( '', #17565 ) ;
#9837 = ORIENTED_EDGE ( 'NONE', *, *, #13594, .F. ) ;
#9838 = CARTESIAN_POINT ( 'NONE',  ( -20.99999999999998224, -54.99999999999990763, -5.000000000000004441 ) ) ;
#9839 = VERTEX_POINT ( 'NONE', #16471 ) ;
#9840 = ORIENTED_EDGE ( 'NONE', *, *, #25544, .T. ) ;
#9841 = CARTESIAN_POINT ( 'NONE',  ( 132.5625000000000284, -4.242640687119298093, 4.242640687119298093 ) ) ;
#9842 = CARTESIAN_POINT ( 'NONE',  ( 162.0000000000000284, 6.000000000000005329, 0.000000000000000000 ) ) ;
#9843 = EDGE_CURVE ( 'NONE', #28330, #18627, #12015, .T. ) ;
#9844 =( BOUNDED_CURVE ( )  B_SPLINE_CURVE ( 2, ( #25063, #22785, #22633, #1573, #19098, #11599, #18956, #4786, #23699 ),
 .UNSPECIFIED., .F., .T. ) 
 B_SPLINE_CURVE_WITH_KNOTS ( ( 3, 2, 2, 2, 3 ),
 ( 0.2656250000000000000, 0.2734375000000000000, 0.2812500000000000000, 0.2890625000000000000, 0.2968750000000000000 ),
 .UNSPECIFIED. ) 
 CURVE ( )  GEOMETRIC_REPRESENTATION_ITEM ( )  RATIONAL_B_SPLINE_CURVE ( ( 1.000000000000000000, 0.9238795325112867385, 1.000000000000000000, 0.9238795325112867385, 1.000000000000000000, 0.9238795325112867385, 1.000000000000000000, 0.9238795325112867385, 1.000000000000000000 ) ) 
 REPRESENTATION_ITEM ( '' )  );
#9845 = CARTESIAN_POINT ( 'NONE',  ( 10.81250000000001243, 0.8284271247461753029, -2.000000000000091926 ) ) ;
#9846 = ORIENTED_EDGE ( 'NONE', *, *, #29723, .F. ) ;
#9847 = CARTESIAN_POINT ( 'NONE',  ( -5.412658773652739619, 3.124999999999975131, -128.3169872981078186 ) ) ;
#9848 = DIRECTION ( 'NONE',  ( 0.000000000000000000, 0.000000000000000000, -1.000000000000000000 ) ) ;
#9849 = CARTESIAN_POINT ( 'NONE',  ( 12.06250000000005507, -1.097466725451379244, -2.649519052838419153 ) ) ;
#9850 = CARTESIAN_POINT ( 'NONE',  ( 161.0000000000000284, 0.000000000000000000, 0.000000000000000000 ) ) ;
#9851 = AXIS2_PLACEMENT_3D ( 'NONE', #24408, #29152, #8112 ) ;
#9852 = VERTEX_POINT ( 'NONE', #28382 ) ;
#9853 = CARTESIAN_POINT ( 'NONE',  ( 18.56250000000005329, -1.999999999999971800, -0.8284271247462354770 ) ) ;
#9854 = CARTESIAN_POINT ( 'NONE',  ( 3.464101615137757051, -5.999999999999979572, -129.9136751345947687 ) ) ;
#9855 = EDGE_CURVE ( 'NONE', #16482, #29957, #18392, .T. ) ;
#9856 = CARTESIAN_POINT ( 'NONE',  ( 6.000000000000000888, -1.859271017917181981E-14, -147.0863248654052313 ) ) ;
#9857 =( BOUNDED_CURVE ( )  B_SPLINE_CURVE ( 2, ( #12370, #21719, #9439, #10041, #28743, #7715, #18822, #28148, #7116 ),
 .UNSPECIFIED., .F., .F. ) 
 B_SPLINE_CURVE_WITH_KNOTS ( ( 3, 2, 2, 2, 3 ),
 ( 0.4027777777777777901, 0.4037037037037036757, 0.4055555555555555580, 0.4074074074074074403, 0.4083333333333333259 ),
 .UNSPECIFIED. ) 
 CURVE ( )  GEOMETRIC_REPRESENTATION_ITEM ( )  RATIONAL_B_SPLINE_CURVE ( ( 0.9330127018922194093, 0.9330127018922194093, 1.000000000000000000, 0.8660254037844388186, 1.000000000000000000, 0.8660254037844388186, 1.000000000000000000, 0.9330127018922194093, 0.9330127018922194093 ) ) 
 REPRESENTATION_ITEM ( '' )  );
#9858 = EDGE_CURVE ( 'NONE', #4225, #30104, #6937, .T. ) ;
#9859 = AXIS2_PLACEMENT_3D ( 'NONE', #16189, #18622, #10958 ) ;
#9860 = CARTESIAN_POINT ( 'NONE',  ( 140.9851497308104058, -3.535533905932725318, 3.535533905932725318 ) ) ;
#9861 = CARTESIAN_POINT ( 'NONE',  ( 12.33632486540522954, -1.767766952966320915, -1.767766952966542959 ) ) ;
#9862 = CARTESIAN_POINT ( 'NONE',  ( -5.196152422706573404, -3.000000000000002665, -140.2113248654052313 ) ) ;
#9863 = CYLINDRICAL_SURFACE ( 'NONE', #8669, 5.500000000000000000 ) ;
#9864 = CARTESIAN_POINT ( 'NONE',  ( 109.1488248654050750, -1.999999999999941602, 0.8284271247463557142 ) ) ;
#9865 = CARTESIAN_POINT ( 'NONE',  ( 106.7499999999999147, -8.326672684688674053E-14, -2.499999999999946709 ) ) ;
#9866 = B_SPLINE_CURVE_WITH_KNOTS ( 'NONE', 3,
 ( #24267, #21695, #10015, #26277, #19393, #26710, #918, #2778, #7833, #6150, #4139, #27472, #15877, #13561, #24735, #5825, #15566, #29172, #18015, #8607, #3833, #1844, #6297, #8133, #1219, #10630 ),
 .UNSPECIFIED., .F., .F.,
 ( 4, 2, 2, 2, 2, 2, 2, 2, 2, 2, 2, 2, 4 ),
 ( 0.001330568787003978985, 0.001691992223416138690, 0.002053415659828298177, 0.002776262532652618020, 0.003499109405476936996, 0.003860532841889096484, 0.004221956278301255971, 0.004583379714713415459, 0.004944803151125575814, 0.005667650023949893923, 0.006029073460362054278, 0.006390496896774213766, 0.007113343769598531874 ),
 .UNSPECIFIED. ) ;
#9867 = CARTESIAN_POINT ( 'NONE',  ( 5.196152422706629359, -2.999999999999988898, -142.7113248654052313 ) ) ;
#9868 = CARTESIAN_POINT ( 'NONE',  ( -6.350852961085760029, -1.281975124255709124E-13, -139.1250000000000000 ) ) ;
#9869 = CARTESIAN_POINT ( 'NONE',  ( -0.5000000000000004441, -9.500000000000008882, 8.000000000000007105 ) ) ;
#9870 = CARTESIAN_POINT ( 'NONE',  ( 153.8511751345948539, -3.889087296526011706, 3.889087296526011706 ) ) ;
#9871 = ORIENTED_EDGE ( 'NONE', *, *, #14063, .F. ) ;
#9872 = SURFACE_STYLE_USAGE ( .BOTH. , #18198 ) ;
#9873 = ORIENTED_EDGE ( 'NONE', *, *, #1725, .F. ) ;
#9874 = CARTESIAN_POINT ( 'NONE',  ( 115.6872167782374561, 1.849990392679532247, 0.7662911109080692285 ) ) ;
#9875 = CARTESIAN_POINT ( 'NONE',  ( 136.3125000000000284, 4.242640687119298093, -4.242640687119298093 ) ) ;
#9876 = CARTESIAN_POINT ( 'NONE',  ( 12.00000000000012079, 2.000000000000112799, -1.665334536937734811E-13 ) ) ;
#9877 = CARTESIAN_POINT ( 'NONE',  ( -3.608439182435052128, -6.250000000000110134, -106.9419872981077901 ) ) ;
#9878 = STYLED_ITEM ( 'NONE', ( #5855 ), #28673 ) ;
#9879 = CARTESIAN_POINT ( 'NONE',  ( 160.4851497308104058, -3.535533905932725318, 3.535533905932725318 ) ) ;
#9880 = CARTESIAN_POINT ( 'NONE',  ( 117.9999999999997868, 2.500000000000002220, 2.220446049250313081E-13 ) ) ;
#9881 = PRESENTATION_LAYER_ASSIGNMENT (  '', '', ( #7894 ) ) ;
#9882 = VECTOR ( 'NONE', #28236, 1000.000000000000000 ) ;
#9883 = EDGE_CURVE ( 'NONE', #5798, #23261, #2062, .T. ) ;
#9884 = CARTESIAN_POINT ( 'NONE',  ( -4.763139720814407951, -2.750000000000016431, -127.0000000000000000 ) ) ;
#9885 = ORIENTED_EDGE ( 'NONE', *, *, #19488, .F. ) ;
#9886 = EDGE_LOOP ( 'NONE', ( #6838, #29262, #13298, #27995 ) ) ;
#9887 = DIRECTION ( 'NONE',  ( 1.000000000000000000, 0.000000000000000000, 0.000000000000000000 ) ) ;
#9888 = CARTESIAN_POINT ( 'NONE',  ( 3.175426480543072749, 5.499999999999865885, -54.12500000000003553 ) ) ;
#9889 = CARTESIAN_POINT ( 'NONE',  ( -5.196152422706573404, -3.000000000000002665, -179.7886751345948539 ) ) ;
#9890 = LINE ( 'NONE', #19264, #26444 ) ;
#9891 = EDGE_CURVE ( 'NONE', #12627, #23669, #12927, .T. ) ;
#9892 = CARTESIAN_POINT ( 'NONE',  ( -5.412658773652684552, -3.125000000000099920, -83.93301270189223828 ) ) ;
#9893 = DIRECTION ( 'NONE',  ( -1.000000000000000000, -1.665334536937736783E-16, -2.220446049250315546E-16 ) ) ;
#9894 =( BOUNDED_CURVE ( )  B_SPLINE_CURVE ( 2, ( #17729, #6020, #29822, #1871, #29520, #19849, #27357, #20320, #8158 ),
 .UNSPECIFIED., .F., .F. ) 
 B_SPLINE_CURVE_WITH_KNOTS ( ( 3, 2, 2, 2, 3 ),
 ( 0.03055555555555556149, 0.03148148148148147835, 0.03333333333333333287, 0.03518518518518518740, 0.03611111111111110772 ),
 .UNSPECIFIED. ) 
 CURVE ( )  GEOMETRIC_REPRESENTATION_ITEM ( )  RATIONAL_B_SPLINE_CURVE ( ( 0.9330127018922194093, 0.9330127018922198534, 1.000000000000000000, 0.8660254037844388186, 1.000000000000000000, 0.8660254037844388186, 1.000000000000000000, 0.9330127018922196314, 0.9330127018922194093 ) ) 
 REPRESENTATION_ITEM ( '' )  );
#9895 = CARTESIAN_POINT ( 'NONE',  ( 105.1872167782375556, -1.849990392679441875, -0.7662911109075883909 ) ) ;
#9896 = CARTESIAN_POINT ( 'NONE',  ( -6.000000000000000888, 1.067854986875958443E-15, 7.560779664488942560E-35 ) ) ;
#9897 = AXIS2_PLACEMENT_3D ( 'NONE', #8083, #17810, #17351 ) ;
#9898 = CARTESIAN_POINT ( 'NONE',  ( 116.3752832217622597, 1.849990392679523588, 0.000000000000000000 ) ) ;
#9899 = CARTESIAN_POINT ( 'NONE',  ( 3.175426480543072749, -5.500000000000105693, -137.1250000000000568 ) ) ;
#9900 = CARTESIAN_POINT ( 'NONE',  ( 3.464101615137757051, -5.999999999999979572, -105.3363248654052171 ) ) ;
#9901 = AXIS2_PLACEMENT_3D ( 'NONE', #29974, #29672, #27208 ) ;
#9902 = CARTESIAN_POINT ( 'NONE',  ( 5.412658773652739619, 3.124999999999988898, -156.6830127018922099 ) ) ;
#9903 = CARTESIAN_POINT ( 'NONE',  ( 139.6949251345948255, 5.500000000000012434, -2.278174593052012309 ) ) ;
#9904 = CARTESIAN_POINT ( 'NONE',  ( -3.175426480542816066, 5.499999999999865885, -74.87500000000000000 ) ) ;
#9905 = CARTESIAN_POINT ( 'NONE',  ( -6.350852961085760029, -1.281975124255709124E-13, -65.62500000000002842 ) ) ;
#9906 = FACE_OUTER_BOUND ( 'NONE', #24079, .T. ) ;
#9907 = CARTESIAN_POINT ( 'NONE',  ( 145.9836002691896510, 4.999999999999989342, -2.071067811865468400 ) ) ;
#9908 = CARTESIAN_POINT ( 'NONE',  ( 154.5937500000000284, 6.000000000000005329, 2.485281374238585972 ) ) ;
#9909 = CARTESIAN_POINT ( 'NONE',  ( -5.999999999999963585, -1.487416814333745711E-14, -97.41367513459481131 ) ) ;
#9910 = CARTESIAN_POINT ( 'NONE',  ( -6.000000000000007105, -1.607695154586655129, -58.34668783648704959 ) ) ;
#9911 = CARTESIAN_POINT ( 'NONE',  ( 115.9372167782375129, -0.7662911109076785410, 1.849990392679712103 ) ) ;
#9912 = CARTESIAN_POINT ( 'NONE',  ( 0.000000000000000000, 0.000000000000000000, 0.000000000000000000 ) ) ;
#9913 = ORIENTED_EDGE ( 'NONE', *, *, #30074, .F. ) ;
#9914 = CARTESIAN_POINT ( 'NONE',  ( 150.0937500000000284, 6.000000000000005329, 2.485281374238585972 ) ) ;
#9915 = CARTESIAN_POINT ( 'NONE',  ( 118.9136751345948113, -1.414213562373173305, -1.414213562373034527 ) ) ;
#9916 =( GEOMETRIC_REPRESENTATION_CONTEXT ( 3 ) GLOBAL_UNCERTAINTY_ASSIGNED_CONTEXT ( ( #26321 ) ) GLOBAL_UNIT_ASSIGNED_CONTEXT ( ( #12459, #19502, #28834 ) ) REPRESENTATION_CONTEXT ( 'NONE', 'WORKASPACE' ) );
#9917 = VECTOR ( 'NONE', #13135, 1000.000000000000000 ) ;
#9918 = EDGE_CURVE ( 'NONE', #23551, #23148, #2309, .T. ) ;
#9919 = EDGE_CURVE ( 'NONE', #12844, #2708, #28742, .T. ) ;
#9920 = DIRECTION ( 'NONE',  ( -7.147005652999508048E-36, 5.642372883946980038E-36, 1.000000000000000000 ) ) ;
#9921 = CARTESIAN_POINT ( 'NONE',  ( -3.608439182435115633, 6.249999999999965361, -47.44198729810783277 ) ) ;
#9922 = CARTESIAN_POINT ( 'NONE',  ( 20.87500000000014211, 1.414213562373367594, -1.414213562373145550 ) ) ;
#9923 = ORIENTED_EDGE ( 'NONE', *, *, #7373, .T. ) ;
#9924 = CARTESIAN_POINT ( 'NONE',  ( -3.175426480542816510, 5.499999999999865885, -79.37500000000001421 ) ) ;
#9925 = CARTESIAN_POINT ( 'NONE',  ( 3.608439182435180470, -6.249999999999997335, -98.55801270189222407 ) ) ;
#9926 = ORIENTED_EDGE ( 'NONE', *, *, #4629, .F. ) ;
#9927 = CARTESIAN_POINT ( 'NONE',  ( 139.5000000000000284, -54.99999999999990763, -7.500000000000007105 ) ) ;
#9928 = CYLINDRICAL_SURFACE ( 'NONE', #19627, 6.000000000000000888 ) ;
#9929 = CARTESIAN_POINT ( 'NONE',  ( -5.999999999999919176, 1.607695154586804565, -58.48066243270260856 ) ) ;
#9930 = CYLINDRICAL_SURFACE ( 'NONE', #15219, 5.500000000000000000 ) ;
#9931 = CARTESIAN_POINT ( 'NONE',  ( 0.000000000000000000, -5.999999999999991118, -58.96132486540523132 ) ) ;
#9932 = PRESENTATION_STYLE_ASSIGNMENT (( #12119 ) ) ;
#9933 = CARTESIAN_POINT ( 'NONE',  ( 6.350852961086080661, -9.614813431917819062E-14, -165.3750000000000568 ) ) ;
#9934 = DIRECTION ( 'NONE',  ( 0.000000000000000000, -1.000000000000000000, 0.000000000000000000 ) ) ;
#9935 = CARTESIAN_POINT ( 'NONE',  ( -3.175426480542816510, -5.500000000000057732, -158.3750000000000284 ) ) ;
#9936 = DIRECTION ( 'NONE',  ( 0.000000000000000000, 0.000000000000000000, 1.000000000000000000 ) ) ;
#9937 = CARTESIAN_POINT ( 'NONE',  ( -3.175426480542816066, -5.500000000000057732, -90.87500000000001421 ) ) ;
#9938 = CARTESIAN_POINT ( 'NONE',  ( -5.999999999999971578, 1.607695154586715303, -125.4033121635129930 ) ) ;
#9939 = CARTESIAN_POINT ( 'NONE',  ( 115.6011751345946550, -0.8284271247461453269, 2.000000000000332179 ) ) ;
#9940 = CARTESIAN_POINT ( 'NONE',  ( -3.175426480542816510, -5.500000000000057732, -90.87500000000001421 ) ) ;
#9941 =( BOUNDED_CURVE ( )  B_SPLINE_CURVE ( 2, ( #8428, #17834, #761, #10145, #28848, #19516, #24547, #7806, #3498 ),
 .UNSPECIFIED., .F., .F. ) 
 B_SPLINE_CURVE_WITH_KNOTS ( ( 3, 2, 2, 2, 3 ),
 ( 0.2750000000000000222, 0.2759259259259259078, 0.2777777777777777901, 0.2796296296296296169, 0.2805555555555555580 ),
 .UNSPECIFIED. ) 
 CURVE ( )  GEOMETRIC_REPRESENTATION_ITEM ( )  RATIONAL_B_SPLINE_CURVE ( ( 0.9330127018922194093, 0.9330127018922214077, 1.000000000000000000, 0.8660254037844388186, 1.000000000000000000, 0.8660254037844388186, 1.000000000000000000, 0.9330127018922194093, 0.9330127018922194093 ) ) 
 REPRESENTATION_ITEM ( '' )  );
#9942 = CARTESIAN_POINT ( 'NONE',  ( 135.0863248654052313, 0.000000000000000000, 5.500000000000005329 ) ) ;
#9943 = CARTESIAN_POINT ( 'NONE',  ( 107.2886751345947118, 2.000000000000085265, 1.110223024625156540E-13 ) ) ;
#9944 = CARTESIAN_POINT ( 'NONE',  ( 23.43750000000010303, -1.999999999999851674, 0.8284271247462955401 ) ) ;
#9945 = CARTESIAN_POINT ( 'NONE',  ( 113.0624999999997726, 2.500000000000084821, 1.035533905932989551 ) ) ;
#9946 = DIRECTION ( 'NONE',  ( 1.000000000000000000, -5.551115123125773458E-17, -1.260129944081490338E-35 ) ) ;
#9947 = CARTESIAN_POINT ( 'NONE',  ( 113.0238248654049613, -0.8284271247460852639, 2.000000000000271783 ) ) ;
#9948 = VERTEX_POINT ( 'NONE', #20905 ) ;
#9949 = CARTESIAN_POINT ( 'NONE',  ( -5.999999999999963585, 1.780251999655701777E-13, -58.41367513459482552 ) ) ;
#9950 = DIRECTION ( 'NONE',  ( -7.147005652999508048E-36, 5.642372883946980038E-36, 1.000000000000000000 ) ) ;
#9951 = CARTESIAN_POINT ( 'NONE',  ( 121.1252832217622597, -5.551115123125782702E-14, -1.849990392679523588 ) ) ;
#9952 = EDGE_LOOP ( 'NONE', ( #23677, #28860, #24374, #28680 ) ) ;
#9953 = EDGE_CURVE ( 'NONE', #12660, #9038, #22260, .T. ) ;
#9954 = ORIENTED_EDGE ( 'NONE', *, *, #713, .T. ) ;
#9955 = ORIENTED_EDGE ( 'NONE', *, *, #7383, .F. ) ;
#9956 = CARTESIAN_POINT ( 'NONE',  ( 3.175426480543072749, -5.500000000000105693, -107.1250000000000284 ) ) ;
#9957 = CARTESIAN_POINT ( 'NONE',  ( 18.00000000000012790, -1.873492889144789952, -1.873492889145123019 ) ) ;
#9958 = CARTESIAN_POINT ( 'NONE',  ( 3.175426480543072749, 5.499999999999865885, -150.1250000000000284 ) ) ;
#9959 = CARTESIAN_POINT ( 'NONE',  ( 3.608439182435180470, -6.249999999999997335, -125.5580127018922383 ) ) ;
#9960 = VERTEX_POINT ( 'NONE', #12605 ) ;
#9961 = CYLINDRICAL_SURFACE ( 'NONE', #14255, 6.000000000000000888 ) ;
#9962 = CARTESIAN_POINT ( 'NONE',  ( 5.412658773652712085, -3.125000000000086153, -160.5669872981078186 ) ) ;
#9963 = CARTESIAN_POINT ( 'NONE',  ( 109.6874999999997868, -1.035533905932659149, -2.499999999999724221 ) ) ;
#9964 = CARTESIAN_POINT ( 'NONE',  ( 132.5476497308104058, 0.000000000000000000, -5.000000000000004441 ) ) ;
#9965 = CARTESIAN_POINT ( 'NONE',  ( -3.608439182435052128, -6.250000000000110134, -56.80801270189228092 ) ) ;
#9966 = VERTEX_POINT ( 'NONE', #10132 ) ;
#9967 = CARTESIAN_POINT ( 'NONE',  ( 3.464101615137852974, 5.999999999999884537, -167.8363248654051745 ) ) ;
#9968 = CARTESIAN_POINT ( 'NONE',  ( 158.1636751345948255, 0.000000000000000000, 5.500000000000005329 ) ) ;
#9969 = CARTESIAN_POINT ( 'NONE',  ( 141.8363248654052029, 0.000000000000000000, -5.500000000000005329 ) ) ;
#9970 = CARTESIAN_POINT ( 'NONE',  ( -3.175426480542816510, 5.499999999999865885, -179.8750000000000000 ) ) ;
#9971 = CARTESIAN_POINT ( 'NONE',  ( 120.7499999999998721, 1.110223024625156540E-13, -2.499999999999946709 ) ) ;
#9972 = CARTESIAN_POINT ( 'NONE',  ( 0.000000000000000000, -14.26420856792215552, 8.432299132049415391 ) ) ;
#9973 = CARTESIAN_POINT ( 'NONE',  ( 5.412658773652739619, 3.124999999999988898, -179.1830127018922383 ) ) ;
#9974 = DIRECTION ( 'NONE',  ( 0.000000000000000000, 1.224646799147353454E-16, 1.000000000000000000 ) ) ;
#9975 = CARTESIAN_POINT ( 'NONE',  ( 0.000000000000000000, -5.999999999999991118, -48.46132486540521711 ) ) ;
#9976 = CARTESIAN_POINT ( 'NONE',  ( -3.175426480542816066, -5.500000000000057732, -117.8750000000000142 ) ) ;
#9977 = CARTESIAN_POINT ( 'NONE',  ( 135.8074773656872765, -8.774755822434132213, 8.164331751096858270 ) ) ;
#9978 = CARTESIAN_POINT ( 'NONE',  ( 4.763139720814407951, 2.750000000000002665, -117.2500000000000142 ) ) ;
#9979 = DIRECTION ( 'NONE',  ( -6.938893903907222067E-15, -1.000000000000000000, 0.000000000000000000 ) ) ;
#9980 = CARTESIAN_POINT ( 'NONE',  ( -5.999999999999963585, 8.134310703387671600E-14, -131.9136751345948255 ) ) ;
#9981 = ORIENTED_EDGE ( 'NONE', *, *, #9918, .T. ) ;
#9982 = CARTESIAN_POINT ( 'NONE',  ( 18.06250000000012079, -2.649519052838178457, 1.097466725451499370 ) ) ;
#9983 = EDGE_CURVE ( 'NONE', #3651, #2002, #12433, .T. ) ;
#9984 = CARTESIAN_POINT ( 'NONE',  ( 0.9867564579130563285, -16.18227523715626504, 6.671628312105942982 ) ) ;
#9985 = CARTESIAN_POINT ( 'NONE',  ( -5.999999999999971578, 1.607695154586715303, -167.9806624327025872 ) ) ;
#9986 = ORIENTED_EDGE ( 'NONE', *, *, #14649, .F. ) ;
#9987 = DIRECTION ( 'NONE',  ( 0.000000000000000000, 0.000000000000000000, 1.000000000000000000 ) ) ;
#9988 = CARTESIAN_POINT ( 'NONE',  ( -3.175426480542816066, 5.499999999999865885, -176.8750000000000568 ) ) ;
#9989 = AXIS2_PLACEMENT_3D ( 'NONE', #22637, #29207, #3560 ) ;
#9990 = CARTESIAN_POINT ( 'NONE',  ( 22.52382486540525974, 1.035533905932749299, -2.500000000000024425 ) ) ;
#9991 = ORIENTED_EDGE ( 'NONE', *, *, #20556, .F. ) ;
#9992 = CARTESIAN_POINT ( 'NONE',  ( 6.000000000000000888, -1.859271017917181981E-14, -125.1636751345948397 ) ) ;
#9993 = ADVANCED_FACE ( 'NONE', ( #9824 ), #15040, .F. ) ;
#9994 = ORIENTED_EDGE ( 'NONE', *, *, #8517, .T. ) ;
#9995 = ORIENTED_EDGE ( 'NONE', *, *, #13141, .F. ) ;
#9996 = DIRECTION ( 'NONE',  ( -1.000000000000000000, -1.665334536937736783E-16, -2.220446049250315546E-16 ) ) ;
#9997 = CARTESIAN_POINT ( 'NONE',  ( 132.6711002691896795, 4.999999999999989342, 2.071067811865468400 ) ) ;
#9998 = ORIENTED_EDGE ( 'NONE', *, *, #24053, .F. ) ;
#9999 = DIRECTION ( 'NONE',  ( 0.000000000000000000, 0.000000000000000000, -1.000000000000000000 ) ) ;
#10000 = CARTESIAN_POINT ( 'NONE',  ( 5.412658773652712085, -3.125000000000086153, -132.0669872981078470 ) ) ;
#10001 = DIRECTION ( 'NONE',  ( -7.147005652999508048E-36, 5.642372883946980038E-36, 1.000000000000000000 ) ) ;
#10002 = DIRECTION ( 'NONE',  ( -7.147005652999508048E-36, 5.642372883946980038E-36, 1.000000000000000000 ) ) ;
#10003 = CARTESIAN_POINT ( 'NONE',  ( 144.2886751345948539, 5.500000000000005329, 0.000000000000000000 ) ) ;
#10004 = VERTEX_POINT ( 'NONE', #28674 ) ;
#10005 = CARTESIAN_POINT ( 'NONE',  ( 20.62500000000014211, -1.414213562372979016, -1.414213562373145550 ) ) ;
#10006 = DIRECTION ( 'NONE',  ( 0.000000000000000000, 0.000000000000000000, 1.000000000000000000 ) ) ;
#10007 = CARTESIAN_POINT ( 'NONE',  ( 6.000000000000000888, -1.859271017917181981E-14, -136.5863248654051745 ) ) ;
#10008 = CARTESIAN_POINT ( 'NONE',  ( 139.0163997308104342, 4.999999999999989342, 2.071067811865468400 ) ) ;
#10009 = CARTESIAN_POINT ( 'NONE',  ( 6.000000000000000888, -3.330669073875464691E-16, -7.560779664488942560E-35 ) ) ;
#10010 = CARTESIAN_POINT ( 'NONE',  ( 0.000000000000000000, -14.50000000000001243, 8.000000000000007105 ) ) ;
#10011 = CIRCLE ( 'NONE', #17881, 15.00000000000000000 ) ;
#10012 = CARTESIAN_POINT ( 'NONE',  ( 107.4999999999999716, -2.499999999999891198, 3.330669073875469621E-13 ) ) ;
#10013 = CARTESIAN_POINT ( 'NONE',  ( 3.175426480543072749, -5.500000000000105693, -137.1250000000000568 ) ) ;
#10014 = CARTESIAN_POINT ( 'NONE',  ( 108.6488248654049045, 2.000000000000061728, -0.8284271247459350507 ) ) ;
#10015 = CARTESIAN_POINT ( 'NONE',  ( 104.7401757384974132, 1.838163912978949099, -0.2412767149991470184 ) ) ;
#10016 = EDGE_LOOP ( 'NONE', ( #11036, #22124, #7520, #18285 ) ) ;
#10017 = ADVANCED_FACE ( 'NONE', ( #24387 ), #19201, .F. ) ;
#10018 = CARTESIAN_POINT ( 'NONE',  ( 108.1636751345946976, 1.414213562373145550, -1.414213562373034527 ) ) ;
#10019 = CARTESIAN_POINT ( 'NONE',  ( 6.000000000000000888, 1.743066579297358182E-13, -76.58632486540523132 ) ) ;
#10020 = CARTESIAN_POINT ( 'NONE',  ( 153.5550748654052029, -5.500000000000012434, -2.278174593052012309 ) ) ;
#10021 = ORIENTED_EDGE ( 'NONE', *, *, #11941, .F. ) ;
#10022 = CARTESIAN_POINT ( 'NONE',  ( 116.3747167782375840, 5.551115123125782702E-14, -1.849990392679190521 ) ) ;
#10023 = CARTESIAN_POINT ( 'NONE',  ( 118.5386751345946124, 8.326672684688674053E-14, 2.000000000000112799 ) ) ;
#10024 = CARTESIAN_POINT ( 'NONE',  ( 11.06250000000006928, 2.000000000000091926, 0.8284271247461753029 ) ) ;
#10025 = CARTESIAN_POINT ( 'NONE',  ( -3.608439182435115633, 6.249999999999965361, -93.94198729810786119 ) ) ;
#10026 =( NAMED_UNIT ( * ) PLANE_ANGLE_UNIT ( ) SI_UNIT ( $, .RADIAN. ) );
#10027 = EDGE_CURVE ( 'NONE', #16677, #21329, #20522, .T. ) ;
#10028 =( BOUNDED_CURVE ( )  B_SPLINE_CURVE ( 2, ( #23326, #1796, #20390, #11363, #13362, #2116, #6716, #11202, #22707 ),
 .UNSPECIFIED., .F., .T. ) 
 B_SPLINE_CURVE_WITH_KNOTS ( ( 3, 2, 2, 2, 3 ),
 ( 0.5125000000000009548, 0.5187500000000008216, 0.5250000000000005773, 0.5312500000000002220, 0.5374999999999999778 ),
 .UNSPECIFIED. ) 
 CURVE ( )  GEOMETRIC_REPRESENTATION_ITEM ( )  RATIONAL_B_SPLINE_CURVE ( ( 0.9999999999999877875, 0.9238795325112989509, 1.000000000000000000, 0.9238795325112867385, 1.000000000000000000, 0.9238795325112867385, 1.000000000000000000, 0.9238795325112867385, 1.000000000000000000 ) ) 
 REPRESENTATION_ITEM ( '' )  );
#10029 = CARTESIAN_POINT ( 'NONE',  ( 118.0624999999997868, 2.500000000000054623, 1.035533905932929599 ) ) ;
#10030 = DIRECTION ( 'NONE',  ( -7.147005652999508048E-36, 5.642372883946980038E-36, 1.000000000000000000 ) ) ;
#10031 = CIRCLE ( 'NONE', #27178, 16.00000000000000000 ) ;
#10032 = CARTESIAN_POINT ( 'NONE',  ( -3.175426480542816510, 5.499999999999865885, -127.3750000000000000 ) ) ;
#10033 =( BOUNDED_CURVE ( )  B_SPLINE_CURVE ( 2, ( #3214, #12637, #19822, #24572, #27025, #15238, #3521, #21982, #5671 ),
 .UNSPECIFIED., .F., .T. ) 
 B_SPLINE_CURVE_WITH_KNOTS ( ( 3, 2, 2, 2, 3 ),
 ( 0.3972222222222222543, 0.3981481481481481399, 0.4000000000000000222, 0.4018518518518518490, 0.4027777777777777901 ),
 .UNSPECIFIED. ) 
 CURVE ( )  GEOMETRIC_REPRESENTATION_ITEM ( )  RATIONAL_B_SPLINE_CURVE ( ( 0.9330127018922194093, 0.9330127018922214077, 1.000000000000000000, 0.8660254037844388186, 1.000000000000000000, 0.8660254037844388186, 1.000000000000000000, 0.9330127018922194093, 0.9330127018922194093 ) ) 
 REPRESENTATION_ITEM ( '' )  );
#10034 = VERTEX_POINT ( 'NONE', #21655 ) ;
#10035 = VERTEX_POINT ( 'NONE', #590 ) ;
#10036 = CARTESIAN_POINT ( 'NONE',  ( 4.763139720814407951, -2.749999999999988454, -57.49999999999999289 ) ) ;
#10037 = DIRECTION ( 'NONE',  ( 3.330669073875465184E-16, -0.8660254037844377084, 0.5000000000000016653 ) ) ;
#10038 = CARTESIAN_POINT ( 'NONE',  ( 6.000000000000000888, 1.743066579297358182E-13, -66.66367513459481131 ) ) ;
#10039 = SURFACE_STYLE_FILL_AREA ( #2404 ) ;
#10040 = CARTESIAN_POINT ( 'NONE',  ( -3.608439182435052128, -6.250000000000110134, -82.30801270189228092 ) ) ;
#10041 = CARTESIAN_POINT ( 'NONE',  ( 3.464101615137757051, -5.999999999999979572, -100.8363248654051887 ) ) ;
#10042 = CYLINDRICAL_SURFACE ( 'NONE', #2020, 0.5000000000000004441 ) ;
#10043 = DIRECTION ( 'NONE',  ( 1.000000000000000000, -5.551115123125774690E-17, 0.000000000000000000 ) ) ;
#10044 = DIRECTION ( 'NONE',  ( -1.000000000000000000, -0.000000000000000000, 0.000000000000000000 ) ) ;
#10045 = CARTESIAN_POINT ( 'NONE',  ( 114.8127832217620465, -1.849990392679591977, 0.7662911109078888172 ) ) ;
#10046 = CARTESIAN_POINT ( 'NONE',  ( -3.175426480542816066, -5.500000000000057732, -138.8750000000000568 ) ) ;
#10047 = CARTESIAN_POINT ( 'NONE',  ( 140.3314506832066400, -9.164856574046146065, 7.747256842543193578 ) ) ;
#10048 = CARTESIAN_POINT ( 'NONE',  ( 5.412658773652739619, 3.124999999999988898, -150.6830127018922099 ) ) ;
#10049 = CARTESIAN_POINT ( 'NONE',  ( -5.999999999999963585, -1.487416814333745711E-14, -66.83632486540523132 ) ) ;
#10050 = PRESENTATION_LAYER_ASSIGNMENT (  '', '', ( #8568 ) ) ;
#10051 = EDGE_CURVE ( 'NONE', #26257, #42, #5335, .T. ) ;
#10052 = AXIS2_PLACEMENT_3D ( 'NONE', #21271, #21125, #64 ) ;
#10054 = CARTESIAN_POINT ( 'NONE',  ( -4.763139720814407951, -2.750000000000016431, -73.00000000000001421 ) ) ;
#10053 = AXIS2_PLACEMENT_3D ( 'NONE', #3531, #5837, #8781 ) ;
#10055 = CARTESIAN_POINT ( 'NONE',  ( 3.464101615137852974, 5.999999999999884537, -114.4136751345948255 ) ) ;
#10056 = CARTESIAN_POINT ( 'NONE',  ( -4.763139720814407951, 2.749999999999946709, -56.75000000000002132 ) ) ;
#10057 = CARTESIAN_POINT ( 'NONE',  ( -5.999999999999919176, 1.607695154586804565, -53.40331216351298593 ) ) ;
#10058 = CARTESIAN_POINT ( 'NONE',  ( 144.2023502691896510, 0.000000000000000000, -5.000000000000004441 ) ) ;
#10059 = CARTESIAN_POINT ( 'NONE',  ( 149.8125000000000568, 4.242640687119298093, -4.242640687119298093 ) ) ;
#10060 = CARTESIAN_POINT ( 'NONE',  ( -5.196152422706601826, 2.999999999999975131, -126.9613248654052313 ) ) ;
#10061 = CARTESIAN_POINT ( 'NONE',  ( 17.25000000000001421, 1.665334536937734811E-13, 2.000000000000001776 ) ) ;
#10062 = CARTESIAN_POINT ( 'NONE',  ( 5.196152422706629359, -2.999999999999988898, -104.2886751345948255 ) ) ;
#10063 = CARTESIAN_POINT ( 'NONE',  ( 115.0622167782373850, -1.849990392679411677, 0.7662911109078888172 ) ) ;
#10064 = EDGE_CURVE ( 'NONE', #25253, #22372, #28566, .T. ) ;
#10065 = CARTESIAN_POINT ( 'NONE',  ( 19.99999999999998934, 2.018759447849275454E-15, -6.500000000000000000 ) ) ;
#10066 = ADVANCED_FACE ( 'NONE', ( #29602 ), #17967, .F. ) ;
#10067 = ORIENTED_EDGE ( 'NONE', *, *, #6007, .T. ) ;
#10068 = CARTESIAN_POINT ( 'NONE',  ( 146.8125000000000284, 4.242640687119298093, -4.242640687119298093 ) ) ;
#10069 = VECTOR ( 'NONE', #18164, 1000.000000000000000 ) ;
#10070 = CARTESIAN_POINT ( 'NONE',  ( 104.9172689374427279, 0.2127325526458908322, 1.948528123138198120 ) ) ;
#10071 = CARTESIAN_POINT ( 'NONE',  ( 3.175426480543072749, 5.499999999999865885, -180.1250000000000000 ) ) ;
#10072 = CARTESIAN_POINT ( 'NONE',  ( 22.06250000000015632, 2.000000000000212275, 0.8284271247461753029 ) ) ;
#10073 = ORIENTED_EDGE ( 'NONE', *, *, #6322, .T. ) ;
#10074 = CARTESIAN_POINT ( 'NONE',  ( 3.175426480543072749, -5.500000000000105693, -78.62500000000001421 ) ) ;
#10075 = CARTESIAN_POINT ( 'NONE',  ( -7.216878364870328078, 0.000000000000000000, -100.5580127018922241 ) ) ;
#10076 = ORIENTED_EDGE ( 'NONE', *, *, #3639, .F. ) ;
#10077 = COLOUR_RGB ( '', 0.66274510, 0.83137255, 0.94901961) ;
#10078 = CARTESIAN_POINT ( 'NONE',  ( 6.000000000000000888, 7.762456499804234384E-14, -127.5863248654052171 ) ) ;
#10079 = CARTESIAN_POINT ( 'NONE',  ( -4.763139720814407951, -2.750000000000016431, -167.4999999999999716 ) ) ;
#10080 = CARTESIAN_POINT ( 'NONE',  ( 0.000000000000000000, 0.000000000000000000, 0.000000000000000000 ) ) ;
#10081 = CARTESIAN_POINT ( 'NONE',  ( 4.871333033796958922, -9.863307416503765523, -21.49176472276546690 ) ) ;
#10082 = FACE_OUTER_BOUND ( 'NONE', #22835, .T. ) ;
#10083 =( NAMED_UNIT ( * ) PLANE_ANGLE_UNIT ( ) SI_UNIT ( $, .RADIAN. ) );
#10084 = CARTESIAN_POINT ( 'NONE',  ( 3.175426480543072749, -5.500000000000105693, -164.1249999999999716 ) ) ;
#10085 = CARTESIAN_POINT ( 'NONE',  ( 143.9925748654052313, 2.278174593052043395, 5.499999999999981348 ) ) ;
#10086 = CARTESIAN_POINT ( 'NONE',  ( 3.175426480543072749, 5.499999999999865885, -148.6250000000000284 ) ) ;
#10087 = CARTESIAN_POINT ( 'NONE',  ( 117.1011751345945981, 0.8284271247463257382, -1.999999999999731104 ) ) ;
#10088 = CARTESIAN_POINT ( 'NONE',  ( -5.999999999999963585, -1.487416814333745711E-14, -59.33632486540522422 ) ) ;
#10089 = VECTOR ( 'NONE', #22944, 1000.000000000000000 ) ;
#10090 = EDGE_CURVE ( 'NONE', #29809, #6843, #12128, .T. ) ;
#10091 = CARTESIAN_POINT ( 'NONE',  ( 4.763139720814407951, 2.750000000000002665, -97.75000000000000000 ) ) ;
#10092 = CARTESIAN_POINT ( 'NONE',  ( 115.3511751345947403, 2.000000000000122125, 0.8284271247462955401 ) ) ;
#10093 = EDGE_CURVE ( 'NONE', #30369, #21072, #1298, .T. ) ;
#10094 = CARTESIAN_POINT ( 'NONE',  ( -3.175426480542816510, 5.499999999999865885, -92.87500000000002842 ) ) ;
#10095 = DIRECTION ( 'NONE',  ( 1.000000000000000000, -0.000000000000000000, -0.000000000000000000 ) ) ;
#10096 = LINE ( 'NONE', #19033, #20428 ) ;
#10097 = CARTESIAN_POINT ( 'NONE',  ( 108.8124999999997442, 1.035533905932839449, -2.499999999999964473 ) ) ;
#10098 = DIRECTION ( 'NONE',  ( 1.000000000000000000, 0.000000000000000000, 0.000000000000000000 ) ) ;
#10099 = DIRECTION ( 'NONE',  ( -1.000000000000000000, -6.938893903907221278E-15, -0.000000000000000000 ) ) ;
#10100 = VERTEX_POINT ( 'NONE', #22706 ) ;
#10101 = AXIS2_PLACEMENT_3D ( 'NONE', #23945, #874, #7783 ) ;
#10102 = CARTESIAN_POINT ( 'NONE',  ( 3.464101615137852974, 5.999999999999884537, -178.9136751345947971 ) ) ;
#10103 = CARTESIAN_POINT ( 'NONE',  ( 5.999999999999949374, 1.607695154586804565, -83.09668783648704959 ) ) ;
#10104 = CARTESIAN_POINT ( 'NONE',  ( 119.2502832217621886, 1.308140751793612777, -1.308140751793418488 ) ) ;
#10105 = ORIENTED_EDGE ( 'NONE', *, *, #19056, .T. ) ;
#10106 = CARTESIAN_POINT ( 'NONE',  ( 145.1250000000000284, 0.000000000000000000, -6.000000000000005329 ) ) ;
#10107 = ORIENTED_EDGE ( 'NONE', *, *, #4387, .T. ) ;
#10108 = CIRCLE ( 'NONE', #10620, 0.5000000000000004441 ) ;
#10109 = CARTESIAN_POINT ( 'NONE',  ( 6.350852961086080661, -9.614813431917819062E-14, -102.3750000000000000 ) ) ;
#10110 = CARTESIAN_POINT ( 'NONE',  ( 19.81250000000006750, -2.649519052838178457, 1.097466725451499370 ) ) ;
#10111 = CARTESIAN_POINT ( 'NONE',  ( 5.412658773652712085, -3.125000000000086153, -119.4330127018922099 ) ) ;
#10112 = ORIENTED_EDGE ( 'NONE', *, *, #24317, .T. ) ;
#10113 = CARTESIAN_POINT ( 'NONE',  ( 5.196152422706629359, -2.999999999999988898, -60.78867513459484684 ) ) ;
#10114 = CARTESIAN_POINT ( 'NONE',  ( 2.775557561562891351E-14, -6.250000000000061284, -162.3169872981078470 ) ) ;
#10115 = CARTESIAN_POINT ( 'NONE',  ( 105.7499999999998010, 1.110223024625156540E-13, -2.499999999999946709 ) ) ;
#10116 = CARTESIAN_POINT ( 'NONE',  ( 132.3601497308104342, -3.535533905932725318, -3.535533905932725318 ) ) ;
#10117 = CARTESIAN_POINT ( 'NONE',  ( -7.216878364870328078, 0.000000000000000000, -57.05801270189221697 ) ) ;
#10118 = ORIENTED_EDGE ( 'NONE', *, *, #12141, .T. ) ;
#10119 = CARTESIAN_POINT ( 'NONE',  ( 0.1053031288715393921, -15.23283975038561344, -8.619984219653437307 ) ) ;
#10120 =( BOUNDED_CURVE ( )  B_SPLINE_CURVE ( 2, ( #3230, #10641, #5238, #29037, #930, #14652, #23996, #17108, #8003 ),
 .UNSPECIFIED., .F., .T. ) 
 B_SPLINE_CURVE_WITH_KNOTS ( ( 3, 2, 2, 2, 3 ),
 ( 0.8281250000000000000, 0.8359375000000000000, 0.8437500000000000000, 0.8515625000000000000, 0.8593750000000000000 ),
 .UNSPECIFIED. ) 
 CURVE ( )  GEOMETRIC_REPRESENTATION_ITEM ( )  RATIONAL_B_SPLINE_CURVE ( ( 1.000000000000000000, 0.9238795325112867385, 1.000000000000000000, 0.9238795325112867385, 1.000000000000000000, 0.9238795325112867385, 1.000000000000000000, 0.9238795325112867385, 1.000000000000000000 ) ) 
 REPRESENTATION_ITEM ( '' )  );
#10121 = CARTESIAN_POINT ( 'NONE',  ( 158.3511751345948539, -3.889087296526011706, 3.889087296526011706 ) ) ;
#10122 = SURFACE_SIDE_STYLE ('',( #19059 ) ) ;
#10123 = CARTESIAN_POINT ( 'NONE',  ( 4.763139720814407951, -2.749999999999988454, -168.4999999999999716 ) ) ;
#10124 = CARTESIAN_POINT ( 'NONE',  ( 105.5002832217622313, 1.308140751793696044, 1.308140751793640533 ) ) ;
#10125 = AXIS2_PLACEMENT_3D ( 'NONE', #22102, #10902, #17969 ) ;
#10126 = DIRECTION ( 'NONE',  ( -1.000000000000000000, -1.665334536937736783E-16, -2.220446049250315546E-16 ) ) ;
#10127 = CARTESIAN_POINT ( 'NONE',  ( 3.608439182435180470, -6.249999999999997335, -166.0580127018922099 ) ) ;
#10128 = DIRECTION ( 'NONE',  ( -1.000000000000000000, 0.000000000000000000, 0.000000000000000000 ) ) ;
#10129 = CARTESIAN_POINT ( 'NONE',  ( 23.37500000000000711, -1.414213562373090038, 1.414213562373034527 ) ) ;
#10130 = EDGE_CURVE ( 'NONE', #25655, #1053, #18362, .T. ) ;
#10131 = CARTESIAN_POINT ( 'NONE',  ( -3.175426480542816066, -5.500000000000057732, -119.3750000000000284 ) ) ;
#10132 = CARTESIAN_POINT ( 'NONE',  ( 6.000000000000000888, -1.859271017917181981E-14, -54.66367513459481842 ) ) ;
#10133 = EDGE_CURVE ( 'NONE', #6908, #16270, #23674, .T. ) ;
#10134 = CARTESIAN_POINT ( 'NONE',  ( -2.775557561562891351E-14, -5.500000000000115463, -114.7500000000000142 ) ) ;
#10135 = CARTESIAN_POINT ( 'NONE',  ( -9.999999999999980460, -60.00000000000001421, -3.000000000000002665 ) ) ;
#10136 = ORIENTED_EDGE ( 'NONE', *, *, #25014, .F. ) ;
#10137 = CARTESIAN_POINT ( 'NONE',  ( 17.43750000000009592, 1.097466725451679892, -2.649519052838238409 ) ) ;
#10138 = AXIS2_PLACEMENT_3D ( 'NONE', #27665, #10981, #6489 ) ;
#10139 = CARTESIAN_POINT ( 'NONE',  ( 119.9374999999996874, 2.500000000000114575, -1.035533905932388699 ) ) ;
#10140 = CARTESIAN_POINT ( 'NONE',  ( 6.000000000000000888, 1.607695154586715303, -109.5193375672974270 ) ) ;
#10141 = ORIENTED_EDGE ( 'NONE', *, *, #2860, .T. ) ;
#10142 = SURFACE_STYLE_FILL_AREA ( #756 ) ;
#10143 = CARTESIAN_POINT ( 'NONE',  ( 4.763139720814407951, -2.749999999999988454, -179.0000000000000568 ) ) ;
#10144 = ORIENTED_EDGE ( 'NONE', *, *, #18958, .T. ) ;
#10145 = CARTESIAN_POINT ( 'NONE',  ( 3.464101615137852974, 5.999999999999884537, -144.4136751345947687 ) ) ;
#10146 = VERTEX_POINT ( 'NONE', #11201 ) ;
#10147 = ORIENTED_EDGE ( 'NONE', *, *, #27824, .F. ) ;
#10148 = CARTESIAN_POINT ( 'NONE',  ( 132.1875000000000284, 4.242640687119269671, 4.242640687119298093 ) ) ;
#10149 = CARTESIAN_POINT ( 'NONE',  ( 135.2023502691896510, 0.000000000000000000, -5.000000000000004441 ) ) ;
#10150 = CARTESIAN_POINT ( 'NONE',  ( 10.87499999999996803, 1.414213562373312083, -1.414213562373145550 ) ) ;
#10151 = CARTESIAN_POINT ( 'NONE',  ( 3.608439182435180470, -6.249999999999997335, -129.1919872981078186 ) ) ;
#10152 = CYLINDRICAL_SURFACE ( 'NONE', #24360, 6.000000000000000888 ) ;
#10153 = DIRECTION ( 'NONE',  ( 1.000000000000000000, -5.551115123125773458E-17, -1.260129944081490338E-35 ) ) ;
#10154 = CARTESIAN_POINT ( 'NONE',  ( 17.06250000000001421, 2.000000000000151879, 0.8284271247461753029 ) ) ;
#10155 = CARTESIAN_POINT ( 'NONE',  ( -5.999999999999963585, 1.780251999655701777E-13, -56.33632486540525264 ) ) ;
#10156 = CARTESIAN_POINT ( 'NONE',  ( -5.999999999999963585, -1.487416814333745711E-14, -139.4136751345948255 ) ) ;
#10157 = CARTESIAN_POINT ( 'NONE',  ( 20.53867513459481486, 0.000000000000000000, 2.500000000000002220 ) ) ;
#10158 = CARTESIAN_POINT ( 'NONE',  ( 138.7351497308104058, 3.535533905932725318, -3.535533905932725318 ) ) ;
#10159 = CARTESIAN_POINT ( 'NONE',  ( 137.5238248654052029, 3.889087296526011706, -3.889087296526011706 ) ) ;
#10160 = CARTESIAN_POINT ( 'NONE',  ( 6.000000000000000888, -3.330669073875464691E-16, -7.560779664488942560E-35 ) ) ;
#10161 = FACE_OUTER_BOUND ( 'NONE', #20193, .T. ) ;
#10162 =( NAMED_UNIT ( * ) PLANE_ANGLE_UNIT ( ) SI_UNIT ( $, .RADIAN. ) );
#10163 = CARTESIAN_POINT ( 'NONE',  ( 106.1874999999999147, 1.035533905932839227, 2.500000000000265121 ) ) ;
#10164 = DIRECTION ( 'NONE',  ( -3.469446951953694061E-16, -1.000000000000000000, 0.000000000000000000 ) ) ;
#10165 = AXIS2_PLACEMENT_3D ( 'NONE', #17288, #18052, #20020 ) ;
#10166 = AXIS2_PLACEMENT_3D ( 'NONE', #4142, #20599, #27935 ) ;
#10167 = EDGE_CURVE ( 'NONE', #16117, #9352, #20547, .T. ) ;
#10168 = CARTESIAN_POINT ( 'NONE',  ( 3.175426480543072749, 5.499999999999865885, -141.1250000000000000 ) ) ;
#10169 = CARTESIAN_POINT ( 'NONE',  ( -19.49999999999998224, -25.00000000000010658, 8.000000000000007105 ) ) ;
#10170 = MECHANICAL_DESIGN_GEOMETRIC_PRESENTATION_REPRESENTATION (  '', ( #12176 ), #29766 ) ;
#10171 = ORIENTED_EDGE ( 'NONE', *, *, #16267, .T. ) ;
#10172 = CARTESIAN_POINT ( 'NONE',  ( 3.175426480543072749, 5.499999999999865885, -49.62500000000000000 ) ) ;
#10173 = CARTESIAN_POINT ( 'NONE',  ( 112.7886751345947403, -1.999999999999946265, 0.000000000000000000 ) ) ;
#10174 = ORIENTED_EDGE ( 'NONE', *, *, #28278, .F. ) ;
#10175 = VECTOR ( 'NONE', #13493, 1000.000000000000000 ) ;
#10176 = CARTESIAN_POINT ( 'NONE',  ( 117.2497167782375129, -1.308140751793585022, -1.308140751793640533 ) ) ;
#10177 = FACE_OUTER_BOUND ( 'NONE', #26958, .T. ) ;
#10178 = CARTESIAN_POINT ( 'NONE',  ( -3.608439182435052128, -6.250000000000110134, -99.44198729810781856 ) ) ;
#10179 = CARTESIAN_POINT ( 'NONE',  ( 3.464101615137757051, -5.999999999999979572, -78.33632486540520290 ) ) ;
#10180 = CARTESIAN_POINT ( 'NONE',  ( 115.8124999999997584, 1.035533905932719101, -2.499999999999784173 ) ) ;
#10181 = CARTESIAN_POINT ( 'NONE',  ( -3.464101615137725076, 5.999999999999979572, -77.58632486540523132 ) ) ;
#10182 = VECTOR ( 'NONE', #12392, 1000.000000000000000 ) ;
#10183 = CARTESIAN_POINT ( 'NONE',  ( -3.175426480542816510, 5.499999999999865885, -125.8749999999999858 ) ) ;
#10184 = CARTESIAN_POINT ( 'NONE',  ( 25.18750000000016698, 1.097466725451679892, -2.649519052838298805 ) ) ;
#10185 = EDGE_CURVE ( 'NONE', #24857, #2252, #30103, .T. ) ;
#10186 = ORIENTED_EDGE ( 'NONE', *, *, #15779, .F. ) ;
#10187 = CARTESIAN_POINT ( 'NONE',  ( -5.999999999999963585, 1.780251999655701777E-13, -83.33632486540520290 ) ) ;
#10188 = EDGE_CURVE ( 'NONE', #28549, #12504, #8878, .T. ) ;
#10189 = CARTESIAN_POINT ( 'NONE',  ( -4.763139720814407951, 2.749999999999946709, -53.75000000000002132 ) ) ;
#10190 = CARTESIAN_POINT ( 'NONE',  ( 159.0074251345947971, 2.278174593052136210, -5.499999999999888978 ) ) ;
#10191 = CARTESIAN_POINT ( 'NONE',  ( -3.464101615137757051, -5.999999999999979572, -134.6636751345948539 ) ) ;
#10192 = DIRECTION ( 'NONE',  ( -0.000000000000000000, -0.000000000000000000, -1.000000000000000000 ) ) ;
#10193 = CARTESIAN_POINT ( 'NONE',  ( -5.412658773652684552, -3.125000000000099920, -76.43301270189223828 ) ) ;
#10194 = FACE_OUTER_BOUND ( 'NONE', #25741, .T. ) ;
#10195 = COLOUR_RGB ( '', 0.31764706, 0.68627451, 0.89019608) ;
#10196 = DIRECTION ( 'NONE',  ( -3.845925372767118265E-16, 1.000000000000000000, 8.881784197001258240E-16 ) ) ;
#10197 = CARTESIAN_POINT ( 'NONE',  ( 3.464101615137852974, 5.999999999999884537, -79.91367513459479710 ) ) ;
#10198 = CYLINDRICAL_SURFACE ( 'NONE', #27349, 5.500000000000000000 ) ;
#10199 = CARTESIAN_POINT ( 'NONE',  ( 0.000000000000000000, 0.000000000000000000, 0.000000000000000000 ) ) ;
#10200 = EDGE_CURVE ( 'NONE', #4935, #10891, #22247, .T. ) ;
#10201 = CARTESIAN_POINT ( 'NONE',  ( -3.175426480542816066, -5.500000000000057732, -140.3750000000000568 ) ) ;
#10202 = CARTESIAN_POINT ( 'NONE',  ( 6.000000000000000888, 5.577813053751546416E-15, -177.0863248654052597 ) ) ;
#10203 = CARTESIAN_POINT ( 'NONE',  ( 5.412658773652712085, -3.125000000000086153, -153.9330127018922383 ) ) ;
#10204 = CARTESIAN_POINT ( 'NONE',  ( 3.464101615137757051, -5.999999999999979572, -70.83632486540518869 ) ) ;
#10205 =( NAMED_UNIT ( * ) PLANE_ANGLE_UNIT ( ) SI_UNIT ( $, .RADIAN. ) );
#10206 = CARTESIAN_POINT ( 'NONE',  ( 6.350852961086080661, -9.614813431917819062E-14, -67.87500000000002842 ) ) ;
#10207 = PRESENTATION_LAYER_ASSIGNMENT (  '', '', ( #20483 ) ) ;
#10208 = CARTESIAN_POINT ( 'NONE',  ( 145.3050748654052029, 5.500000000000012434, 2.278174593052012309 ) ) ;
#10209 = CARTESIAN_POINT ( 'NONE',  ( -2.775557561562891351E-14, -5.500000000000115463, -57.75000000000002132 ) ) ;
#10210 =( BOUNDED_CURVE ( )  B_SPLINE_CURVE ( 2, ( #19028, #28635, #21166, #16584, #2556, #28346, #7322, #19165, #4999 ),
 .UNSPECIFIED., .F., .T. ) 
 B_SPLINE_CURVE_WITH_KNOTS ( ( 3, 2, 2, 2, 3 ),
 ( 0.09722222222222220989, 0.09814814814814809552, 0.09999999999999997780, 0.1018518518518518601, 0.1027777777777777457 ),
 .UNSPECIFIED. ) 
 CURVE ( )  GEOMETRIC_REPRESENTATION_ITEM ( )  RATIONAL_B_SPLINE_CURVE ( ( 0.9330127018922194093, 0.9330127018922194093, 1.000000000000000000, 0.8660254037844388186, 1.000000000000000000, 0.8660254037844388186, 1.000000000000000000, 0.9330127018922234061, 0.9330127018922194093 ) ) 
 REPRESENTATION_ITEM ( '' )  );
#10211 =( NAMED_UNIT ( * ) SI_UNIT ( $, .STERADIAN. ) SOLID_ANGLE_UNIT ( ) );
#10212 = EDGE_LOOP ( 'NONE', ( #14967, #26106, #4686, #8644 ) ) ;
#10213 = CARTESIAN_POINT ( 'NONE',  ( 138.5773502691896510, 5.000000000000004441, 0.000000000000000000 ) ) ;
#10214 = CARTESIAN_POINT ( 'NONE',  ( 154.6875000000000284, 4.242640687119269671, 4.242640687119298093 ) ) ;
#10215 = CARTESIAN_POINT ( 'NONE',  ( 135.0000000000000284, -7.311352623425150909, -8.296311145640547835 ) ) ;
#10216 = CARTESIAN_POINT ( 'NONE',  ( 15.43750000000009770, -1.999999999999851674, 0.8284271247462354770 ) ) ;
#10217 = CARTESIAN_POINT ( 'NONE',  ( -5.196152422706573404, -3.000000000000002665, -104.7886751345948397 ) ) ;
#10218 = CARTESIAN_POINT ( 'NONE',  ( 114.9372167782374135, -0.7662911109077987781, 1.849990392679591977 ) ) ;
#10219 =( BOUNDED_CURVE ( )  B_SPLINE_CURVE ( 2, ( #15787, #29392, #25091, #12709, #6057, #8360, #26772, #5738, #8194 ),
 .UNSPECIFIED., .F., .T. ) 
 B_SPLINE_CURVE_WITH_KNOTS ( ( 3, 2, 2, 2, 3 ),
 ( 0.6694444444444443976, 0.6703703703703703942, 0.6722222222222222765, 0.6740740740740740478, 0.6750000000000000444 ),
 .UNSPECIFIED. ) 
 CURVE ( )  GEOMETRIC_REPRESENTATION_ITEM ( )  RATIONAL_B_SPLINE_CURVE ( ( 0.9330127018922194093, 0.9330127018922154125, 1.000000000000000000, 0.8660254037844388186, 1.000000000000000000, 0.8660254037844388186, 1.000000000000000000, 0.9330127018922154125, 0.9330127018922194093 ) ) 
 REPRESENTATION_ITEM ( '' )  );
#10220 = ORIENTED_EDGE ( 'NONE', *, *, #17696, .T. ) ;
#10221 = CARTESIAN_POINT ( 'NONE',  ( 141.7500000000000568, -6.000000000000005329, 0.000000000000000000 ) ) ;
#10222 = VECTOR ( 'NONE', #3153, 1000.000000000000000 ) ;
#10223 = CARTESIAN_POINT ( 'NONE',  ( 104.9999999999999716, -0.4876318259226519736, 1.939643060552054266 ) ) ;
#10224 = CARTESIAN_POINT ( 'NONE',  ( 3.608439182435180470, 6.249999999999982236, -46.19198729810782567 ) ) ;
#10225 = CARTESIAN_POINT ( 'NONE',  ( 18.75000000000015632, 1.110223024625156540E-13, -2.000000000000168310 ) ) ;
#10226 = CARTESIAN_POINT ( 'NONE',  ( 3.608439182435180470, -6.249999999999997335, -153.1919872981078186 ) ) ;
#10227 = FILL_AREA_STYLE ('',( #831 ) ) ;
#10228 = ADVANCED_FACE ( 'NONE', ( #15365 ), #24689, .T. ) ;
#10229 = CARTESIAN_POINT ( 'NONE',  ( 3.175426480543072749, -5.500000000000105693, -84.62499999999998579 ) ) ;
#10230 = CARTESIAN_POINT ( 'NONE',  ( 15.43750000000009770, 2.649519052838538613, 1.097466725451439196 ) ) ;
#10231 = CARTESIAN_POINT ( 'NONE',  ( -7.216878364870328078, 0.000000000000000000, -97.55801270189222407 ) ) ;
#10232 = FACE_OUTER_BOUND ( 'NONE', #7674, .T. ) ;
#10233 = DIRECTION ( 'NONE',  ( 1.000000000000000000, 0.000000000000000000, 0.000000000000000000 ) ) ;
#10234 = CARTESIAN_POINT ( 'NONE',  ( 5.195867772253143890, -9.698547982442518034, -21.97454809331924608 ) ) ;
#10235 =( LENGTH_UNIT ( ) NAMED_UNIT ( * ) SI_UNIT ( .MILLI., .METRE. ) );
#10236 = EDGE_CURVE ( 'NONE', #27584, #5282, #29922, .T. ) ;
#10237 = SHAPE_REPRESENTATION_RELATIONSHIP ( 'NONE' , 'NONE' ,  #1893, #1155 ) ;
#10238 = ADVANCED_FACE ( 'NONE', ( #6715 ), #1957, .T. ) ;
#10239 = CARTESIAN_POINT ( 'NONE',  ( 0.000000000000000000, 5.499999999999991118, -165.0000000000000284 ) ) ;
#10240 = CARTESIAN_POINT ( 'NONE',  ( 143.4300748654052029, 2.278174593051733421, -5.500000000000292211 ) ) ;
#10241 = CARTESIAN_POINT ( 'NONE',  ( 6.350852961086080661, -9.614813431917819062E-14, -144.3750000000000568 ) ) ;
#10242 = LINE ( 'NONE', #19601, #22305 ) ;
#10243 = CARTESIAN_POINT ( 'NONE',  ( 148.8675748654052029, -5.500000000000012434, 2.278174593052012309 ) ) ;
#10244 = B_SPLINE_CURVE_WITH_KNOTS ( 'NONE', 3,
 ( #24818, #15169, #1624, #10553, #12730, #8537 ),
 .UNSPECIFIED., .F., .F.,
 ( 4, 2, 4 ),
 ( 0.000000000000000000, 0.0009324921843552346802, 0.001864984368710469360 ),
 .UNSPECIFIED. ) ;
#10245 = CARTESIAN_POINT ( 'NONE',  ( 0.000000000000000000, 5.499999999999991118, -91.50000000000002842 ) ) ;
#10246 = CARTESIAN_POINT ( 'NONE',  ( -5.196152422706601826, 2.999999999999975131, -125.4613248654052313 ) ) ;
#10247 = CARTESIAN_POINT ( 'NONE',  ( 24.35117513459483263, 2.500000000000144773, 1.035533905932689347 ) ) ;
#10248 = CARTESIAN_POINT ( 'NONE',  ( -3.175426480542816510, 5.499999999999865885, -83.87500000000004263 ) ) ;
#10249 = CARTESIAN_POINT ( 'NONE',  ( 5.196152422706629359, 3.000000000000002665, -143.9613248654052597 ) ) ;
#10250 = CARTESIAN_POINT ( 'NONE',  ( -3.464101615137725076, 5.999999999999979572, -124.6636751345948113 ) ) ;
#10251 = CARTESIAN_POINT ( 'NONE',  ( -3.464101615137757051, -5.999999999999979572, -74.08632486540518869 ) ) ;
#10252 = FACE_OUTER_BOUND ( 'NONE', #7796, .T. ) ;
#10253 = ORIENTED_EDGE ( 'NONE', *, *, #16311, .F. ) ;
#10254 = CARTESIAN_POINT ( 'NONE',  ( 117.7113248654050466, 2.000000000000085265, 0.000000000000000000 ) ) ;
#10255 = CARTESIAN_POINT ( 'NONE',  ( -3.464101615137725076, 5.999999999999979572, -178.6636751345948255 ) ) ;
#10256 = ORIENTED_EDGE ( 'NONE', *, *, #25458, .F. ) ;
#10257 = ORIENTED_EDGE ( 'NONE', *, *, #25965, .F. ) ;
#10258 = VERTEX_POINT ( 'NONE', #25758 ) ;
#10259 = ADVANCED_FACE ( 'NONE', ( #27736 ), #11829, .F. ) ;
#10260 = CARTESIAN_POINT ( 'NONE',  ( 0.000000000000000000, 5.499999999999991118, -107.9999999999999858 ) ) ;
#10261 = CARTESIAN_POINT ( 'NONE',  ( 18.43750000000011724, 2.649519052838478661, 1.097466725451439196 ) ) ;
#10262 = CARTESIAN_POINT ( 'NONE',  ( -3.608439182435115633, 6.249999999999965361, -121.8080127018921957 ) ) ;
#10263 = ORIENTED_EDGE ( 'NONE', *, *, #25014, .T. ) ;
#10264 = CARTESIAN_POINT ( 'NONE',  ( 6.000000000000000888, -1.607695154586752384, -110.2306624327026157 ) ) ;
#10265 = CARTESIAN_POINT ( 'NONE',  ( -3.608439182435052128, -6.250000000000110134, -159.4419872981077617 ) ) ;
#10266 = CARTESIAN_POINT ( 'NONE',  ( 105.9374999999997584, 2.500000000000144773, -1.035533905932568777 ) ) ;
#10267 = CARTESIAN_POINT ( 'NONE',  ( 5.412658773652739619, 3.124999999999988898, -62.18301270189224539 ) ) ;
#10268 = VERTEX_POINT ( 'NONE', #107 ) ;
#10269 = CARTESIAN_POINT ( 'NONE',  ( -0.05510817352033407085, -14.57581869335689007, -8.269855266334088739 ) ) ;
#10270 = EDGE_CURVE ( 'NONE', #16308, #3499, #15249, .T. ) ;
#10271 = CARTESIAN_POINT ( 'NONE',  ( -5.999999999999982236, -1.607695154586700426, -119.8466878364870496 ) ) ;
#10272 = CARTESIAN_POINT ( 'NONE',  ( 0.000000000000000000, 0.000000000000000000, 0.000000000000000000 ) ) ;
#10273 = CARTESIAN_POINT ( 'NONE',  ( 6.000000000000000000, 2.951592740943527306E-14, -160.5863248654052313 ) ) ;
#10274 = CARTESIAN_POINT ( 'NONE',  ( -6.350852961085760029, -1.281975124255709124E-13, -170.6250000000000284 ) ) ;
#10275 = CARTESIAN_POINT ( 'NONE',  ( 120.8749999999998863, 1.767766952966348670, -1.767766952966209892 ) ) ;
#10276 = DIRECTION ( 'NONE',  ( 0.000000000000000000, 0.000000000000000000, 1.000000000000000000 ) ) ;
#10277 = CARTESIAN_POINT ( 'NONE',  ( -3.608439182435052128, -6.250000000000110134, -166.3080127018922667 ) ) ;
#10278 = CARTESIAN_POINT ( 'NONE',  ( 0.000000000000000000, 5.999999999999977796, -48.28867513459483973 ) ) ;
#10279 = CARTESIAN_POINT ( 'NONE',  ( 24.75000000000010658, 1.665334536937734811E-13, -2.000000000000001776 ) ) ;
#10280 = CARTESIAN_POINT ( 'NONE',  ( -6.350852961085760029, -1.281975124255709124E-13, -115.1250000000000000 ) ) ;
#10281 = CARTESIAN_POINT ( 'NONE',  ( 159.6636751345948539, 0.000000000000000000, 5.500000000000005329 ) ) ;
#10282 = CARTESIAN_POINT ( 'NONE',  ( 3.175426480543072749, -5.500000000000105693, -105.6250000000000142 ) ) ;
#10283 = CARTESIAN_POINT ( 'NONE',  ( 149.0699251345948539, 2.278174593052259667, 5.499999999999763745 ) ) ;
#10284 = EDGE_LOOP ( 'NONE', ( #21771, #4983, #5159, #7196 ) ) ;
#10285 = CARTESIAN_POINT ( 'NONE',  ( 135.2246127425879081, -8.380956232050152721, -8.129726081524356829 ) ) ;
#10286 = CARTESIAN_POINT ( 'NONE',  ( -5.196152422706601826, 2.999999999999975131, -86.46132486540525974 ) ) ;
#10287 = ORIENTED_EDGE ( 'NONE', *, *, #18222, .T. ) ;
#10288 = CARTESIAN_POINT ( 'NONE',  ( -3.608439182435115633, 6.249999999999965361, -80.44198729810779014 ) ) ;
#10289 = CIRCLE ( 'NONE', #29871, 0.9999999999999995559 ) ;
#10290 = ORIENTED_EDGE ( 'NONE', *, *, #21025, .F. ) ;
#10291 = DIRECTION ( 'NONE',  ( 0.000000000000000000, 0.000000000000000000, 1.000000000000000000 ) ) ;
#10292 =( BOUNDED_CURVE ( )  B_SPLINE_CURVE ( 2, ( #2933, #19984, #3221, #29177, #21990, #17553, #14935, #22142, #10173 ),
 .UNSPECIFIED., .F., .T. ) 
 B_SPLINE_CURVE_WITH_KNOTS ( ( 3, 2, 2, 2, 3 ),
 ( 0.4411764705882352811, 0.4485294117647058432, 0.4558823529411765163, 0.4632352941176470784, 0.4705882352941176405 ),
 .UNSPECIFIED. ) 
 CURVE ( )  GEOMETRIC_REPRESENTATION_ITEM ( )  RATIONAL_B_SPLINE_CURVE ( ( 1.000000000000000000, 0.9238795325112867385, 1.000000000000000000, 0.9238795325112867385, 1.000000000000000000, 0.9238795325112867385, 1.000000000000000000, 0.9238795325112867385, 1.000000000000000000 ) ) 
 REPRESENTATION_ITEM ( '' )  );
#10293 = VECTOR ( 'NONE', #4217, 1000.000000000000000 ) ;
#10294 = ORIENTED_EDGE ( 'NONE', *, *, #24589, .T. ) ;
#10295 = CARTESIAN_POINT ( 'NONE',  ( 136.0461002691896795, -2.071067811865468400, 4.999999999999989342 ) ) ;
#10296 = ADVANCED_FACE ( 'NONE', ( #16131 ), #6864, .F. ) ;
#10297 = EDGE_CURVE ( 'NONE', #11265, #7855, #24626, .T. ) ;
#10298 =( BOUNDED_CURVE ( )  B_SPLINE_CURVE ( 2, ( #447, #21811, #14903, #19078, #19214, #7804, #7961, #304, #17220 ),
 .UNSPECIFIED., .F., .T. ) 
 B_SPLINE_CURVE_WITH_KNOTS ( ( 3, 2, 2, 2, 3 ),
 ( 0.5305555555555555580, 0.5314814814814814437, 0.5333333333333333259, 0.5351851851851852082, 0.5361111111111110938 ),
 .UNSPECIFIED. ) 
 CURVE ( )  GEOMETRIC_REPRESENTATION_ITEM ( )  RATIONAL_B_SPLINE_CURVE ( ( 0.9330127018922194093, 0.9330127018922194093, 1.000000000000000000, 0.8660254037844388186, 1.000000000000000000, 0.8660254037844388186, 1.000000000000000000, 0.9330127018922234061, 0.9330127018922194093 ) ) 
 REPRESENTATION_ITEM ( '' )  );
#10299 = ORIENTED_EDGE ( 'NONE', *, *, #8019, .T. ) ;
#10300 = CARTESIAN_POINT ( 'NONE',  ( 5.412658773652739619, 3.124999999999988898, -133.3169872981078186 ) ) ;
#10301 = DIRECTION ( 'NONE',  ( -1.000000000000000000, -0.000000000000000000, -0.000000000000000000 ) ) ;
#10302 = CARTESIAN_POINT ( 'NONE',  ( 20.21132486540527751, -2.499999999999835687, -2.220446049250313081E-13 ) ) ;
#10303 = ORIENTED_EDGE ( 'NONE', *, *, #7435, .T. ) ;
#10304 = CARTESIAN_POINT ( 'NONE',  ( 17.12500000000005684, 1.414213562373090038, 1.414213562373201061 ) ) ;
#10305 = CARTESIAN_POINT ( 'NONE',  ( 6.000000000000026645, -1.607695154586707753, -138.7306624327025872 ) ) ;
#10306 = CYLINDRICAL_SURFACE ( 'NONE', #21098, 6.000000000000000888 ) ;
#10307 = CARTESIAN_POINT ( 'NONE',  ( 139.4851497308104058, -3.535533905932725318, 3.535533905932725318 ) ) ;
#10308 = CARTESIAN_POINT ( 'NONE',  ( 137.6175748654052597, 5.500000000000012434, -2.278174593052012309 ) ) ;
#10309 = CARTESIAN_POINT ( 'NONE',  ( 7.216878364870455975, -6.409875621278545621E-14, -65.94198729810784698 ) ) ;
#10310 = CARTESIAN_POINT ( 'NONE',  ( 7.216878364870455975, -6.409875621278545621E-14, -53.94198729810779724 ) ) ;
#10311 = CARTESIAN_POINT ( 'NONE',  ( 6.000000000000000888, 7.762456499804234384E-14, -128.1636751345948539 ) ) ;
#10312 = CARTESIAN_POINT ( 'NONE',  ( 105.5624999999997726, -2.499999999999874767, -1.035533905932568999 ) ) ;
#10313 = CARTESIAN_POINT ( 'NONE',  ( -5.196152422706601826, 2.999999999999975131, -74.46132486540524553 ) ) ;
#10314 = AXIS2_PLACEMENT_3D ( 'NONE', #7161, #18865, #9167 ) ;
#10315 = CARTESIAN_POINT ( 'NONE',  ( -4.763139720814407951, 2.749999999999946709, -140.7500000000000284 ) ) ;
#10316 = STYLED_ITEM ( 'NONE', ( #19733 ), #16057 ) ;
#10317 = EDGE_LOOP ( 'NONE', ( #13545, #9041 ) ) ;
#10318 = SURFACE_STYLE_USAGE ( .BOTH. , #12089 ) ;
#10319 = COLOUR_RGB ( '', 0.66274510, 0.83137255, 0.94901961) ;
#10320 = CARTESIAN_POINT ( 'NONE',  ( -4.763139720814407951, 2.749999999999946709, -50.75000000000001421 ) ) ;
#10321 = DIRECTION ( 'NONE',  ( -1.000000000000000000, -1.067522139062651904E-16, 0.000000000000000000 ) ) ;
#10322 = CYLINDRICAL_SURFACE ( 'NONE', #13950, 30.00000000000000000 ) ;
#10323 = DIRECTION ( 'NONE',  ( 6.938893903907221278E-15, -1.000000000000000000, 0.000000000000000000 ) ) ;
#10324 = ORIENTED_EDGE ( 'NONE', *, *, #6809, .F. ) ;
#10325 = CARTESIAN_POINT ( 'NONE',  ( 112.6872167782374419, 1.849990392679621953, 0.7662911109081291805 ) ) ;
#10326 = CARTESIAN_POINT ( 'NONE',  ( 135.0937500000000284, 5.999999999999970690, 2.485281374238619723 ) ) ;
#10327 = CARTESIAN_POINT ( 'NONE',  ( 11.00000000000014921, 2.000000000000112799, 0.000000000000000000 ) ) ;
#10328 = CARTESIAN_POINT ( 'NONE',  ( -3.608439182435052128, -6.250000000000110134, -93.44198729810786119 ) ) ;
#10329 = CARTESIAN_POINT ( 'NONE',  ( -5.196152422706573404, -3.000000000000002665, -78.71132486540521711 ) ) ;
#10330 = DIRECTION ( 'NONE',  ( -1.000000000000000000, 0.000000000000000000, 0.000000000000000000 ) ) ;
#10331 = CARTESIAN_POINT ( 'NONE',  ( 114.8124999999998010, 1.035533905932749299, -2.499999999999844569 ) ) ;
#10332 = CARTESIAN_POINT ( 'NONE',  ( 19.99999999999998934, 2.220446049250313081E-16, -4.000000000000010658 ) ) ;
#10333 = CARTESIAN_POINT ( 'NONE',  ( 5.196152422706629359, 3.000000000000002665, -77.96132486540518869 ) ) ;
#10334 = COLOUR_RGB ( '', 0.40784314, 0.44705882, 0.49803922) ;
#10335 = ADVANCED_FACE ( 'NONE', ( #26346 ), #19603, .T. ) ;
#10336 = AXIS2_PLACEMENT_3D ( 'NONE', #20207, #27238, #13318 ) ;
#10337 = CARTESIAN_POINT ( 'NONE',  ( 25.12500000000014566, 1.665334536937734811E-13, -2.649519052838333888 ) ) ;
#10338 = ORIENTED_EDGE ( 'NONE', *, *, #18090, .T. ) ;
#10339 = CARTESIAN_POINT ( 'NONE',  ( 4.763139720814407951, -2.749999999999988454, -60.50000000000000000 ) ) ;
#10340 = CARTESIAN_POINT ( 'NONE',  ( -3.464101615137757051, -5.999999999999979572, -51.58632486540522422 ) ) ;
#10341 =( NAMED_UNIT ( * ) PLANE_ANGLE_UNIT ( ) SI_UNIT ( $, .RADIAN. ) );
#10342 = CARTESIAN_POINT ( 'NONE',  ( -3.608439182435052128, -6.250000000000110134, -74.80801270189222407 ) ) ;
#10343 = DIRECTION ( 'NONE',  ( 0.000000000000000000, 0.000000000000000000, -1.000000000000000000 ) ) ;
#10344 = CARTESIAN_POINT ( 'NONE',  ( 156.8288997308103774, 4.999999999999989342, -2.071067811865468400 ) ) ;
#10345 = CARTESIAN_POINT ( 'NONE',  ( -5.999999999999963585, 9.296355089585909904E-15, -168.8363248654052029 ) ) ;
#10346 = CARTESIAN_POINT ( 'NONE',  ( 6.000000000000000888, -1.859271017917181981E-14, -80.16367513459481131 ) ) ;
#10347 = CARTESIAN_POINT ( 'NONE',  ( -9.159339953159387393E-16, 5.637083940101630296E-14, -6.000000000000001776 ) ) ;
#10348 = CARTESIAN_POINT ( 'NONE',  ( -5.196152422706573404, -3.000000000000002665, -94.28867513459482552 ) ) ;
#10349 = CARTESIAN_POINT ( 'NONE',  ( 4.763139720814407951, 2.750000000000002665, -135.2500000000000284 ) ) ;
#10350 = CARTESIAN_POINT ( 'NONE',  ( 0.000000000000000000, 0.000000000000000000, 0.000000000000000000 ) ) ;
#10351 = CARTESIAN_POINT ( 'NONE',  ( 6.000000000000000888, -1.859271017917181981E-14, -170.1636751345948539 ) ) ;
#10352 = CARTESIAN_POINT ( 'NONE',  ( 147.0863248654052313, 0.000000000000000000, 5.500000000000005329 ) ) ;
#10353 = PRESENTATION_LAYER_ASSIGNMENT (  '', '', ( #14770 ) ) ;
#10354 = CARTESIAN_POINT ( 'NONE',  ( -4.763139720814407951, 2.749999999999946709, -70.25000000000002842 ) ) ;
#10355 = CARTESIAN_POINT ( 'NONE',  ( -3.175426480542816510, -5.500000000000057732, -60.87500000000000000 ) ) ;
#10356 = AXIS2_PLACEMENT_3D ( 'NONE', #21911, #22057, #17466 ) ;
#10357 = ORIENTED_EDGE ( 'NONE', *, *, #19213, .T. ) ;
#10358 = CARTESIAN_POINT ( 'NONE',  ( 138.0148502691896510, -3.535533905932725318, -3.535533905932725318 ) ) ;
#10359 = VECTOR ( 'NONE', #1465, 1000.000000000000000 ) ;
#10360 = CARTESIAN_POINT ( 'NONE',  ( 153.1875000000000284, 4.242640687119269671, 4.242640687119298093 ) ) ;
#10361 = CARTESIAN_POINT ( 'NONE',  ( -5.999999999999963585, -1.487416814333745711E-14, -126.8363248654052171 ) ) ;
#10362 = CARTESIAN_POINT ( 'NONE',  ( 16.25000000000009948, 1.665334536937734811E-13, 2.000000000000001776 ) ) ;
#10363 = EDGE_CURVE ( 'NONE', #8247, #17248, #22501, .T. ) ;
#10364 = CARTESIAN_POINT ( 'NONE',  ( 5.196152422706629359, -2.999999999999988898, -57.78867513459484684 ) ) ;
#10365 = ORIENTED_EDGE ( 'NONE', *, *, #22387, .T. ) ;
#10366 = CARTESIAN_POINT ( 'NONE',  ( 145.7812500000000284, 2.485281374238585972, 6.000000000000005329 ) ) ;
#10367 = CARTESIAN_POINT ( 'NONE',  ( 6.000000000000000888, 7.762456499804235646E-14, -140.1636751345948255 ) ) ;
#10368 = CIRCLE ( 'NONE', #10387, 29.00000000000000000 ) ;
#10369 = DIRECTION ( 'NONE',  ( 1.000000000000000000, -5.551115123125773458E-17, -1.260129944081490338E-35 ) ) ;
#10370 = ADVANCED_FACE ( 'NONE', ( #12868 ), #8369, .T. ) ;
#10371 = CARTESIAN_POINT ( 'NONE',  ( 6.350852961086080661, -9.614813431917819062E-14, -180.3750000000000284 ) ) ;
#10372 = CARTESIAN_POINT ( 'NONE',  ( 17.93750000000012434, 2.000000000000091926, -0.8284271247463557142 ) ) ;
#10373 = CARTESIAN_POINT ( 'NONE',  ( 3.608439182435180470, 6.249999999999982236, -146.6919872981078470 ) ) ;
#10374 = CARTESIAN_POINT ( 'NONE',  ( -4.763139720814407951, -2.750000000000016431, -83.50000000000001421 ) ) ;
#10375 = VECTOR ( 'NONE', #1600, 1000.000000000000000 ) ;
#10376 = CARTESIAN_POINT ( 'NONE',  ( -5.412658773652684552, -3.125000000000099920, -92.93301270189225249 ) ) ;
#10377 = ORIENTED_EDGE ( 'NONE', *, *, #14457, .T. ) ;
#10378 = AXIS2_PLACEMENT_3D ( 'NONE', #28747, #10499, #19851 ) ;
#10379 = CARTESIAN_POINT ( 'NONE',  ( 119.9999999999998579, 1.183822024857545507, 1.888846423990942158 ) ) ;
#10380 = SURFACE_STYLE_USAGE ( .BOTH. , #22043 ) ;
#10381 = CARTESIAN_POINT ( 'NONE',  ( -5.196152422706573404, -3.000000000000002665, -151.2886751345948824 ) ) ;
#10382 = CARTESIAN_POINT ( 'NONE',  ( 6.000000000000000888, -1.859271017917181981E-14, -120.0863248654052313 ) ) ;
#10383 = FACE_OUTER_BOUND ( 'NONE', #1020, .T. ) ;
#10384 =( BOUNDED_CURVE ( )  B_SPLINE_CURVE ( 2, ( #21390, #2628, #18952, #5072, #9712, #12049, #322, #14500, #19094 ),
 .UNSPECIFIED., .F., .T. ) 
 B_SPLINE_CURVE_WITH_KNOTS ( ( 3, 2, 2, 2, 3 ),
 ( 0.8972222222222222543, 0.8981481481481481399, 0.9000000000000000222, 0.9018518518518519045, 0.9027777777777777901 ),
 .UNSPECIFIED. ) 
 CURVE ( )  GEOMETRIC_REPRESENTATION_ITEM ( )  RATIONAL_B_SPLINE_CURVE ( ( 0.9330127018922194093, 0.9330127018922234061, 1.000000000000000000, 0.8660254037844388186, 1.000000000000000000, 0.8660254037844388186, 1.000000000000000000, 0.9330127018922194093, 0.9330127018922194093 ) ) 
 REPRESENTATION_ITEM ( '' )  );
#10385 = CARTESIAN_POINT ( 'NONE',  ( -4.763139720814407951, 2.749999999999946709, -164.7500000000000000 ) ) ;
#10386 = DIRECTION ( 'NONE',  ( -7.147005652999508048E-36, 5.642372883946980038E-36, 1.000000000000000000 ) ) ;
#10387 = AXIS2_PLACEMENT_3D ( 'NONE', #17251, #14934, #6911 ) ;
#10388 = CARTESIAN_POINT ( 'NONE',  ( 4.763139720814407951, 2.750000000000002665, -144.2500000000000000 ) ) ;
#10389 = CARTESIAN_POINT ( 'NONE',  ( 135.0000000000000000, 4.598116130853834527, 3.436179909522558251 ) ) ;
#10390 = CARTESIAN_POINT ( 'NONE',  ( 5.196152422706629359, -2.999999999999988898, -92.28867513459482552 ) ) ;
#10391 = AXIS2_PLACEMENT_3D ( 'NONE', #10825, #3556, #26897 ) ;
#10392 = CARTESIAN_POINT ( 'NONE',  ( -3.175426480542816066, -5.500000000000057732, -95.37500000000002842 ) ) ;
#10393 = CARTESIAN_POINT ( 'NONE',  ( 0.000000000000000000, -5.999999999999991118, -130.9613248654052313 ) ) ;
#10394 = CARTESIAN_POINT ( 'NONE',  ( -3.175426480542816510, 5.499999999999865885, -85.37500000000004263 ) ) ;
#10395 = LINE ( 'NONE', #3000, #18773 ) ;
#10396 = CARTESIAN_POINT ( 'NONE',  ( 3.464101615137757051, -5.999999999999979572, -108.3363248654052171 ) ) ;
#10397 = CARTESIAN_POINT ( 'NONE',  ( 0.8631338372297875372, -15.37878787878788067, 8.351220472436777342 ) ) ;
#10398 = CARTESIAN_POINT ( 'NONE',  ( 21.87500000000011724, 1.414213562373201061, -1.414213562373090038 ) ) ;
#10399 = ADVANCED_FACE ( 'NONE', ( #15635 ), #27098, .T. ) ;
#10400 = CARTESIAN_POINT ( 'NONE',  ( 5.196152422706629359, 3.000000000000002665, -128.9613248654052313 ) ) ;
#10401 = CARTESIAN_POINT ( 'NONE',  ( 0.000000000000000000, 5.999999999999977796, -174.2886751345948255 ) ) ;
#10402 = ORIENTED_EDGE ( 'NONE', *, *, #14254, .F. ) ;
#10403 = CARTESIAN_POINT ( 'NONE',  ( 159.2812500000000568, 2.485281374238585972, 6.000000000000005329 ) ) ;
#10404 = CYLINDRICAL_SURFACE ( 'NONE', #21444, 6.000000000000000888 ) ;
#10405 = CARTESIAN_POINT ( 'NONE',  ( -5.999999999999919176, 1.607695154586804565, -82.48066243270260145 ) ) ;
#10406 = CARTESIAN_POINT ( 'NONE',  ( 119.9377832217623023, -1.849990392679501827, -0.7662911109076485650 ) ) ;
#10407 = CARTESIAN_POINT ( 'NONE',  ( -5.999999999999963585, 8.134310703387671600E-14, -116.3363248654052313 ) ) ;
#10408 = EDGE_LOOP ( 'NONE', ( #25282, #5474, #25802, #2325 ) ) ;
#10409 = EDGE_CURVE ( 'NONE', #15581, #13661, #27757, .T. ) ;
#10410 = VERTEX_POINT ( 'NONE', #24488 ) ;
#10411 = AXIS2_PLACEMENT_3D ( 'NONE', #24943, #20049, #3894 ) ;
#10412 = CARTESIAN_POINT ( 'NONE',  ( -6.350852961085760029, -1.281975124255709124E-13, -101.6250000000000000 ) ) ;
#10413 = CARTESIAN_POINT ( 'NONE',  ( -3.608439182435052128, -6.250000000000110134, -115.3080127018922241 ) ) ;
#10414 = ORIENTED_EDGE ( 'NONE', *, *, #27826, .T. ) ;
#10415 = CARTESIAN_POINT ( 'NONE',  ( 159.6636751345948539, 0.000000000000000000, 5.500000000000005329 ) ) ;
#10416 = CARTESIAN_POINT ( 'NONE',  ( -3.608439182435115633, 6.249999999999965361, -161.4419872981077901 ) ) ;
#10417 = CARTESIAN_POINT ( 'NONE',  ( 105.2499999999999147, -2.775557561562891351E-14, 2.499999999999946709 ) ) ;
#10418 = CARTESIAN_POINT ( 'NONE',  ( -5.412658773652739619, 3.124999999999975131, -58.68301270189224539 ) ) ;
#10419 = VERTEX_POINT ( 'NONE', #22667 ) ;
#10420 = CARTESIAN_POINT ( 'NONE',  ( 0.1257737839961825255, -15.26928397096460266, -8.555325078616231593 ) ) ;
#10421 = CARTESIAN_POINT ( 'NONE',  ( 116.2886751345946124, 2.000000000000168310, 3.330669073875469621E-13 ) ) ;
#10422 = CARTESIAN_POINT ( 'NONE',  ( 13.99999999999999822, 2.143131898507868643E-15, -17.50000000000000355 ) ) ;
#10423 = CARTESIAN_POINT ( 'NONE',  ( 118.7113248654050750, 1.999999999999946265, 1.110223024625156540E-13 ) ) ;
#10424 = CARTESIAN_POINT ( 'NONE',  ( 4.763139720814407951, 2.750000000000002665, -171.2500000000000000 ) ) ;
#10425 = CARTESIAN_POINT ( 'NONE',  ( 105.0002832217622029, -1.308140751793612777, -1.308140751793640533 ) ) ;
#10426 = CIRCLE ( 'NONE', #19269, 17.50000000000000355 ) ;
#10427 = CARTESIAN_POINT ( 'NONE',  ( 152.6175748654052029, 5.500000000000012434, -2.278174593052012309 ) ) ;
#10428 = CARTESIAN_POINT ( 'NONE',  ( -3.608439182435115633, 6.249999999999965361, -171.3080127018922383 ) ) ;
#10429 = B_SPLINE_CURVE_WITH_KNOTS ( 'NONE', 3,
 ( #27009, #19808, #26410, #17378 ),
 .UNSPECIFIED., .F., .F.,
 ( 4, 4 ),
 ( 0.000000000000000000, 0.0005217984816236547699 ),
 .UNSPECIFIED. ) ;
#10430 = CARTESIAN_POINT ( 'NONE',  ( -0.6001665993698097612, -9.799666801260405791, 4.385453238887307315 ) ) ;
#10431 = CARTESIAN_POINT ( 'NONE',  ( 24.25000000000018829, 1.110223024625156540E-13, 2.000000000000001776 ) ) ;
#10432 = CARTESIAN_POINT ( 'NONE',  ( 4.763139720814407951, 2.750000000000002665, -112.7500000000000142 ) ) ;
#10433 = CARTESIAN_POINT ( 'NONE',  ( 135.0000000000000284, -6.982120021884474781, 8.500000000000007105 ) ) ;
#10434 = CARTESIAN_POINT ( 'NONE',  ( 6.350852961086080661, -9.614813431917819062E-14, -102.3750000000000000 ) ) ;
#10435 = CARTESIAN_POINT ( 'NONE',  ( 6.000000000000000888, -1.859271017917181981E-14, -145.5863248654052029 ) ) ;
#10436 = ORIENTED_EDGE ( 'NONE', *, *, #26499, .F. ) ;
#10437 = CARTESIAN_POINT ( 'NONE',  ( 119.4374999999997868, -2.499999999999994671, 1.035533905932809473 ) ) ;
#10438 = EDGE_CURVE ( 'NONE', #11662, #4075, #2134, .T. ) ;
#10439 = FACE_OUTER_BOUND ( 'NONE', #8272, .T. ) ;
#10440 = ORIENTED_EDGE ( 'NONE', *, *, #30191, .T. ) ;
#10441 = CARTESIAN_POINT ( 'NONE',  ( -4.763139720814407951, 2.749999999999946709, -160.2500000000000000 ) ) ;
#10442 = CARTESIAN_POINT ( 'NONE',  ( 2.775557561562891351E-14, -6.250000000000061284, -81.31698729810781856 ) ) ;
#10443 = DIRECTION ( 'NONE',  ( 1.000000000000000000, -0.000000000000000000, -0.000000000000000000 ) ) ;
#10444 = VERTEX_POINT ( 'NONE', #20053 ) ;
#10445 = EDGE_CURVE ( 'NONE', #22536, #18017, #497, .T. ) ;
#10446 = DIRECTION ( 'NONE',  ( 6.938893903907221278E-15, 1.000000000000000000, -0.000000000000000000 ) ) ;
#10447 = VERTEX_POINT ( 'NONE', #25719 ) ;
#10448 = ORIENTED_EDGE ( 'NONE', *, *, #26299, .F. ) ;
#10449 = CARTESIAN_POINT ( 'NONE',  ( 135.4836002691896510, 4.999999999999989342, -2.071067811865468400 ) ) ;
#10450 = CARTESIAN_POINT ( 'NONE',  ( -5.412658773652684552, -3.125000000000099920, -142.4330127018922383 ) ) ;
#10451 = ORIENTED_EDGE ( 'NONE', *, *, #28736, .T. ) ;
#10452 = CARTESIAN_POINT ( 'NONE',  ( -3.608439182435052128, -6.250000000000110134, -135.4419872981078186 ) ) ;
#10453 = SURFACE_STYLE_USAGE ( .BOTH. , #15391 ) ;
#10454 = CARTESIAN_POINT ( 'NONE',  ( -5.999999999999919176, 1.607695154586804565, -49.48066243270260856 ) ) ;
#10455 = DIRECTION ( 'NONE',  ( 0.000000000000000000, 0.000000000000000000, 1.000000000000000000 ) ) ;
#10456 = VERTEX_POINT ( 'NONE', #3109 ) ;
#10457 = CARTESIAN_POINT ( 'NONE',  ( 14.43750000000014033, -1.999999999999851674, 0.8284271247462955401 ) ) ;
#10458 = CARTESIAN_POINT ( 'NONE',  ( 0.9172299446477815144, -15.89788423467024181, -7.323522863575444575 ) ) ;
#10459 = CARTESIAN_POINT ( 'NONE',  ( 149.4449251345948539, -5.500000000000012434, 2.278174593052012309 ) ) ;
#10460 = CARTESIAN_POINT ( 'NONE',  ( 6.000000000000000888, 5.577813053751546416E-15, -165.6636751345948255 ) ) ;
#10461 = CARTESIAN_POINT ( 'NONE',  ( 139.5863248654052313, 0.000000000000000000, 5.500000000000005329 ) ) ;
#10462 = CARTESIAN_POINT ( 'NONE',  ( 8.673617379884035472E-16, -14.99923475244192339, -9.015151515151522688 ) ) ;
#10463 = CARTESIAN_POINT ( 'NONE',  ( -5.412658773652684552, -3.125000000000099920, -65.06698729810783277 ) ) ;
#10464 = CARTESIAN_POINT ( 'NONE',  ( 3.608439182435180470, -6.249999999999997335, -51.19198729810784698 ) ) ;
#10465 = DIRECTION ( 'NONE',  ( 1.000000000000000000, -0.000000000000000000, -0.000000000000000000 ) ) ;
#10466 = CARTESIAN_POINT ( 'NONE',  ( 135.0000000000000000, 3.026753582206697324, 4.706811043600045430 ) ) ;
#10467 = CARTESIAN_POINT ( 'NONE',  ( 119.9999999999998010, 0.1805100831798492900, -2.088914846013065318 ) ) ;
#10468 = CARTESIAN_POINT ( 'NONE',  ( -15.49999999999999289, -54.99999999999990763, -7.500000000000007105 ) ) ;
#10469 = CARTESIAN_POINT ( 'NONE',  ( 4.763139720814407951, -2.749999999999988454, -128.0000000000000000 ) ) ;
#10470 = TOROIDAL_SURFACE ( 'NONE', #7988, 2.000000000000000000, 1.000000000000000000 ) ;
#10471 = CARTESIAN_POINT ( 'NONE',  ( -3.464101615137725076, 5.999999999999979572, -166.6636751345947971 ) ) ;
#10472 = EDGE_LOOP ( 'NONE', ( #19217, #17329, #30253, #28552 ) ) ;
#10473 = LINE ( 'NONE', #15411, #12204 ) ;
#10474 = EDGE_CURVE ( 'NONE', #20437, #9337, #29741, .T. ) ;
#10475 = DIRECTION ( 'NONE',  ( -1.000000000000000000, -1.665334536937736783E-16, -2.220446049250315546E-16 ) ) ;
#10476 = CARTESIAN_POINT ( 'NONE',  ( 153.7425748654052029, -2.278174593052213481, -5.499999999999811706 ) ) ;
#10477 =( BOUNDED_CURVE ( )  B_SPLINE_CURVE ( 2, ( #4569, #9340, #8460, #6873, #20868, #4258, #18274, #23019, #30064 ),
 .UNSPECIFIED., .F., .T. ) 
 B_SPLINE_CURVE_WITH_KNOTS ( ( 3, 2, 2, 2, 3 ),
 ( 0.7343750000000000000, 0.7421875000000000000, 0.7500000000000000000, 0.7578125000000000000, 0.7656250000000000000 ),
 .UNSPECIFIED. ) 
 CURVE ( )  GEOMETRIC_REPRESENTATION_ITEM ( )  RATIONAL_B_SPLINE_CURVE ( ( 1.000000000000000000, 0.9238795325112867385, 1.000000000000000000, 0.9238795325112867385, 1.000000000000000000, 0.9238795325112867385, 1.000000000000000000, 0.9238795325112867385, 1.000000000000000000 ) ) 
 REPRESENTATION_ITEM ( '' )  );
#10478 = EDGE_CURVE ( 'NONE', #21171, #14517, #6787, .T. ) ;
#10479 = CARTESIAN_POINT ( 'NONE',  ( 104.9470444944719532, -1.248719657643215575, -1.538360625296347095 ) ) ;
#10480 =( GEOMETRIC_REPRESENTATION_CONTEXT ( 3 ) GLOBAL_UNCERTAINTY_ASSIGNED_CONTEXT ( ( #7558 ) ) GLOBAL_UNIT_ASSIGNED_CONTEXT ( ( #7899, #7598, #699 ) ) REPRESENTATION_CONTEXT ( 'NONE', 'WORKASPACE' ) );
#10481 = ORIENTED_EDGE ( 'NONE', *, *, #5311, .T. ) ;
#10482 = PRODUCT_DEFINITION ( 'UNKNOWN', '', #14906, #5097 ) ;
#10483 = CARTESIAN_POINT ( 'NONE',  ( 114.8747167782375840, -5.551115123125782702E-14, 1.849990392679523588 ) ) ;
#10484 = CARTESIAN_POINT ( 'NONE',  ( 10.37500000000005151, -1.414213562373034527, 1.414213562372756972 ) ) ;
#10485 = CARTESIAN_POINT ( 'NONE',  ( -5.412658773652684552, -3.125000000000099920, -96.56698729810780435 ) ) ;
#10486 = CARTESIAN_POINT ( 'NONE',  ( 6.000000000000000888, 1.607695154586715303, -173.0966878364870354 ) ) ;
#10487 =( BOUNDED_CURVE ( )  B_SPLINE_CURVE ( 2, ( #1093, #2939, #24433, #17409, #26435, #28729, #12356, #21706, #644 ),
 .UNSPECIFIED., .F., .T. ) 
 B_SPLINE_CURVE_WITH_KNOTS ( ( 3, 2, 2, 2, 3 ),
 ( 0.2343750000000000000, 0.2421875000000000000, 0.2500000000000000000, 0.2578125000000000000, 0.2656250000000000000 ),
 .UNSPECIFIED. ) 
 CURVE ( )  GEOMETRIC_REPRESENTATION_ITEM ( )  RATIONAL_B_SPLINE_CURVE ( ( 1.000000000000000000, 0.9238795325112867385, 1.000000000000000000, 0.9238795325112867385, 1.000000000000000000, 0.9238795325112867385, 1.000000000000000000, 0.9238795325112867385, 1.000000000000000000 ) ) 
 REPRESENTATION_ITEM ( '' )  );
#10488 = DIRECTION ( 'NONE',  ( 1.000000000000000000, -0.000000000000000000, -0.000000000000000000 ) ) ;
#10489 = CARTESIAN_POINT ( 'NONE',  ( 112.5624999999998010, -2.499999999999994671, -1.035533905932689347 ) ) ;
#10490 = CARTESIAN_POINT ( 'NONE',  ( 140.5573082070725377, -11.11461641399629663, 4.524920606408917578 ) ) ;
#10491 = ORIENTED_EDGE ( 'NONE', *, *, #17559, .F. ) ;
#10492 = CARTESIAN_POINT ( 'NONE',  ( 10.43750000000004619, -1.999999999999851674, 0.8284271247461753029 ) ) ;
#10493 = CARTESIAN_POINT ( 'NONE',  ( 161.0000000000000568, -11.64610661123979440, 2.895702980449532227 ) ) ;
#10494 = CARTESIAN_POINT ( 'NONE',  ( 0.000000000000000000, 5.499999999999991118, -48.00000000000004263 ) ) ;
#10495 = CARTESIAN_POINT ( 'NONE',  ( 6.000000000000052403, -1.607695154586662678, -51.15331216351301435 ) ) ;
#10496 = CARTESIAN_POINT ( 'NONE',  ( 2.775557561562891351E-14, -6.250000000000061284, -77.68301270189226670 ) ) ;
#10497 = CARTESIAN_POINT ( 'NONE',  ( 150.5476497308104058, 0.000000000000000000, -5.000000000000004441 ) ) ;
#10498 = CARTESIAN_POINT ( 'NONE',  ( -5.999999999999963585, 8.134310703387671600E-14, -141.8363248654052029 ) ) ;
#10499 = DIRECTION ( 'NONE',  ( -1.000000000000000000, -1.665334536937736783E-16, -2.220446049250315546E-16 ) ) ;
#10500 = PRESENTATION_STYLE_ASSIGNMENT (( #19852 ) ) ;
#10501 = CARTESIAN_POINT ( 'NONE',  ( 135.1658987231415097, -8.213333715523679857, 8.175427762257710285 ) ) ;
#10502 = CARTESIAN_POINT ( 'NONE',  ( -3.175426480542816066, -5.500000000000057732, -128.3750000000000000 ) ) ;
#10503 = CARTESIAN_POINT ( 'NONE',  ( 104.7401757384973280, -1.849990392679412565, 2.220446049250313081E-13 ) ) ;
#10504 = CARTESIAN_POINT ( 'NONE',  ( -3.608439182435052128, -6.250000000000110134, -148.3080127018922667 ) ) ;
#10505 = CARTESIAN_POINT ( 'NONE',  ( -5.999999999999962697, 3.323446944526963260E-14, -158.3363248654052313 ) ) ;
#10506 = CARTESIAN_POINT ( 'NONE',  ( 0.000000000000000000, 5.499999999999991118, -64.50000000000000000 ) ) ;
#10507 = CARTESIAN_POINT ( 'NONE',  ( -3.175426480542816510, -5.500000000000057732, -56.37500000000004263 ) ) ;
#10508 = EDGE_CURVE ( 'NONE', #14874, #19083, #13117, .T. ) ;
#10509 =( NAMED_UNIT ( * ) PLANE_ANGLE_UNIT ( ) SI_UNIT ( $, .RADIAN. ) );
#10510 = ORIENTED_EDGE ( 'NONE', *, *, #8328, .T. ) ;
#10511 = CARTESIAN_POINT ( 'NONE',  ( 151.7812500000000284, 2.485281374238585972, 6.000000000000005329 ) ) ;
#10512 = CARTESIAN_POINT ( 'NONE',  ( 6.000000000000026645, -1.607695154586707753, -117.7306624327026299 ) ) ;
#10513 = CARTESIAN_POINT ( 'NONE',  ( 16.00000000000007105, 2.000000000000223821, -5.551115123125782702E-14 ) ) ;
#10514 = STYLED_ITEM ( 'NONE', ( #3847 ), #9 ) ;
#10515 = CARTESIAN_POINT ( 'NONE',  ( 0.000000000000000000, -5.999999999999991118, -58.03867513459481842 ) ) ;
#10516 = CARTESIAN_POINT ( 'NONE',  ( 112.3747167782374703, -5.551115123125782702E-14, -1.849990392679523588 ) ) ;
#10517 = ORIENTED_EDGE ( 'NONE', *, *, #18961, .F. ) ;
#10518 = CARTESIAN_POINT ( 'NONE',  ( 143.3437500000000284, -6.000000000000005329, -2.485281374238555774 ) ) ;
#10519 = CARTESIAN_POINT ( 'NONE',  ( 161.2977071193381846, -5.560427160162643823, 1.671920971621268182 ) ) ;
#10520 = ORIENTED_EDGE ( 'NONE', *, *, #27812, .T. ) ;
#10521 = CARTESIAN_POINT ( 'NONE',  ( 4.763139720814407951, -2.749999999999988454, -147.5000000000000284 ) ) ;
#10522 = CARTESIAN_POINT ( 'NONE',  ( 7.216878364870455975, -6.409875621278545621E-14, -49.44198729810784698 ) ) ;
#10523 = CARTESIAN_POINT ( 'NONE',  ( 15.25000000000012434, 1.110223024625156540E-13, 1.999999999999946265 ) ) ;
#10524 = ORIENTED_EDGE ( 'NONE', *, *, #7774, .F. ) ;
#10525 = CARTESIAN_POINT ( 'NONE',  ( -5.412658773652739619, 3.124999999999975131, -146.3169872981078186 ) ) ;
#10526 = CARTESIAN_POINT ( 'NONE',  ( 0.000000000000000000, 5.499999999999991118, -70.50000000000000000 ) ) ;
#10527 = CARTESIAN_POINT ( 'NONE',  ( 13.50000000000006750, 1.873492889145123019, 1.873492889144734441 ) ) ;
#10528 = CARTESIAN_POINT ( 'NONE',  ( -3.608439182435115633, 6.249999999999965361, -91.80801270189225249 ) ) ;
#10529 = CARTESIAN_POINT ( 'NONE',  ( -19.99999999999998224, -54.99999999999990763, -5.000000000000004441 ) ) ;
#10530 = ADVANCED_FACE ( 'NONE', ( #953 ), #23247, .T. ) ;
#10531 = CYLINDRICAL_SURFACE ( 'NONE', #4420, 2.499999999999999112 ) ;
#10532 = CARTESIAN_POINT ( 'NONE',  ( 2.081668171172167281E-16, 3.582034040661430693E-16, -2.499999999999999112 ) ) ;
#10533 = LINE ( 'NONE', #3889, #30393 ) ;
#10534 = FACE_OUTER_BOUND ( 'NONE', #5930, .T. ) ;
#10535 = FILL_AREA_STYLE_COLOUR ( '', #18326 ) ;
#10536 = CARTESIAN_POINT ( 'NONE',  ( 6.350852961086080661, -9.614813431917819062E-14, -156.3750000000000000 ) ) ;
#10537 = FACE_OUTER_BOUND ( 'NONE', #24066, .T. ) ;
#10538 = CARTESIAN_POINT ( 'NONE',  ( -3.175426480542816510, 5.499999999999865885, -143.8750000000000000 ) ) ;
#10539 = CARTESIAN_POINT ( 'NONE',  ( 135.0000000000000000, 5.980918879946599098, 0.2920434870148253537 ) ) ;
#10540 = CARTESIAN_POINT ( 'NONE',  ( 6.000000000000052403, -1.607695154586662678, -92.23066243270260145 ) ) ;
#10541 = CARTESIAN_POINT ( 'NONE',  ( 4.763139720814407951, 2.750000000000002665, -90.25000000000005684 ) ) ;
#10542 = CARTESIAN_POINT ( 'NONE',  ( 6.000000000000000888, 1.743066579297358182E-13, -66.08632486540521711 ) ) ;
#10543 = CARTESIAN_POINT ( 'NONE',  ( -6.350852961085760029, -1.281975124255709124E-13, -77.62500000000001421 ) ) ;
#10544 = ADVANCED_FACE ( 'NONE', ( #3867 ), #22326, .T. ) ;
#10545 = CARTESIAN_POINT ( 'NONE',  ( 152.6398502691896510, -3.535533905932752852, 3.535533905932725318 ) ) ;
#10546 = CARTESIAN_POINT ( 'NONE',  ( 161.1742592625232930, -5.078550059815297502, -2.565790349115546931 ) ) ;
#10547 = CARTESIAN_POINT ( 'NONE',  ( 6.000000000000000888, -1.859271017917181981E-14, -109.5863248654052029 ) ) ;
#10548 = CARTESIAN_POINT ( 'NONE',  ( -5.999999999999963585, 1.780251999655701777E-13, -98.33632486540520290 ) ) ;
#10549 = CARTESIAN_POINT ( 'NONE',  ( 6.000000000000000888, 1.607695154586715303, -135.0193375672974412 ) ) ;
#10550 = CARTESIAN_POINT ( 'NONE',  ( 6.000000000000001776, 5.345404176511898156E-15, -174.6636751345948539 ) ) ;
#10551 = ORIENTED_EDGE ( 'NONE', *, *, #24519, .T. ) ;
#10552 = CARTESIAN_POINT ( 'NONE',  ( 161.8125000000000284, 4.242640687119298093, -4.242640687119298093 ) ) ;
#10553 = CARTESIAN_POINT ( 'NONE',  ( -0.02670840214258772202, -15.33233796376583946, 6.888541525869519511 ) ) ;
#10554 = DIRECTION ( 'NONE',  ( -7.147005652999508048E-36, 5.642372883946980038E-36, 1.000000000000000000 ) ) ;
#10555 = CARTESIAN_POINT ( 'NONE',  ( 120.0627832217621602, -0.7662911109077388261, -1.849990392679291551 ) ) ;
#10556 = CARTESIAN_POINT ( 'NONE',  ( 24.90641467890419847, 1.251337131507474831, -1.683925187308909832 ) ) ;
#10557 = ORIENTED_EDGE ( 'NONE', *, *, #3195, .T. ) ;
#10558 = ORIENTED_EDGE ( 'NONE', *, *, #20957, .T. ) ;
#10559 = CARTESIAN_POINT ( 'NONE',  ( 0.000000000000000000, 5.499999999999991118, -106.5000000000000426 ) ) ;
#10560 = CARTESIAN_POINT ( 'NONE',  ( 16.31250000000002487, 2.649519052838298805, -1.097466725451499370 ) ) ;
#10561 = CARTESIAN_POINT ( 'NONE',  ( 160.0000000000000284, -11.67610212985248097, 2.769230769230771827 ) ) ;
#10562 =( BOUNDED_CURVE ( )  B_SPLINE_CURVE ( 2, ( #10746, #1793, #11042, #1171, #17965, #17651, #29434, #17813, #27133 ),
 .UNSPECIFIED., .F., .T. ) 
 B_SPLINE_CURVE_WITH_KNOTS ( ( 3, 2, 2, 2, 3 ),
 ( 0.8906250000000000000, 0.8984375000000000000, 0.9062500000000000000, 0.9140625000000000000, 0.9194088329326726150 ),
 .UNSPECIFIED. ) 
 CURVE ( )  GEOMETRIC_REPRESENTATION_ITEM ( )  RATIONAL_B_SPLINE_CURVE ( ( 1.000000000000000000, 0.9238795325112867385, 1.000000000000000000, 0.9238795325112867385, 1.000000000000000000, 0.9238795325112867385, 1.000000000000000000, 0.9479084336402761046, 0.9671125746068864881 ) ) 
 REPRESENTATION_ITEM ( '' )  );
#10563 = CARTESIAN_POINT ( 'NONE',  ( 5.412658773652712085, -3.125000000000086153, -117.9330127018922667 ) ) ;
#10564 = VERTEX_POINT ( 'NONE', #17739 ) ;
#10565 = CARTESIAN_POINT ( 'NONE',  ( 19.53867513459495342, 5.551115123125782702E-14, 2.500000000000002220 ) ) ;
#10566 = CARTESIAN_POINT ( 'NONE',  ( 105.8749999999999574, 1.767766952966320915, -1.767766952966320915 ) ) ;
#10567 = EDGE_CURVE ( 'NONE', #29332, #23925, #17431, .T. ) ;
#10568 = CARTESIAN_POINT ( 'NONE',  ( 21.03867513459492500, 1.665334536937734811E-13, -2.500000000000002220 ) ) ;
#10569 = AXIS2_PLACEMENT_3D ( 'NONE', #29755, #18121, #1498 ) ;
#10570 = ADVANCED_FACE ( 'NONE', ( #15447 ), #27365, .F. ) ;
#10571 = CARTESIAN_POINT ( 'NONE',  ( 5.412658773652712085, -3.125000000000086153, -50.43301270189226670 ) ) ;
#10572 = ORIENTED_EDGE ( 'NONE', *, *, #20324, .T. ) ;
#10573 = CARTESIAN_POINT ( 'NONE',  ( -5.196152422706601826, 2.999999999999975131, -167.4613248654052029 ) ) ;
#10574 = CARTESIAN_POINT ( 'NONE',  ( 0.000000000000000000, -5.999999999999991118, -56.53867513459481842 ) ) ;
#10575 = CARTESIAN_POINT ( 'NONE',  ( 6.000000000000052403, -1.607695154586662678, -61.65331216351297883 ) ) ;
#10576 = CARTESIAN_POINT ( 'NONE',  ( 118.8363248654051176, 1.414213562373034527, 1.414213562373256572 ) ) ;
#10577 = CARTESIAN_POINT ( 'NONE',  ( 4.763139720814407951, 2.750000000000002665, -174.2500000000000284 ) ) ;
#10578 = CARTESIAN_POINT ( 'NONE',  ( 119.6249999999999716, -1.767766952966404181, -1.767766952966320915 ) ) ;
#10579 = CARTESIAN_POINT ( 'NONE',  ( -5.196152422706601826, 2.999999999999975131, -107.4613248654052171 ) ) ;
#10580 = CARTESIAN_POINT ( 'NONE',  ( 2.775557561562891351E-14, 6.250000000000033751, -168.4330127018922667 ) ) ;
#10581 = CARTESIAN_POINT ( 'NONE',  ( -9.757819552369539906E-16, -9.499999999869134015, 4.869076758059749821 ) ) ;
#10582 = AXIS2_PLACEMENT_3D ( 'NONE', #24357, #8541, #15653 ) ;
#10583 = CARTESIAN_POINT ( 'NONE',  ( -3.175426480542816066, -5.500000000000057732, -114.8749999999999858 ) ) ;
#10584 = CARTESIAN_POINT ( 'NONE',  ( 13.16367513459484861, 1.767766952966431937, -1.767766952966709493 ) ) ;
#10585 = EDGE_CURVE ( 'NONE', #29768, #23369, #16262, .T. ) ;
#10586 = CARTESIAN_POINT ( 'NONE',  ( 6.350852961086080661, -9.614813431917819062E-14, -106.8750000000000142 ) ) ;
#10587 = CARTESIAN_POINT ( 'NONE',  ( -5.196152422706601826, 2.999999999999975131, -142.5386751345948255 ) ) ;
#10588 = FILL_AREA_STYLE_COLOUR ( '', #21094 ) ;
#10589 = CARTESIAN_POINT ( 'NONE',  ( 135.0000000000000284, -9.047800747817843714, 7.999999999999092282 ) ) ;
#10590 = ORIENTED_EDGE ( 'NONE', *, *, #24396, .T. ) ;
#10591 = CARTESIAN_POINT ( 'NONE',  ( 13.56250000000003375, 2.649519052838358757, -1.097466725451559322 ) ) ;
#10592 = CARTESIAN_POINT ( 'NONE',  ( 120.2499999999998721, -2.775557561562891351E-14, 2.500000000000168754 ) ) ;
#10593 = CARTESIAN_POINT ( 'NONE',  ( 107.8363248654051034, 1.414213562373117794, 1.414213562373256572 ) ) ;
#10594 = CARTESIAN_POINT ( 'NONE',  ( -6.000000000000007105, -1.607695154586655129, -146.2693375672974412 ) ) ;
#10595 = ORIENTED_EDGE ( 'NONE', *, *, #27230, .F. ) ;
#10596 = CARTESIAN_POINT ( 'NONE',  ( 6.000000000000000888, 1.743066579297358182E-13, -66.08632486540521711 ) ) ;
#10597 = CARTESIAN_POINT ( 'NONE',  ( -5.412658773652684552, -3.125000000000099920, -78.56698729810784698 ) ) ;
#10598 = CARTESIAN_POINT ( 'NONE',  ( 135.5000000000000000, -9.047800747817552391, 8.000000000000007105 ) ) ;
#10599 = ORIENTED_EDGE ( 'NONE', *, *, #14582, .T. ) ;
#10600 = CARTESIAN_POINT ( 'NONE',  ( 107.1488248654049897, -1.999999999999911626, 0.8284271247464157772 ) ) ;
#10601 = ORIENTED_EDGE ( 'NONE', *, *, #7803, .T. ) ;
#10602 = CARTESIAN_POINT ( 'NONE',  ( 154.8750000000000284, 0.000000000000000000, 6.000000000000005329 ) ) ;
#10603 = CARTESIAN_POINT ( 'NONE',  ( 5.412658773652712085, -3.125000000000086153, -140.4330127018922383 ) ) ;
#10604 = ORIENTED_EDGE ( 'NONE', *, *, #2118, .T. ) ;
#10605 = CARTESIAN_POINT ( 'NONE',  ( 5.412658773652712085, -3.125000000000086153, -124.5669872981078328 ) ) ;
#10606 = CARTESIAN_POINT ( 'NONE',  ( -4.763139720814407951, -2.750000000000016431, -173.5000000000000000 ) ) ;
#10607 = CARTESIAN_POINT ( 'NONE',  ( -5.196152422706601826, 2.999999999999975131, -83.46132486540524553 ) ) ;
#10608 = CARTESIAN_POINT ( 'NONE',  ( 107.2886751345947118, 2.000000000000085265, 1.110223024625156540E-13 ) ) ;
#10609 = ADVANCED_FACE ( 'NONE', ( #2352 ), #29834, .T. ) ;
#10610 = EDGE_LOOP ( 'NONE', ( #17795, #24116, #12928, #14031, #19011, #17375, #6652, #8261, #999, #5655, #22792, #23517, #16081, #20654, #10402, #29108, #23157, #24406, #16344, #16661, #13231, #24255, #5755, #12848, #5199, #15856, #18807, #18651, #10959, #24401, #15029, #21190, #3983 ) ) ;
#10611 = CARTESIAN_POINT ( 'NONE',  ( 13.93750000000017941, 2.000000000000151879, -0.8284271247462354770 ) ) ;
#10612 = DIRECTION ( 'NONE',  ( 1.000000000000000000, -5.551115123125773458E-17, -1.260129944081490338E-35 ) ) ;
#10613 = DIRECTION ( 'NONE',  ( 1.000000000000000000, -5.551115123125773458E-17, -1.260129944081490338E-35 ) ) ;
#10614 = DIRECTION ( 'NONE',  ( -7.147005652999508048E-36, 5.642372883946980038E-36, 1.000000000000000000 ) ) ;
#10615 = CARTESIAN_POINT ( 'NONE',  ( 159.8052981416689704, -11.45305019762678356, -3.625266920314750951 ) ) ;
#10616 = LINE ( 'NONE', #27458, #18752 ) ;
#10617 = CARTESIAN_POINT ( 'NONE',  ( 0.7566315082547844240, -15.57044312447410483, -7.988287420809495387 ) ) ;
#10618 = CARTESIAN_POINT ( 'NONE',  ( 114.0627832217621602, -0.7662911109077388261, -1.849990392679231599 ) ) ;
#10619 = CARTESIAN_POINT ( 'NONE',  ( 3.608439182435180470, -6.249999999999997335, -66.19198729810779014 ) ) ;
#10620 = AXIS2_PLACEMENT_3D ( 'NONE', #21096, #18799, #28126 ) ;
#10621 = CARTESIAN_POINT ( 'NONE',  ( 3.608439182435180470, 6.249999999999982236, -53.69198729810779724 ) ) ;
#10622 = CARTESIAN_POINT ( 'NONE',  ( 119.7113248654050750, 2.000000000000001776, 1.110223024625156540E-13 ) ) ;
#10623 = CARTESIAN_POINT ( 'NONE',  ( 0.000000000000000000, -5.999999999999991118, -64.03867513459482552 ) ) ;
#10624 = CARTESIAN_POINT ( 'NONE',  ( 119.9999999999999574, 2.481996037643088293, -0.1722232477815017759 ) ) ;
#10625 = FACE_OUTER_BOUND ( 'NONE', #19647, .T. ) ;
#10626 = ADVANCED_FACE ( 'NONE', ( #29988 ), #14071, .T. ) ;
#10627 = CARTESIAN_POINT ( 'NONE',  ( -6.350852961085760029, -1.281975124255709124E-13, -125.6250000000000426 ) ) ;
#10628 = ADVANCED_FACE ( 'NONE', ( #28129 ), #1660, .F. ) ;
#10629 = CARTESIAN_POINT ( 'NONE',  ( 108.3363248654050182, -1.414213562373201061, -1.414213562373034527 ) ) ;
#10630 = CARTESIAN_POINT ( 'NONE',  ( 104.7401757384973280, -1.849990392679412565, 2.220446049250313081E-13 ) ) ;
#10631 = ORIENTED_EDGE ( 'NONE', *, *, #4807, .F. ) ;
#10632 = CARTESIAN_POINT ( 'NONE',  ( 24.00000000000007816, -1.873492889144789952, 1.873492889144845464 ) ) ;
#10633 = CARTESIAN_POINT ( 'NONE',  ( 0.000000000000000000, 5.999999999999977796, -119.7113248654052597 ) ) ;
#10634 = DIRECTION ( 'NONE',  ( 0.000000000000000000, -1.000000000000000000, 0.000000000000000000 ) ) ;
#10635 = CARTESIAN_POINT ( 'NONE',  ( 153.0863248654052313, 0.000000000000000000, 5.500000000000005329 ) ) ;
#10636 = EDGE_LOOP ( 'NONE', ( #12316, #7406, #4553, #11601 ) ) ;
#10637 = CARTESIAN_POINT ( 'NONE',  ( 114.3747167782375556, -1.665334536937734811E-13, -1.849990392679523588 ) ) ;
#10638 = CARTESIAN_POINT ( 'NONE',  ( -5.196152422706601826, 2.999999999999975131, -71.46132486540524553 ) ) ;
#10639 = CARTESIAN_POINT ( 'NONE',  ( 3.608439182435180470, -6.249999999999997335, -99.19198729810781856 ) ) ;
#10640 = CARTESIAN_POINT ( 'NONE',  ( 135.0000000000001421, 4.599834066449496994, -3.434280637378118950 ) ) ;
#10641 = CARTESIAN_POINT ( 'NONE',  ( 11.39882486540520468, -1.035533905932568999, -2.499999999999904521 ) ) ;
#10642 = CARTESIAN_POINT ( 'NONE',  ( 115.6249999999998295, -1.767766952966376426, -1.767766952966320915 ) ) ;
#10643 = EDGE_LOOP ( 'NONE', ( #4230, #1863, #572, #28648 ) ) ;
#10644 = CARTESIAN_POINT ( 'NONE',  ( -5.999999999999963585, 1.780251999655701777E-13, -77.33632486540524553 ) ) ;
#10645 = CARTESIAN_POINT ( 'NONE',  ( 140.6250000000000284, 0.000000000000000000, -6.000000000000005329 ) ) ;
#10646 = CARTESIAN_POINT ( 'NONE',  ( 9.625000000000133227, -1.414213562372979016, -1.414213562373145550 ) ) ;
#10647 = CARTESIAN_POINT ( 'NONE',  ( 159.8733676508969666, -11.15074878458750085, 4.434313772618972749 ) ) ;
#10648 = CARTESIAN_POINT ( 'NONE',  ( -4.763139720814407951, 2.749999999999946709, -49.25000000000001421 ) ) ;
#10649 = EDGE_CURVE ( 'NONE', #234, #4156, #26650, .T. ) ;
#10650 = PRODUCT_DEFINITION_SHAPE ( 'NONE', 'NONE',  #30418 ) ;
#10651 = CARTESIAN_POINT ( 'NONE',  ( 16.96132486540522066, 1.110223024625156540E-13, 2.500000000000002220 ) ) ;
#10652 = CARTESIAN_POINT ( 'NONE',  ( -5.999999999999963585, 1.780251999655701777E-13, -62.91367513459483973 ) ) ;
#10653 = DIRECTION ( 'NONE',  ( 1.000000000000000000, -5.551115123125773458E-17, -1.260129944081490338E-35 ) ) ;
#10654 = CARTESIAN_POINT ( 'NONE',  ( -3.608439182435052128, -6.250000000000110134, -71.80801270189222407 ) ) ;
#10655 = CARTESIAN_POINT ( 'NONE',  ( -19.49999999999998224, -54.99999999999990763, -8.000000000000007105 ) ) ;
#10656 = CARTESIAN_POINT ( 'NONE',  ( 150.8288997308104058, 4.999999999999989342, -2.071067811865468400 ) ) ;
#10657 = CYLINDRICAL_SURFACE ( 'NONE', #17298, 17.50000000000004619 ) ;
#10658 = CARTESIAN_POINT ( 'NONE',  ( 0.000000000000000000, 0.000000000000000000, 0.000000000000000000 ) ) ;
#10659 = COLOUR_RGB ( '', 0.09019608, 0.27058824, 0.51372549) ;
#10660 = CARTESIAN_POINT ( 'NONE',  ( 5.999999999999999112, 2.951592740943527306E-14, -152.1636751345948255 ) ) ;
#10661 = FILL_AREA_STYLE_COLOUR ( '', #3463 ) ;
#10662 = CARTESIAN_POINT ( 'NONE',  ( 3.464101615137852974, 5.999999999999884537, -104.8363248654052029 ) ) ;
#10663 = ADVANCED_FACE ( 'NONE', ( #23406 ), #9416, .T. ) ;
#10664 =( BOUNDED_CURVE ( )  B_SPLINE_CURVE ( 2, ( #16446, #30221, #9186, #23021, #1967, #9500, #2427, #4260, #16299 ),
 .UNSPECIFIED., .F., .T. ) 
 B_SPLINE_CURVE_WITH_KNOTS ( ( 3, 2, 2, 2, 3 ),
 ( 0.8375000000000002442, 0.8437500000000000000, 0.8499999999999997558, 0.8562499999999995115, 0.8624999999999993783 ),
 .UNSPECIFIED. ) 
 CURVE ( )  GEOMETRIC_REPRESENTATION_ITEM ( )  RATIONAL_B_SPLINE_CURVE ( ( 0.9999999999999973355, 0.9238795325112894030, 1.000000000000000000, 0.9238795325112867385, 1.000000000000000000, 0.9238795325112867385, 1.000000000000000000, 0.9238795325112948431, 0.9999999999999918954 ) ) 
 REPRESENTATION_ITEM ( '' )  );
#10665 = CARTESIAN_POINT ( 'NONE',  ( 6.350852961086080661, -9.614813431917819062E-14, -133.8750000000000284 ) ) ;
#10666 = CARTESIAN_POINT ( 'NONE',  ( 105.4136751345947260, 1.414213562372979016, 1.414213562373256572 ) ) ;
#10667 = CIRCLE ( 'NONE', #4280, 2.000000000000012879 ) ;
#10668 = LINE ( 'NONE', #1257, #9623 ) ;
#10669 = ORIENTED_EDGE ( 'NONE', *, *, #13440, .F. ) ;
#10670 = CARTESIAN_POINT ( 'NONE',  ( 0.000000000000000000, 5.499999999999991118, -60.00000000000005684 ) ) ;
#10671 = CARTESIAN_POINT ( 'NONE',  ( 4.763139720814407951, -2.749999999999988454, -57.49999999999999289 ) ) ;
#10672 =( BOUNDED_CURVE ( )  B_SPLINE_CURVE ( 2, ( #18655, #16219, #14072, #27974, #4934, #30, #14365, #28131, #23104 ),
 .UNSPECIFIED., .F., .T. ) 
 B_SPLINE_CURVE_WITH_KNOTS ( ( 3, 2, 2, 2, 3 ),
 ( 0.9805555555555555136, 0.9814814814814815103, 0.9833333333333332815, 0.9851851851851851638, 0.9861111111111111605 ),
 .UNSPECIFIED. ) 
 CURVE ( )  GEOMETRIC_REPRESENTATION_ITEM ( )  RATIONAL_B_SPLINE_CURVE ( ( 0.9330127018922194093, 0.9330127018922154125, 1.000000000000000000, 0.8660254037844388186, 1.000000000000000000, 0.8660254037844388186, 1.000000000000000000, 0.9330127018922154125, 0.9330127018922194093 ) ) 
 REPRESENTATION_ITEM ( '' )  );
#10673 = CARTESIAN_POINT ( 'NONE',  ( -6.000000000000007105, -1.607695154586655129, -174.7693375672974412 ) ) ;
#10674 = ORIENTED_EDGE ( 'NONE', *, *, #14755, .F. ) ;
#10675 = CARTESIAN_POINT ( 'NONE',  ( 107.9374999999997726, 2.500000000000144773, -1.035533905932508825 ) ) ;
#10676 = CARTESIAN_POINT ( 'NONE',  ( 144.5625000000000284, -4.242640687119298093, 4.242640687119298093 ) ) ;
#10677 = CARTESIAN_POINT ( 'NONE',  ( 142.0386751345948255, -5.500000000000005329, 0.000000000000000000 ) ) ;
#10678 = CARTESIAN_POINT ( 'NONE',  ( 15.81250000000000178, 0.8284271247462354770, -2.000000000000151879 ) ) ;
#10679 = AXIS2_PLACEMENT_3D ( 'NONE', #5699, #3391, #12817 ) ;
#10680 = FILL_AREA_STYLE ('',( #8338 ) ) ;
#10681 = AXIS2_PLACEMENT_3D ( 'NONE', #9460, #7436, #9150 ) ;
#10682 = CARTESIAN_POINT ( 'NONE',  ( 112.3122167782374987, -0.7662911109076785410, -1.849990392679291551 ) ) ;
#10683 = CIRCLE ( 'NONE', #5243, 1.000000000000000888 ) ;
#10684 = ORIENTED_EDGE ( 'NONE', *, *, #11178, .T. ) ;
#10685 = CARTESIAN_POINT ( 'NONE',  ( 142.8750000000000284, 0.000000000000000000, 6.000000000000005329 ) ) ;
#10686 = CARTESIAN_POINT ( 'NONE',  ( 5.196152422706629359, -2.999999999999988898, -121.7113248654052597 ) ) ;
#10687 = ORIENTED_EDGE ( 'NONE', *, *, #11941, .T. ) ;
#10688 = CARTESIAN_POINT ( 'NONE',  ( 3.175426480543072749, -5.500000000000105693, -147.6250000000000284 ) ) ;
#10689 = CARTESIAN_POINT ( 'NONE',  ( 15.56250000000003553, -1.999999999999851674, -0.8284271247462354770 ) ) ;
#10690 = ORIENTED_EDGE ( 'NONE', *, *, #8183, .T. ) ;
#10691 = CARTESIAN_POINT ( 'NONE',  ( -7.216878364870328078, 0.000000000000000000, -146.1919872981078470 ) ) ;
#10692 = CARTESIAN_POINT ( 'NONE',  ( -4.763139720814407951, 2.749999999999946709, -70.25000000000002842 ) ) ;
#10693 = EDGE_CURVE ( 'NONE', #18702, #3793, #19369, .T. ) ;
#10694 = EDGE_CURVE ( 'NONE', #10419, #13111, #10949, .T. ) ;
#10695 = CARTESIAN_POINT ( 'NONE',  ( 5.412658773652712085, -3.125000000000086153, -90.93301270189225249 ) ) ;
#10696 = ORIENTED_EDGE ( 'NONE', *, *, #15120, .T. ) ;
#10697 = CARTESIAN_POINT ( 'NONE',  ( -5.799430203125090166, -9.347489878302569721, -23.41021253818530923 ) ) ;
#10698 = CARTESIAN_POINT ( 'NONE',  ( 0.000000000000000000, -5.999999999999991118, -96.46132486540520290 ) ) ;
#10699 = CARTESIAN_POINT ( 'NONE',  ( 148.5863248654052313, 0.000000000000000000, 5.500000000000005329 ) ) ;
#10700 = CARTESIAN_POINT ( 'NONE',  ( -6.000000000000007105, -1.607695154586655129, -86.84668783648706381 ) ) ;
#10701 = DIRECTION ( 'NONE',  ( 1.000000000000000000, -5.551115123125773458E-17, -1.260129944081490338E-35 ) ) ;
#10702 = COLOUR_RGB ( '', 0.09019608, 0.27058824, 0.51372549) ;
#10703 =( NAMED_UNIT ( * ) PLANE_ANGLE_UNIT ( ) SI_UNIT ( $, .RADIAN. ) );
#10704 = CARTESIAN_POINT ( 'NONE',  ( -6.350852961085760029, -1.281975124255709124E-13, -154.1250000000000568 ) ) ;
#10705 = CYLINDRICAL_SURFACE ( 'NONE', #10411, 6.000000000000000888 ) ;
#10706 = CARTESIAN_POINT ( 'NONE',  ( -2.775557561562891351E-14, -5.500000000000115463, -149.2500000000000000 ) ) ;
#10707 = CARTESIAN_POINT ( 'NONE',  ( 19.83632486540521001, 1.767766952966487448, 1.767766952966320915 ) ) ;
#10708 = UNCERTAINTY_MEASURE_WITH_UNIT (LENGTH_MEASURE( 1.000000000000000082E-05 ), #20839, 'distance_accuracy_value', 'NONE');
#10709 = CARTESIAN_POINT ( 'NONE',  ( 6.350852961086080661, -9.614813431917819062E-14, -82.87500000000004263 ) ) ;
#10710 = FACE_OUTER_BOUND ( 'NONE', #28557, .T. ) ;
#10711 = CARTESIAN_POINT ( 'NONE',  ( -6.350852961085760029, -1.281975124255709124E-13, -83.62499999999998579 ) ) ;
#10712 = DIRECTION ( 'NONE',  ( -7.147005652999508048E-36, 5.642372883946980038E-36, 1.000000000000000000 ) ) ;
#10713 = CARTESIAN_POINT ( 'NONE',  ( 151.5148502691896510, -3.535533905932725318, -3.535533905932725318 ) ) ;
#10714 = CARTESIAN_POINT ( 'NONE',  ( 150.3824251345948539, 5.500000000000012434, 2.278174593052012309 ) ) ;
#10715 = FACE_OUTER_BOUND ( 'NONE', #22688, .T. ) ;
#10716 = VECTOR ( 'NONE', #24206, 1000.000000000000000 ) ;
#10717 =( BOUNDED_CURVE ( )  B_SPLINE_CURVE ( 2, ( #24031, #14979, #16997, #12103, #26323, #21442, #375, #21745, #9766 ),
 .UNSPECIFIED., .F., .F. ) 
 B_SPLINE_CURVE_WITH_KNOTS ( ( 3, 2, 2, 2, 3 ),
 ( 0.1694444444444444253, 0.1703703703703703665, 0.1722222222222222210, 0.1740740740740740755, 0.1750000000000000167 ),
 .UNSPECIFIED. ) 
 CURVE ( )  GEOMETRIC_REPRESENTATION_ITEM ( )  RATIONAL_B_SPLINE_CURVE ( ( 0.9330127018922196314, 0.9330127018922185211, 1.000000000000000000, 0.8660254037844388186, 1.000000000000000000, 0.8660254037844388186, 1.000000000000000000, 0.9330127018922184101, 0.9330127018922194093 ) ) 
 REPRESENTATION_ITEM ( '' )  );
#10718 = CARTESIAN_POINT ( 'NONE',  ( 144.4613248654052313, -5.500000000000005329, 0.000000000000000000 ) ) ;
#10719 = CARTESIAN_POINT ( 'NONE',  ( 22.43750000000002842, -1.999999999999851674, 0.8284271247462354770 ) ) ;
#10720 =( BOUNDED_CURVE ( )  B_SPLINE_CURVE ( 2, ( #26087, #28823, #9817, #5327, #875, #21501, #21938, #285, #3032 ),
 .UNSPECIFIED., .F., .F. ) 
 B_SPLINE_CURVE_WITH_KNOTS ( ( 3, 2, 2, 2, 3 ),
 ( 0.6750000000000000444, 0.6759259259259259300, 0.6777777777777778123, 0.6796296296296295836, 0.6805555555555555802 ),
 .UNSPECIFIED. ) 
 CURVE ( )  GEOMETRIC_REPRESENTATION_ITEM ( )  RATIONAL_B_SPLINE_CURVE ( ( 0.9330127018922194093, 0.9330127018922234061, 1.000000000000000000, 0.8660254037844388186, 1.000000000000000000, 0.8660254037844388186, 1.000000000000000000, 0.9330127018922154125, 0.9330127018922194093 ) ) 
 REPRESENTATION_ITEM ( '' )  );
#10721 = CARTESIAN_POINT ( 'NONE',  ( 10.83632486540525619, 1.767766952966431937, 1.767766952966376426 ) ) ;
#10722 = CARTESIAN_POINT ( 'NONE',  ( 13.53867513459486283, 1.110223024625156540E-13, 2.499999999999946709 ) ) ;
#10723 = ORIENTED_EDGE ( 'NONE', *, *, #5209, .F. ) ;
#10724 = CARTESIAN_POINT ( 'NONE',  ( 160.6875000000000284, 4.242640687119269671, 4.242640687119298093 ) ) ;
#10725 = CARTESIAN_POINT ( 'NONE',  ( 6.000000000000052403, -1.607695154586662678, -78.73066243270262987 ) ) ;
#10726 = CARTESIAN_POINT ( 'NONE',  ( 118.8752832217621460, -1.849990392679384810, 2.220446049250313081E-13 ) ) ;
#10727 = ORIENTED_EDGE ( 'NONE', *, *, #19259, .F. ) ;
#10728 = ORIENTED_EDGE ( 'NONE', *, *, #24516, .T. ) ;
#10729 = CARTESIAN_POINT ( 'NONE',  ( -4.763139720814407951, -2.750000000000016431, -101.5000000000000284 ) ) ;
#10730 = FACE_OUTER_BOUND ( 'NONE', #10643, .T. ) ;
#10731 = ADVANCED_FACE ( 'NONE', ( #11288 ), #27669, .T. ) ;
#10732 = CARTESIAN_POINT ( 'NONE',  ( 5.412658773652712085, -3.125000000000086153, -111.9330127018922667 ) ) ;
#10733 = ORIENTED_EDGE ( 'NONE', *, *, #25964, .T. ) ;
#10734 = CARTESIAN_POINT ( 'NONE',  ( 6.000000000000000888, -1.859271017917181981E-14, -141.0863248654051745 ) ) ;
#10735 = DIRECTION ( 'NONE',  ( -1.000000000000000000, -1.665334536937736783E-16, -2.220446049250315546E-16 ) ) ;
#10736 = STYLED_ITEM ( 'NONE', ( #7918 ), #17567 ) ;
#10737 = LINE ( 'NONE', #19630, #14092 ) ;
#10738 = CARTESIAN_POINT ( 'NONE',  ( 2.775557561562891351E-14, -6.250000000000061284, -50.68301270189223828 ) ) ;
#10739 = ORIENTED_EDGE ( 'NONE', *, *, #16747, .F. ) ;
#10740 = CARTESIAN_POINT ( 'NONE',  ( 1.110223024625164183E-16, -2.000000000000012879, -1.776356839400262692E-15 ) ) ;
#10741 = CARTESIAN_POINT ( 'NONE',  ( 22.85117513459491434, -2.499999999999904521, -1.035533905932749299 ) ) ;
#10742 = CARTESIAN_POINT ( 'NONE',  ( 125.0000000000000568, -55.00000000000000711, 7.500000000000007105 ) ) ;
#10743 = DIRECTION ( 'NONE',  ( -7.147005652999508048E-36, 5.642372883946980038E-36, 1.000000000000000000 ) ) ;
#10744 = CARTESIAN_POINT ( 'NONE',  ( 3.175426480543072749, -5.500000000000105693, -170.1250000000000000 ) ) ;
#10745 = CARTESIAN_POINT ( 'NONE',  ( 117.8749999999998010, 1.767766952966320915, -1.767766952966209892 ) ) ;
#10746 = CARTESIAN_POINT ( 'NONE',  ( 10.46132486540518514, 5.551115123125782702E-14, -2.499999999999946709 ) ) ;
#10747 = CARTESIAN_POINT ( 'NONE',  ( -3.608439182435115633, 6.249999999999965361, -172.8080127018922667 ) ) ;
#10748 = DIRECTION ( 'NONE',  ( -7.147005652999508048E-36, 5.642372883946980038E-36, 1.000000000000000000 ) ) ;
#10749 = CARTESIAN_POINT ( 'NONE',  ( 3.175426480543072749, -5.500000000000105693, -107.1250000000000284 ) ) ;
#10750 = CARTESIAN_POINT ( 'NONE',  ( 13.28867513459505645, 2.500000000000224265, -5.551115123125782702E-14 ) ) ;
#10751 = CARTESIAN_POINT ( 'NONE',  ( -4.763139720814407951, -2.750000000000016431, -101.5000000000000284 ) ) ;
#10752 = FILL_AREA_STYLE_COLOUR ( '', #29999 ) ;
#10753 = FILL_AREA_STYLE ('',( #3634 ) ) ;
#10754 = CARTESIAN_POINT ( 'NONE',  ( 135.0000000000000284, -8.128268291558169878, 7.787242644550133264 ) ) ;
#10755 = ORIENTED_EDGE ( 'NONE', *, *, #1090, .T. ) ;
#10756 = CARTESIAN_POINT ( 'NONE',  ( -5.999999999999963585, 1.780251999655701777E-13, -90.83632486540521711 ) ) ;
#10757 = CARTESIAN_POINT ( 'NONE',  ( 109.2502832217621602, 1.308140751793751555, -1.308140751793640533 ) ) ;
#10758 = ORIENTED_EDGE ( 'NONE', *, *, #21100, .F. ) ;
#10759 = CARTESIAN_POINT ( 'NONE',  ( -6.350852961085760029, -1.281975124255709124E-13, -161.6250000000000284 ) ) ;
#10760 = CARTESIAN_POINT ( 'NONE',  ( 5.999999999999999112, 2.951592740943527306E-14, -156.6636751345948255 ) ) ;
#10761 = CARTESIAN_POINT ( 'NONE',  ( 108.4997167782375982, 1.308140751793668288, -1.308140751793418488 ) ) ;
#10762 = EDGE_CURVE ( 'NONE', #9352, #25369, #14113, .T. ) ;
#10763 = CARTESIAN_POINT ( 'NONE',  ( -5.412658773652684552, -3.125000000000099920, -83.06698729810779014 ) ) ;
#10764 = CARTESIAN_POINT ( 'NONE',  ( 149.9925748654051745, 2.278174593051981223, 5.500000000000041744 ) ) ;
#10765 = VERTEX_POINT ( 'NONE', #10019 ) ;
#10766 =( BOUNDED_CURVE ( )  B_SPLINE_CURVE ( 3, ( #6251, #12123, #12270, #16729 ),
 .UNSPECIFIED., .F., .T. ) 
 B_SPLINE_CURVE_WITH_KNOTS ( ( 4, 4 ),
 ( 3.536383773289563326, 4.712388980384689674 ),
 .UNSPECIFIED. ) 
 CURVE ( )  GEOMETRIC_REPRESENTATION_ITEM ( )  RATIONAL_B_SPLINE_CURVE ( ( 1.000000000000000000, 0.8880335295585641830, 0.8880335295585641830, 1.000000000000000000 ) ) 
 REPRESENTATION_ITEM ( '' )  );
#10767 = ORIENTED_EDGE ( 'NONE', *, *, #9689, .T. ) ;
#10768 = CARTESIAN_POINT ( 'NONE',  ( 158.4375000000000284, -4.242640687119298093, -4.242640687119298093 ) ) ;
#10769 = CARTESIAN_POINT ( 'NONE',  ( -4.763139720814407951, -2.750000000000016431, -119.5000000000000568 ) ) ;
#10770 = EDGE_CURVE ( 'NONE', #16190, #22104, #17224, .T. ) ;
#10771 = CARTESIAN_POINT ( 'NONE',  ( 2.775557561562891351E-14, -6.250000000000061284, -137.6830127018922099 ) ) ;
#10772 = DIRECTION ( 'NONE',  ( 0.000000000000000000, 1.000000000000000000, 0.000000000000000000 ) ) ;
#10773 = CIRCLE ( 'NONE', #3861, 1.000000000000000000 ) ;
#10774 = CARTESIAN_POINT ( 'NONE',  ( 5.412658773652739619, 3.124999999999988898, -125.8169872981078612 ) ) ;
#10775 = CARTESIAN_POINT ( 'NONE',  ( 6.000000000000000888, -1.859271017917181981E-14, -135.0863248654052029 ) ) ;
#10776 = CARTESIAN_POINT ( 'NONE',  ( -2.775557561562891351E-14, -5.500000000000115463, -173.2500000000000284 ) ) ;
#10777 = CARTESIAN_POINT ( 'NONE',  ( 160.0244396974608208, -11.17509275094623966, 4.373542244167537341 ) ) ;
#10778 = CARTESIAN_POINT ( 'NONE',  ( 107.4136751345947545, 1.414213562373201061, 1.414213562373256572 ) ) ;
#10779 = ORIENTED_EDGE ( 'NONE', *, *, #23074, .F. ) ;
#10780 = CARTESIAN_POINT ( 'NONE',  ( 16.62500000000013856, -1.414213562372867994, -1.414213562373145550 ) ) ;
#10781 = CARTESIAN_POINT ( 'NONE',  ( -5.999999999999963585, -1.487416814333745711E-14, -92.33632486540518869 ) ) ;
#10782 = CARTESIAN_POINT ( 'NONE',  ( 6.000000000000000888, 1.743066579297358182E-13, -90.66367513459483973 ) ) ;
#10783 = DIRECTION ( 'NONE',  ( 1.000000000000000000, 0.000000000000000000, 0.000000000000000000 ) ) ;
#10784 = CARTESIAN_POINT ( 'NONE',  ( 8.673617379884035472E-16, -14.14213562373095634, -8.500000000000007105 ) ) ;
#10785 = CARTESIAN_POINT ( 'NONE',  ( 114.7502832217623592, -1.308140751793640533, 1.308140751793640533 ) ) ;
#10786 = CARTESIAN_POINT ( 'NONE',  ( -3.608439182435115633, 6.249999999999965361, -63.94198729810785409 ) ) ;
#10787 = CARTESIAN_POINT ( 'NONE',  ( 119.4613248654050182, 5.551115123125782702E-14, -2.000000000000001776 ) ) ;
#10788 = LINE ( 'NONE', #15562, #12671 ) ;
#10789 = CARTESIAN_POINT ( 'NONE',  ( 107.7113248654050892, 2.000000000000057288, 0.000000000000000000 ) ) ;
#10790 = CARTESIAN_POINT ( 'NONE',  ( 3.175426480543072749, -5.500000000000105693, -132.6250000000000000 ) ) ;
#10791 = CARTESIAN_POINT ( 'NONE',  ( -5.196152422706601826, 2.999999999999975131, -138.0386751345948255 ) ) ;
#10792 = ORIENTED_EDGE ( 'NONE', *, *, #30040, .T. ) ;
#10793 = DIRECTION ( 'NONE',  ( -1.000000000000000000, 0.000000000000000000, 0.000000000000000000 ) ) ;
#10794 = AXIS2_PLACEMENT_3D ( 'NONE', #21565, #21260, #16681 ) ;
#10795 = CARTESIAN_POINT ( 'NONE',  ( 17.85117513459488947, -2.499999999999844569, -1.035533905932809473 ) ) ;
#10796 = CARTESIAN_POINT ( 'NONE',  ( 159.8363248654052313, 0.000000000000000000, -5.500000000000005329 ) ) ;
#10797 = VECTOR ( 'NONE', #24119, 1000.000000000000000 ) ;
#10798 = ORIENTED_EDGE ( 'NONE', *, *, #19113, .F. ) ;
#10799 = CARTESIAN_POINT ( 'NONE',  ( 115.4997167782375129, 1.308140751793640533, -1.308140751793640533 ) ) ;
#10800 = CARTESIAN_POINT ( 'NONE',  ( 10.91367513459493033, -1.767766952966265404, -1.767766952966376426 ) ) ;
#10801 = DIRECTION ( 'NONE',  ( -1.387778780781444256E-14, -1.000000000000000000, -0.000000000000000000 ) ) ;
#10802 = EDGE_CURVE ( 'NONE', #13611, #11502, #19331, .T. ) ;
#10803 = CARTESIAN_POINT ( 'NONE',  ( -7.216878364870328078, 0.000000000000000000, -116.1919872981078328 ) ) ;
#10804 = CARTESIAN_POINT ( 'NONE',  ( 19.78867513459489658, -2.499999999999946709, -1.110223024625156540E-13 ) ) ;
#10805 = CARTESIAN_POINT ( 'NONE',  ( 114.8749999999998295, 1.767766952966320915, -1.767766952966209892 ) ) ;
#10806 = ORIENTED_EDGE ( 'NONE', *, *, #23823, .T. ) ;
#10807 = CARTESIAN_POINT ( 'NONE',  ( 138.1011751345948539, 3.889087296526011706, -3.889087296526011706 ) ) ;
#10808 = CARTESIAN_POINT ( 'NONE',  ( 144.1875000000000284, 4.242640687119269671, 4.242640687119298093 ) ) ;
#10809 = EDGE_CURVE ( 'NONE', #23669, #2929, #20339, .T. ) ;
#10810 = EDGE_CURVE ( 'NONE', #17667, #476, #10011, .T. ) ;
#10811 = ORIENTED_EDGE ( 'NONE', *, *, #21983, .T. ) ;
#10812 = VERTEX_POINT ( 'NONE', #7691 ) ;
#10813 = CARTESIAN_POINT ( 'NONE',  ( 136.2113248654052029, 5.500000000000005329, 0.000000000000000000 ) ) ;
#10814 = CARTESIAN_POINT ( 'NONE',  ( -4.763139720814407951, -2.750000000000016431, -47.49999999999998579 ) ) ;
#10815 = AXIS2_PLACEMENT_3D ( 'NONE', #20458, #27653, #27499 ) ;
#10816 = DIRECTION ( 'NONE',  ( -1.000000000000000000, -1.665334536937736783E-16, -2.220446049250315546E-16 ) ) ;
#10817 = CARTESIAN_POINT ( 'NONE',  ( -5.412658773652739619, 3.124999999999975131, -75.18301270189226670 ) ) ;
#10818 = CARTESIAN_POINT ( 'NONE',  ( 116.7113248654051318, 2.000000000000057288, 0.000000000000000000 ) ) ;
#10819 = VECTOR ( 'NONE', #28264, 1000.000000000000000 ) ;
#10820 = CARTESIAN_POINT ( 'NONE',  ( 147.9226497308104058, 5.000000000000004441, 0.000000000000000000 ) ) ;
#10821 = CARTESIAN_POINT ( 'NONE',  ( -5.196152422706573404, -3.000000000000002665, -178.2886751345948539 ) ) ;
#10822 = CARTESIAN_POINT ( 'NONE',  ( 140.5384615384615756, -11.07692307692306777, 4.615384615384604317 ) ) ;
#10823 = CARTESIAN_POINT ( 'NONE',  ( 24.55536240870550557, -0.7428269089336653197, 2.333994687179698602 ) ) ;
#10824 = CARTESIAN_POINT ( 'NONE',  ( 6.350852961086080661, -9.614813431917819062E-14, -132.3750000000000284 ) ) ;
#10825 = CARTESIAN_POINT ( 'NONE',  ( -0.5000000000000004441, -9.500000000000008882, -7.500000000000007105 ) ) ;
#10826 = CARTESIAN_POINT ( 'NONE',  ( 0.000000000000000000, 0.000000000000000000, 0.000000000000000000 ) ) ;
#10827 = CARTESIAN_POINT ( 'NONE',  ( 3.464101615137852974, 5.999999999999884537, -178.3363248654052313 ) ) ;
#10828 = ORIENTED_EDGE ( 'NONE', *, *, #10938, .T. ) ;
#10829 = CARTESIAN_POINT ( 'NONE',  ( -4.763139720814407951, 2.749999999999946709, -64.25000000000002842 ) ) ;
#10830 = CARTESIAN_POINT ( 'NONE',  ( 3.464101615137852974, 5.999999999999884537, -70.33632486540518869 ) ) ;
#10831 = DIRECTION ( 'NONE',  ( 5.551115123125785167E-17, -1.000000000000000000, -8.881784197001256268E-16 ) ) ;
#10832 = ORIENTED_EDGE ( 'NONE', *, *, #16099, .F. ) ;
#10833 = CARTESIAN_POINT ( 'NONE',  ( 110.3124999999998863, -1.035533905932659149, 2.500000000000144773 ) ) ;
#10834 = CARTESIAN_POINT ( 'NONE',  ( 149.0625000000000284, -4.242640687119298093, 4.242640687119298093 ) ) ;
#10835 = CARTESIAN_POINT ( 'NONE',  ( 0.000000000000000000, 0.000000000000000000, 0.000000000000000000 ) ) ;
#10836 = CARTESIAN_POINT ( 'NONE',  ( 14.56249999999998934, -1.999999999999851674, -0.8284271247462354770 ) ) ;
#10837 = ADVANCED_FACE ( 'NONE', ( #12349 ), #28573, .T. ) ;
#10838 =( GEOMETRIC_REPRESENTATION_CONTEXT ( 3 ) GLOBAL_UNCERTAINTY_ASSIGNED_CONTEXT ( ( #12163 ) ) GLOBAL_UNIT_ASSIGNED_CONTEXT ( ( #769, #24715, #17377 ) ) REPRESENTATION_CONTEXT ( 'NONE', 'WORKASPACE' ) );
#10839 = ORIENTED_EDGE ( 'NONE', *, *, #4741, .F. ) ;
#10840 = AXIS2_PLACEMENT_3D ( 'NONE', #20740, #27613, #7456 ) ;
#10841 = CARTESIAN_POINT ( 'NONE',  ( 140.4375000000000284, -4.242640687119298093, -4.242640687119298093 ) ) ;
#10842 = CARTESIAN_POINT ( 'NONE',  ( 161.2636380912115612, -5.033346391500745476, 2.825791916966355011 ) ) ;
#10843 = EDGE_LOOP ( 'NONE', ( #440, #9413, #6572, #18053 ) ) ;
#10844 = ADVANCED_FACE ( 'NONE', ( #922 ), #12495, .F. ) ;
#10845 = CARTESIAN_POINT ( 'NONE',  ( -3.175426480542816510, -5.500000000000057732, -141.8750000000000568 ) ) ;
#10846 = ORIENTED_EDGE ( 'NONE', *, *, #4940, .F. ) ;
#10847 = CARTESIAN_POINT ( 'NONE',  ( 19.06250000000013500, 2.000000000000091926, 0.8284271247461753029 ) ) ;
#10848 = ORIENTED_EDGE ( 'NONE', *, *, #21609, .T. ) ;
#10849 = CARTESIAN_POINT ( 'NONE',  ( -6.350852961085760029, -1.281975124255709124E-13, -76.12500000000000000 ) ) ;
#10850 =( BOUNDED_CURVE ( )  B_SPLINE_CURVE ( 2, ( #6605, #16179, #28086, #11564, #23216, #11713, #16329, #2457, #23368 ),
 .UNSPECIFIED., .F., .T. ) 
 B_SPLINE_CURVE_WITH_KNOTS ( ( 3, 2, 2, 2, 3 ),
 ( 0.7972222222222222765, 0.7981481481481481621, 0.8000000000000000444, 0.8018518518518518157, 0.8027777777777778123 ),
 .UNSPECIFIED. ) 
 CURVE ( )  GEOMETRIC_REPRESENTATION_ITEM ( )  RATIONAL_B_SPLINE_CURVE ( ( 0.9330127018922194093, 0.9330127018922234061, 1.000000000000000000, 0.8660254037844388186, 1.000000000000000000, 0.8660254037844388186, 1.000000000000000000, 0.9330127018922154125, 0.9330127018922194093 ) ) 
 REPRESENTATION_ITEM ( '' )  );
#10851 = CARTESIAN_POINT ( 'NONE',  ( 5.412658773652739619, 3.124999999999988898, -93.68301270189222407 ) ) ;
#10852 = CARTESIAN_POINT ( 'NONE',  ( -6.000000000000000888, 1.067854986875958443E-15, 7.560779664488942560E-35 ) ) ;
#10853 = DIRECTION ( 'NONE',  ( 0.000000000000000000, 0.000000000000000000, -1.000000000000000000 ) ) ;
#10854 = VECTOR ( 'NONE', #13096, 1000.000000000000000 ) ;
#10855 = CARTESIAN_POINT ( 'NONE',  ( 6.000000000000052403, -1.607695154586662678, -86.23066243270258724 ) ) ;
#10856 = CARTESIAN_POINT ( 'NONE',  ( 24.49999999999999289, 0.6095397824026904665, 2.424553825690067832 ) ) ;
#10857 = PRODUCT_CONTEXT ( 'NONE', #27314, 'mechanical' ) ;
#10858 =( BOUNDED_CURVE ( )  B_SPLINE_CURVE ( 2, ( #1545, #17871, #10638, #19834, #15252, #12962, #20303, #22457, #8464 ),
 .UNSPECIFIED., .F., .F. ) 
 B_SPLINE_CURVE_WITH_KNOTS ( ( 3, 2, 2, 2, 3 ),
 ( 0.1861111111111111160, 0.1870370370370370017, 0.1888888888888888840, 0.1907407407407407662, 0.1916666666666666519 ),
 .UNSPECIFIED. ) 
 CURVE ( )  GEOMETRIC_REPRESENTATION_ITEM ( )  RATIONAL_B_SPLINE_CURVE ( ( 0.9330127018922194093, 0.9330127018922194093, 1.000000000000000000, 0.8660254037844388186, 1.000000000000000000, 0.8660254037844388186, 1.000000000000000000, 0.9330127018922194093, 0.9330127018922194093 ) ) 
 REPRESENTATION_ITEM ( '' )  );
#10859 = CARTESIAN_POINT ( 'NONE',  ( 4.763139720814407951, 2.750000000000002665, -159.2500000000000000 ) ) ;
#10860 = CARTESIAN_POINT ( 'NONE',  ( 17.58632486540531659, 1.767766952966487448, -1.767766952966598470 ) ) ;
#10861 = CARTESIAN_POINT ( 'NONE',  ( 156.6488248654052029, -3.889087296526011706, -3.889087296526011706 ) ) ;
#10862 = CARTESIAN_POINT ( 'NONE',  ( 6.350852961086080661, -9.614813431917819062E-14, -85.87500000000004263 ) ) ;
#10863 = CARTESIAN_POINT ( 'NONE',  ( -3.464101615137757051, -5.999999999999979572, -140.6636751345948255 ) ) ;
#10864 = SURFACE_STYLE_USAGE ( .BOTH. , #19604 ) ;
#10865 = CARTESIAN_POINT ( 'NONE',  ( 6.350852961086080661, -9.614813431917819062E-14, -82.87500000000004263 ) ) ;
#10866 = VECTOR ( 'NONE', #9099, 1000.000000000000000 ) ;
#10867 = CARTESIAN_POINT ( 'NONE',  ( -5.999999999999971578, 1.607695154586715303, -105.9033121635130072 ) ) ;
#10868 = CARTESIAN_POINT ( 'NONE',  ( 151.7886751345948255, 5.500000000000005329, 0.000000000000000000 ) ) ;
#10869 = CARTESIAN_POINT ( 'NONE',  ( 139.5863248654052313, 0.000000000000000000, 5.500000000000005329 ) ) ;
#10870 = ADVANCED_FACE ( 'NONE', ( #3527 ), #29027, .F. ) ;
#10871 = CARTESIAN_POINT ( 'NONE',  ( 150.1800748654052029, -2.278174593052043395, 5.499999999999981348 ) ) ;
#10872 = CARTESIAN_POINT ( 'NONE',  ( -5.999999999999963585, 1.780251999655701777E-13, -74.91367513459485394 ) ) ;
#10873 = EDGE_CURVE ( 'NONE', #23894, #12844, #23497, .T. ) ;
#10874 = VERTEX_POINT ( 'NONE', #5677 ) ;
#10875 = CARTESIAN_POINT ( 'NONE',  ( 161.6250000000000568, 0.000000000000000000, -6.000000000000005329 ) ) ;
#10876 = DIRECTION ( 'NONE',  ( 0.000000000000000000, 0.000000000000000000, 1.000000000000000000 ) ) ;
#10877 = CARTESIAN_POINT ( 'NONE',  ( 0.000000000000000000, -5.999999999999991118, -172.0386751345947971 ) ) ;
#10878 = CARTESIAN_POINT ( 'NONE',  ( 117.6252832217623165, 0.000000000000000000, 1.849990392679523588 ) ) ;
#10879 = DIRECTION ( 'NONE',  ( 1.000000000000000000, 1.665334536937736783E-16, 2.220446049250315546E-16 ) ) ;
#10880 = ORIENTED_EDGE ( 'NONE', *, *, #384, .T. ) ;
#10881 = AXIS2_PLACEMENT_3D ( 'NONE', #11994, #5012, #14443 ) ;
#10882 = ORIENTED_EDGE ( 'NONE', *, *, #26186, .F. ) ;
#10883 = CARTESIAN_POINT ( 'NONE',  ( -3.175426480542816510, -5.500000000000057732, -95.37500000000004263 ) ) ;
#10884 = LINE ( 'NONE', #22840, #19043 ) ;
#10885 = CARTESIAN_POINT ( 'NONE',  ( 3.608439182435180470, -6.249999999999997335, -118.0580127018922525 ) ) ;
#10886 = VERTEX_POINT ( 'NONE', #17705 ) ;
#10887 = CARTESIAN_POINT ( 'NONE',  ( 0.000000000000000000, 5.999999999999977796, -140.7113248654052313 ) ) ;
#10888 = LINE ( 'NONE', #2101, #22107 ) ;
#10889 = CARTESIAN_POINT ( 'NONE',  ( 21.47617513459490013, 1.035533905932809473, 2.499999999999844569 ) ) ;
#10890 = CARTESIAN_POINT ( 'NONE',  ( 3.608439182435180470, -6.249999999999997335, -50.55801270189225249 ) ) ;
#10891 = VERTEX_POINT ( 'NONE', #10796 ) ;
#10892 = DIRECTION ( 'NONE',  ( -7.147005652999508048E-36, 5.642372883946980038E-36, 1.000000000000000000 ) ) ;
#10893 =( NAMED_UNIT ( * ) PLANE_ANGLE_UNIT ( ) SI_UNIT ( $, .RADIAN. ) );
#10894 = CARTESIAN_POINT ( 'NONE',  ( 1.000000000000000666, -16.31586670994437682, -6.338163299696071284 ) ) ;
#10895 = CARTESIAN_POINT ( 'NONE',  ( -4.763139720814407951, 2.749999999999946709, -163.2500000000000000 ) ) ;
#10896 = CARTESIAN_POINT ( 'NONE',  ( 114.4374999999998010, -2.499999999999964473, 1.035533905932929599 ) ) ;
#10897 =( NAMED_UNIT ( * ) SI_UNIT ( $, .STERADIAN. ) SOLID_ANGLE_UNIT ( ) );
#10898 = AXIS2_PLACEMENT_3D ( 'NONE', #3971, #3665, #6434 ) ;
#10899 = CARTESIAN_POINT ( 'NONE',  ( -2.775557561562891351E-14, -5.500000000000115463, -110.2500000000000142 ) ) ;
#10900 = DIRECTION ( 'NONE',  ( 0.000000000000000000, 0.000000000000000000, -1.000000000000000000 ) ) ;
#10901 = CARTESIAN_POINT ( 'NONE',  ( -4.763139720814407951, 2.749999999999946709, -106.2500000000000142 ) ) ;
#10902 = DIRECTION ( 'NONE',  ( 1.000000000000000000, 0.000000000000000000, -0.000000000000000000 ) ) ;
#10903 = FACE_OUTER_BOUND ( 'NONE', #22187, .T. ) ;
#10904 = CARTESIAN_POINT ( 'NONE',  ( 135.4999999999991189, -9.047800747817843714, 8.000000000000007105 ) ) ;
#10905 = ORIENTED_EDGE ( 'NONE', *, *, #1432, .F. ) ;
#10906 = CARTESIAN_POINT ( 'NONE',  ( 13.68750000000000178, 2.649519052838298805, 1.097466725451559322 ) ) ;
#10907 = CARTESIAN_POINT ( 'NONE',  ( 115.6249999999998295, -1.767766952966376426, -1.767766952966320915 ) ) ;
#10908 = CARTESIAN_POINT ( 'NONE',  ( 109.8127832217621034, -1.849990392679501827, 0.7662911109077686911 ) ) ;
#10909 = ADVANCED_FACE ( 'NONE', ( #3372 ), #6155, .F. ) ;
#10910 = ORIENTED_EDGE ( 'NONE', *, *, #24703, .F. ) ;
#10911 = CARTESIAN_POINT ( 'NONE',  ( -5.999999999999963585, -1.487416814333745711E-14, -127.4136751345948113 ) ) ;
#10912 = VECTOR ( 'NONE', #15940, 1000.000000000000000 ) ;
#10913 = CARTESIAN_POINT ( 'NONE',  ( 7.216878364870455975, -6.409875621278545621E-14, -91.44198729810784698 ) ) ;
#10914 = PRODUCT ( 'Handle knob', 'Handle knob', '', ( #20211 ) ) ;
#10915 = CARTESIAN_POINT ( 'NONE',  ( 135.0000000000000284, 1.469576158976823947E-15, 12.00000000000000178 ) ) ;
#10916 = ORIENTED_EDGE ( 'NONE', *, *, #11013, .F. ) ;
#10917 = CYLINDRICAL_SURFACE ( 'NONE', #15011, 6.000000000000000888 ) ;
#10918 = COLOUR_RGB ( '', 0.66274510, 0.83137255, 0.94901961) ;
#10919 = ORIENTED_EDGE ( 'NONE', *, *, #12820, .F. ) ;
#10920 = ORIENTED_EDGE ( 'NONE', *, *, #332, .F. ) ;
#10921 = CARTESIAN_POINT ( 'NONE',  ( 157.7812500000000568, 2.485281374238585972, 6.000000000000005329 ) ) ;
#10922 = VECTOR ( 'NONE', #12198, 1000.000000000000000 ) ;
#10923 = CARTESIAN_POINT ( 'NONE',  ( -6.350852961085760029, -1.281975124255709124E-13, -122.6250000000000426 ) ) ;
#10924 = EDGE_LOOP ( 'NONE', ( #13267, #21894, #11524 ) ) ;
#10925 = CARTESIAN_POINT ( 'NONE',  ( 5.196152422706629359, 3.000000000000002665, -161.0386751345948539 ) ) ;
#10926 = CARTESIAN_POINT ( 'NONE',  ( 2.775557561562891351E-14, -6.250000000000061284, -123.3169872981078043 ) ) ;
#10927 = CARTESIAN_POINT ( 'NONE',  ( 5.412658773652739619, 3.124999999999988898, -175.3169872981078470 ) ) ;
#10928 = CARTESIAN_POINT ( 'NONE',  ( -6.350852961085760029, -1.281975124255709124E-13, -175.1250000000000284 ) ) ;
#10929 = FACE_OUTER_BOUND ( 'NONE', #8427, .T. ) ;
#10930 = CARTESIAN_POINT ( 'NONE',  ( -5.999999999999963585, 1.780251999655701777E-13, -47.33632486540523132 ) ) ;
#10931 = VERTEX_POINT ( 'NONE', #29335 ) ;
#10932 = DIRECTION ( 'NONE',  ( -1.000000000000000000, -1.665334536937731113E-16, 1.526556658859586792E-16 ) ) ;
#10933 = CARTESIAN_POINT ( 'NONE',  ( 159.5092728369245378, -12.11071345234885754, -3.863094837972295803 ) ) ;
#10934 = CYLINDRICAL_SURFACE ( 'NONE', #13859, 15.00000000000000000 ) ;
#10935 = CARTESIAN_POINT ( 'NONE',  ( 13.66367513459493210, -1.767766952966320915, 1.767766952966431937 ) ) ;
#10936 = CARTESIAN_POINT ( 'NONE',  ( 2.775557561562891351E-14, 6.250000000000033751, -65.56698729810783277 ) ) ;
#10937 = CARTESIAN_POINT ( 'NONE',  ( -7.216878364870328078, 0.000000000000000000, -54.69198729810780435 ) ) ;
#10938 = EDGE_CURVE ( 'NONE', #27584, #12287, #5529, .T. ) ;
#10939 = CARTESIAN_POINT ( 'NONE',  ( -5.999999999999963585, 1.780251999655701777E-13, -110.3363248654052029 ) ) ;
#10940 = CARTESIAN_POINT ( 'NONE',  ( 0.000000000000000000, 5.499999999999991118, -51.00000000000004263 ) ) ;
#10941 = CARTESIAN_POINT ( 'NONE',  ( 119.9999999999997158, 1.183822024845517351, -1.888846423996454860 ) ) ;
#10942 = CARTESIAN_POINT ( 'NONE',  ( 0.000000000000000000, 0.000000000000000000, 0.000000000000000000 ) ) ;
#10943 = CARTESIAN_POINT ( 'NONE',  ( 0.000000000000000000, 5.499999999999991118, -132.0000000000000000 ) ) ;
#10944 = EDGE_LOOP ( 'NONE', ( #10290, #24501, #9317, #17702 ) ) ;
#10945 = CARTESIAN_POINT ( 'NONE',  ( 23.25000000000018829, -1.873492889144734441, -1.873492889145011997 ) ) ;
#10946 = DIRECTION ( 'NONE',  ( 1.000000000000000000, -5.551115123125773458E-17, -1.260129944081490338E-35 ) ) ;
#10947 = CARTESIAN_POINT ( 'NONE',  ( 138.9523502691896510, 0.000000000000000000, 5.000000000000004441 ) ) ;
#10948 = CARTESIAN_POINT ( 'NONE',  ( 6.000000000000000888, -1.859271017917181981E-14, -147.6636751345948255 ) ) ;
#10949 =( BOUNDED_CURVE ( )  B_SPLINE_CURVE ( 2, ( #11126, #27514, #6492, #20474, #18197, #1882, #18353, #13599, #22943 ),
 .UNSPECIFIED., .F., .T. ) 
 B_SPLINE_CURVE_WITH_KNOTS ( ( 3, 2, 2, 2, 3 ),
 ( 0.2027777777777777790, 0.2037037037037036924, 0.2055555555555555469, 0.2074074074074074014, 0.2083333333333333426 ),
 .UNSPECIFIED. ) 
 CURVE ( )  GEOMETRIC_REPRESENTATION_ITEM ( )  RATIONAL_B_SPLINE_CURVE ( ( 0.9330127018922194093, 0.9330127018922194093, 1.000000000000000000, 0.8660254037844388186, 1.000000000000000000, 0.8660254037844388186, 1.000000000000000000, 0.9330127018922184101, 0.9330127018922194093 ) ) 
 REPRESENTATION_ITEM ( '' )  );
#10950 = EDGE_CURVE ( 'NONE', #28820, #7308, #12800, .T. ) ;
#10951 = ORIENTED_EDGE ( 'NONE', *, *, #3720, .F. ) ;
#10952 = CARTESIAN_POINT ( 'NONE',  ( 113.9372167782373566, -0.7662911109077388261, 1.849990392679652151 ) ) ;
#10953 = DIRECTION ( 'NONE',  ( 1.526556658859587038E-16, -2.081668171172187002E-17, 1.000000000000000000 ) ) ;
#10954 = DIRECTION ( 'NONE',  ( -7.147005652999508048E-36, 5.642372883946980038E-36, 1.000000000000000000 ) ) ;
#10955 = CARTESIAN_POINT ( 'NONE',  ( 5.412658773652712085, -3.125000000000086153, -117.0669872981078328 ) ) ;
#10956 = CARTESIAN_POINT ( 'NONE',  ( 0.000000000000000000, -5.999999999999991118, -109.9613248654052171 ) ) ;
#10957 = COLOUR_RGB ( '', 0.66274510, 0.83137255, 0.94901961) ;
#10958 = DIRECTION ( 'NONE',  ( -8.326672684688675286E-17, -2.081668171172168821E-17, 1.000000000000000000 ) ) ;
#10959 = ORIENTED_EDGE ( 'NONE', *, *, #5246, .F. ) ;
#10960 = CARTESIAN_POINT ( 'NONE',  ( 104.9999999999999432, 2.775557561562891351E-14, 1.110223024625156540E-13 ) ) ;
#10961 = CARTESIAN_POINT ( 'NONE',  ( 140.7187500000000284, 2.485281374238555774, -6.000000000000005329 ) ) ;
#10962 = ORIENTED_EDGE ( 'NONE', *, *, #19965, .F. ) ;
#10963 = ORIENTED_EDGE ( 'NONE', *, *, #2004, .F. ) ;
#10964 = LINE ( 'NONE', #18335, #13137 ) ;
#10965 = CARTESIAN_POINT ( 'NONE',  ( 6.000000000000000888, 1.743066579297358182E-13, -107.1636751345948539 ) ) ;
#10966 = CARTESIAN_POINT ( 'NONE',  ( 22.12500000000006040, 1.414213562373145550, 1.414213562373201061 ) ) ;
#10967 = CARTESIAN_POINT ( 'NONE',  ( 116.0000000000000142, 0.000000000000000000, 0.000000000000000000 ) ) ;
#10968 = DIRECTION ( 'NONE',  ( -0.000000000000000000, -0.000000000000000000, -1.000000000000000000 ) ) ;
#10969 = CARTESIAN_POINT ( 'NONE',  ( -5.412658773652739619, 3.124999999999975131, -64.68301270189225249 ) ) ;
#10970 = VECTOR ( 'NONE', #16206, 1000.000000000000000 ) ;
#10971 = CARTESIAN_POINT ( 'NONE',  ( 150.4538997308104626, -2.071067811865468400, -4.999999999999989342 ) ) ;
#10972 = CARTESIAN_POINT ( 'NONE',  ( 16.46132486540524553, 2.220446049250313081E-13, -2.500000000000002220 ) ) ;
#10973 = FACE_OUTER_BOUND ( 'NONE', #26184, .T. ) ;
#10974 = EDGE_CURVE ( 'NONE', #6046, #29880, #26594, .T. ) ;
#10975 = CYLINDRICAL_SURFACE ( 'NONE', #9901, 2.499999999999999112 ) ;
#10976 = FACE_OUTER_BOUND ( 'NONE', #22723, .T. ) ;
#10977 = CARTESIAN_POINT ( 'NONE',  ( 135.0476735965559101, -7.696154670787128005, 8.313613484422726074 ) ) ;
#10978 = MECHANICAL_DESIGN_GEOMETRIC_PRESENTATION_REPRESENTATION (  '', ( #637 ), #26601 ) ;
#10979 = CARTESIAN_POINT ( 'NONE',  ( -3.175426480542816066, 5.499999999999865885, -130.3750000000000284 ) ) ;
#10980 = CARTESIAN_POINT ( 'NONE',  ( 3.608439182435180470, -6.249999999999997335, -148.0580127018922383 ) ) ;
#10981 = DIRECTION ( 'NONE',  ( 1.000000000000000000, 1.665334536937731113E-16, -1.526556658859586792E-16 ) ) ;
#10982 = ORIENTED_EDGE ( 'NONE', *, *, #9689, .F. ) ;
#10983 = CARTESIAN_POINT ( 'NONE',  ( -4.763139720814407951, 2.749999999999946709, -61.25000000000002842 ) ) ;
#10984 = EDGE_CURVE ( 'NONE', #11104, #3131, #2487, .T. ) ;
#10985 = ORIENTED_EDGE ( 'NONE', *, *, #2547, .T. ) ;
#10986 = CARTESIAN_POINT ( 'NONE',  ( 107.5624999999998153, -2.499999999999874767, -1.035533905932629173 ) ) ;
#10987 = CARTESIAN_POINT ( 'NONE',  ( 145.5937500000000284, 6.000000000000005329, 2.485281374238585972 ) ) ;
#10988 = CARTESIAN_POINT ( 'NONE',  ( 161.0000000000000284, -11.67610212985246676, -2.769230769230771827 ) ) ;
#10989 = LINE ( 'NONE', #8659, #13630 ) ;
#10990 = VERTEX_POINT ( 'NONE', #22452 ) ;
#10991 = CARTESIAN_POINT ( 'NONE',  ( 135.5625000000000284, -4.242640687119298093, 4.242640687119298093 ) ) ;
#10992 = AXIS2_PLACEMENT_3D ( 'NONE', #13985, #2115, #7017 ) ;
#10993 = ORIENTED_EDGE ( 'NONE', *, *, #25616, .T. ) ;
#10994 =( BOUNDED_CURVE ( )  B_SPLINE_CURVE ( 2, ( #10352, #29058, #7870, #3107, #14671, #5110, #12238, #12381, #14963 ),
 .UNSPECIFIED., .F., .F. ) 
 B_SPLINE_CURVE_WITH_KNOTS ( ( 3, 2, 2, 2, 3 ),
 ( 0.4875000000000000444, 0.4937500000000002998, 0.5000000000000005551, 0.5062500000000007550, 0.5125000000000009548 ),
 .UNSPECIFIED. ) 
 CURVE ( )  GEOMETRIC_REPRESENTATION_ITEM ( )  RATIONAL_B_SPLINE_CURVE ( ( 0.9999999999999993339, 0.9238795325112874046, 1.000000000000000000, 0.9238795325112867385, 1.000000000000000000, 0.9238795325112867385, 1.000000000000000000, 0.9238795325112745260, 1.000000000000012212 ) ) 
 REPRESENTATION_ITEM ( '' )  );
#10995 = CARTESIAN_POINT ( 'NONE',  ( 6.350852961086080661, -9.614813431917819062E-14, -148.8750000000000284 ) ) ;
#10996 = AXIS2_PLACEMENT_3D ( 'NONE', #18221, #25092, #4049 ) ;
#10997 = CARTESIAN_POINT ( 'NONE',  ( 12.93750000000004263, 2.000000000000151879, -0.8284271247462955401 ) ) ;
#10998 = VERTEX_POINT ( 'NONE', #1386 ) ;
#10999 = CARTESIAN_POINT ( 'NONE',  ( -2.775557561562891351E-14, -5.500000000000115463, -77.25000000000004263 ) ) ;
#11000 = CARTESIAN_POINT ( 'NONE',  ( 15.12500000000008349, 1.665334536937734811E-13, -2.649519052838555933 ) ) ;
#11001 = ORIENTED_EDGE ( 'NONE', *, *, #12894, .T. ) ;
#11002 = CARTESIAN_POINT ( 'NONE',  ( 104.9999999999999005, -0.4876318259229017738, -1.939643060551943243 ) ) ;
#11003 = ADVANCED_FACE ( 'NONE', ( #20146 ), #8459, .T. ) ;
#11004 = CARTESIAN_POINT ( 'NONE',  ( -5.196152422706601826, 2.999999999999975131, -150.0386751345948539 ) ) ;
#11005 = CARTESIAN_POINT ( 'NONE',  ( 148.3050748654052029, 5.500000000000012434, 2.278174593052012309 ) ) ;
#11006 = DIRECTION ( 'NONE',  ( -0.000000000000000000, -0.000000000000000000, -1.000000000000000000 ) ) ;
#11007 = CARTESIAN_POINT ( 'NONE',  ( 121.3752832217622881, 1.849990392679579099, 0.000000000000000000 ) ) ;
#11008 = SHAPE_DEFINITION_REPRESENTATION ( #15587, #13689 ) ;
#11009 = CARTESIAN_POINT ( 'NONE',  ( -3.175426480542816066, 5.499999999999865885, -158.8750000000000000 ) ) ;
#11010 = CARTESIAN_POINT ( 'NONE',  ( 17.77382486540514250, 2.500000000000144773, 1.035533905932689347 ) ) ;
#11011 = CARTESIAN_POINT ( 'NONE',  ( -3.175426480542816066, 5.499999999999865885, -88.37500000000001421 ) ) ;
#11012 = CARTESIAN_POINT ( 'NONE',  ( 3.464101615137757051, -5.999999999999979572, -140.4136751345948255 ) ) ;
#11013 = EDGE_CURVE ( 'NONE', #16005, #9495, #10368, .T. ) ;
#11014 = CARTESIAN_POINT ( 'NONE',  ( 6.350852961086080661, -9.614813431917819062E-14, -70.87500000000004263 ) ) ;
#11015 = EDGE_CURVE ( 'NONE', #10886, #18250, #20911, .T. ) ;
#11016 = CARTESIAN_POINT ( 'NONE',  ( -5.196152422706601826, 2.999999999999975131, -105.9613248654052171 ) ) ;
#11017 = CARTESIAN_POINT ( 'NONE',  ( -6.000000000000007105, -1.607695154586655129, -108.7693375672974412 ) ) ;
#11018 = CARTESIAN_POINT ( 'NONE',  ( 135.2886751345948539, 5.500000000000005329, 0.000000000000000000 ) ) ;
#11019 = CARTESIAN_POINT ( 'NONE',  ( -5.999999999999971578, 1.607695154586715303, -54.90331216351302146 ) ) ;
#11020 = DIRECTION ( 'NONE',  ( 1.000000000000000000, -5.551115123125773458E-17, -1.260129944081490338E-35 ) ) ;
#11021 = CYLINDRICAL_SURFACE ( 'NONE', #22845, 6.000000000000000888 ) ;
#11022 = VERTEX_POINT ( 'NONE', #23372 ) ;
#11023 = CARTESIAN_POINT ( 'NONE',  ( 158.7187500000000000, 2.485281374238555774, -6.000000000000005329 ) ) ;
#11024 = CYLINDRICAL_SURFACE ( 'NONE', #11177, 2.499999999999999112 ) ;
#11025 = CARTESIAN_POINT ( 'NONE',  ( 24.85364373589974818, 0.2738724476063931212, -2.146356264100431677 ) ) ;
#11026 =( BOUNDED_CURVE ( )  B_SPLINE_CURVE ( 2, ( #6478, #22772, #11270, #13427, #27654 ),
 .UNSPECIFIED., .F., .F. ) 
 B_SPLINE_CURVE_WITH_KNOTS ( ( 3, 2, 3 ),
 ( 0.9117647058823529216, 0.9191176470588234837, 0.9241494898189103191 ),
 .UNSPECIFIED. ) 
 CURVE ( )  GEOMETRIC_REPRESENTATION_ITEM ( )  RATIONAL_B_SPLINE_CURVE ( ( 1.000000000000000000, 0.9238795325112867385, 1.000000000000000000, 0.9479084336410595890, 0.9671125746063085060 ) ) 
 REPRESENTATION_ITEM ( '' )  );
#11027 = EDGE_LOOP ( 'NONE', ( #3732, #10993, #897, #11690 ) ) ;
#11028 = CARTESIAN_POINT ( 'NONE',  ( 0.000000000000000000, 5.499999999999991118, -100.5000000000000284 ) ) ;
#11029 = DIRECTION ( 'NONE',  ( -7.147005652999508048E-36, 5.642372883946980038E-36, 1.000000000000000000 ) ) ;
#11030 = CARTESIAN_POINT ( 'NONE',  ( 2.775557561562891351E-14, 6.250000000000033751, -115.9330127018922667 ) ) ;
#11031 = CARTESIAN_POINT ( 'NONE',  ( -5.999999999999963585, 1.780251999655701777E-13, -110.3363248654052029 ) ) ;
#11032 = CARTESIAN_POINT ( 'NONE',  ( -0.5000000000000004441, -14.50000000000001243, -8.000000000000007105 ) ) ;
#11033 = CARTESIAN_POINT ( 'NONE',  ( -5.999999999999963585, 1.780251999655701777E-13, -107.9136751345948397 ) ) ;
#11034 = ADVANCED_FACE ( 'NONE', ( #30107 ), #25653, .T. ) ;
#11035 = CARTESIAN_POINT ( 'NONE',  ( -5.412658773652739619, 3.124999999999975131, -55.68301270189224539 ) ) ;
#11036 = ORIENTED_EDGE ( 'NONE', *, *, #19209, .F. ) ;
#11037 = CARTESIAN_POINT ( 'NONE',  ( -5.999999999999971578, 1.607695154586715303, -159.9033121635130499 ) ) ;
#11038 = DIRECTION ( 'NONE',  ( 0.000000000000000000, 0.000000000000000000, 1.000000000000000000 ) ) ;
#11039 = CARTESIAN_POINT ( 'NONE',  ( -5.196152422706573404, -3.000000000000002665, -167.2113248654052313 ) ) ;
#11040 = CARTESIAN_POINT ( 'NONE',  ( 0.000000000000000000, 5.499999999999991118, -165.0000000000000284 ) ) ;
#11041 = CARTESIAN_POINT ( 'NONE',  ( 116.7499999999997584, 1.665334536937734811E-13, -2.499999999999724665 ) ) ;
#11042 = CARTESIAN_POINT ( 'NONE',  ( 10.33632486540525619, -1.767766952966209892, -1.767766952966487448 ) ) ;
#11043 = CARTESIAN_POINT ( 'NONE',  ( 6.350852961086080661, -9.614813431917819062E-14, -108.3750000000000426 ) ) ;
#11044 = DIRECTION ( 'NONE',  ( 5.551115123125785167E-17, -1.000000000000000000, -8.881784197001256268E-16 ) ) ;
#11045 = FACE_OUTER_BOUND ( 'NONE', #679, .T. ) ;
#11046 = EDGE_CURVE ( 'NONE', #6403, #22416, #20299, .T. ) ;
#11047 = CARTESIAN_POINT ( 'NONE',  ( 4.763139720814407951, -2.749999999999988454, -98.00000000000002842 ) ) ;
#11048 = FACE_OUTER_BOUND ( 'NONE', #19289, .T. ) ;
#11049 = DIRECTION ( 'NONE',  ( -1.000000000000000000, 0.000000000000000000, 0.000000000000000000 ) ) ;
#11050 = VERTEX_POINT ( 'NONE', #29645 ) ;
#11051 = CARTESIAN_POINT ( 'NONE',  ( 116.3749999999998579, -1.767766952966209892, 1.767766952966542959 ) ) ;
#11052 = CARTESIAN_POINT ( 'NONE',  ( 108.8127832217621176, -1.849990392679501827, 0.7662911109078287542 ) ) ;
#11053 = ORIENTED_EDGE ( 'NONE', *, *, #15719, .F. ) ;
#11054 = CARTESIAN_POINT ( 'NONE',  ( 5.999999999999949374, 1.607695154586804565, -112.5193375672973986 ) ) ;
#11055 = CARTESIAN_POINT ( 'NONE',  ( 109.2497167782375413, -1.308140751793585022, -1.308140751793640533 ) ) ;
#11056 = CARTESIAN_POINT ( 'NONE',  ( 5.412658773652739619, 3.124999999999988898, -89.81698729810783277 ) ) ;
#11057 = CARTESIAN_POINT ( 'NONE',  ( -5.196152422706573404, -3.000000000000002665, -129.7113248654052029 ) ) ;
#11058 = ORIENTED_EDGE ( 'NONE', *, *, #23492, .T. ) ;
#11059 = CARTESIAN_POINT ( 'NONE',  ( -4.384309399116673944, 10.08956758734764136, -29.10056064752988547 ) ) ;
#11060 = CARTESIAN_POINT ( 'NONE',  ( 4.763139720814407951, 2.750000000000002665, -151.7500000000000568 ) ) ;
#11061 = ORIENTED_EDGE ( 'NONE', *, *, #12403, .T. ) ;
#11062 = ORIENTED_EDGE ( 'NONE', *, *, #28305, .T. ) ;
#11063 = CARTESIAN_POINT ( 'NONE',  ( 159.4687500000000568, -2.485281374238585972, 6.000000000000005329 ) ) ;
#11064 = AXIS2_PLACEMENT_3D ( 'NONE', #27745, #18424, #2126 ) ;
#11065 = CARTESIAN_POINT ( 'NONE',  ( 0.000000000000000000, 5.499999999999991118, -120.0000000000000000 ) ) ;
#11066 = CARTESIAN_POINT ( 'NONE',  ( 7.216878364870455975, -6.409875621278545621E-14, -137.3080127018922667 ) ) ;
#11067 = ORIENTED_EDGE ( 'NONE', *, *, #15317, .F. ) ;
#11068 = CARTESIAN_POINT ( 'NONE',  ( 3.464101615137757051, -5.999999999999979572, -57.33632486540520290 ) ) ;
#11069 = CARTESIAN_POINT ( 'NONE',  ( 7.216878364870455975, -6.409875621278545621E-14, -119.9419872981078470 ) ) ;
#11070 = CARTESIAN_POINT ( 'NONE',  ( -4.763139720814407951, 2.749999999999946709, -170.7500000000000000 ) ) ;
#11071 = FACE_OUTER_BOUND ( 'NONE', #21527, .T. ) ;
#11072 =( REPRESENTATION_RELATIONSHIP ('NONE','NONE', #103, #1893 ) REPRESENTATION_RELATIONSHIP_WITH_TRANSFORMATION ( #207 )SHAPE_REPRESENTATION_RELATIONSHIP( ) );
#11073 = DIRECTION ( 'NONE',  ( 1.000000000000000000, -5.551115123125773458E-17, -1.260129944081490338E-35 ) ) ;
#11074 =( BOUNDED_CURVE ( )  B_SPLINE_CURVE ( 2, ( #16087, #27996, #7117, #25863, #9589, #25391, #14238, #11471, #203 ),
 .UNSPECIFIED., .F., .F. ) 
 B_SPLINE_CURVE_WITH_KNOTS ( ( 3, 2, 2, 2, 3 ),
 ( 0.5027777777777777679, 0.5037037037037036535, 0.5055555555555555358, 0.5074074074074074181, 0.5083333333333334147 ),
 .UNSPECIFIED. ) 
 CURVE ( )  GEOMETRIC_REPRESENTATION_ITEM ( )  RATIONAL_B_SPLINE_CURVE ( ( 0.9330127018922194093, 0.9330127018922194093, 1.000000000000000000, 0.8660254037844388186, 1.000000000000000000, 0.8660254037844388186, 1.000000000000000000, 0.9330127018922154125, 0.9330127018922194093 ) ) 
 REPRESENTATION_ITEM ( '' )  );
#11075 = ADVANCED_FACE ( 'NONE', ( #3986 ), #13409, .T. ) ;
#11076 = ORIENTED_EDGE ( 'NONE', *, *, #17627, .F. ) ;
#11077 = CARTESIAN_POINT ( 'NONE',  ( 12.56250000000007638, -1.999999999999851674, -0.8284271247462354770 ) ) ;
#11078 = DIRECTION ( 'NONE',  ( 0.000000000000000000, 5.551115123125768527E-17, -1.000000000000000000 ) ) ;
#11079 = EDGE_CURVE ( 'NONE', #9960, #10034, #22157, .T. ) ;
#11080 = CARTESIAN_POINT ( 'NONE',  ( 159.1714057324313103, -11.33333333361816031, -3.999999999173795562 ) ) ;
#11081 = CARTESIAN_POINT ( 'NONE',  ( 25.00000000000013500, 2.000000000000279332, -5.551115123125782702E-14 ) ) ;
#11082 = CARTESIAN_POINT ( 'NONE',  ( 110.6252832217622029, 5.551115123125782702E-14, 1.849990392679523588 ) ) ;
#11083 = CARTESIAN_POINT ( 'NONE',  ( 2.775557561562891351E-14, -6.250000000000061284, -76.81698729810781856 ) ) ;
#11084 = CARTESIAN_POINT ( 'NONE',  ( 2.775557561562891351E-14, -6.250000000000061284, -61.81698729810780435 ) ) ;
#11085 = DIRECTION ( 'NONE',  ( 1.000000000000000000, 0.000000000000000000, -0.000000000000000000 ) ) ;
#11086 = CARTESIAN_POINT ( 'NONE',  ( -6.350852961085760029, -1.281975124255709124E-13, -52.12500000000002132 ) ) ;
#11087 = DIRECTION ( 'NONE',  ( -0.000000000000000000, -0.000000000000000000, -1.000000000000000000 ) ) ;
#11088 = CARTESIAN_POINT ( 'NONE',  ( -39.00000000000000000, -20.00000000000001776, 3.000000000000002665 ) ) ;
#11089 = CARTESIAN_POINT ( 'NONE',  ( 3.175426480543072749, -5.500000000000105693, -125.1250000000000426 ) ) ;
#11090 =( NAMED_UNIT ( * ) PLANE_ANGLE_UNIT ( ) SI_UNIT ( $, .RADIAN. ) );
#11091 = ORIENTED_EDGE ( 'NONE', *, *, #14651, .T. ) ;
#11092 = CARTESIAN_POINT ( 'NONE',  ( 0.000000000000000000, 5.999999999999977796, -132.2886751345947971 ) ) ;
#11093 = AXIS2_PLACEMENT_3D ( 'NONE', #2970, #28764, #12098 ) ;
#11094 = CARTESIAN_POINT ( 'NONE',  ( 0.000000000000000000, 0.000000000000000000, 0.000000000000000000 ) ) ;
#11095 = CARTESIAN_POINT ( 'NONE',  ( 141.2961002691896510, 2.071067811865468400, -4.999999999999989342 ) ) ;
#11096 = ORIENTED_EDGE ( 'NONE', *, *, #2050, .T. ) ;
#11097 = CARTESIAN_POINT ( 'NONE',  ( 108.9997167782375698, -1.308140751793612777, 1.308140751793640533 ) ) ;
#11098 = DIRECTION ( 'NONE',  ( -1.000000000000000000, -1.665334536937731113E-16, 1.526556658859586792E-16 ) ) ;
#11099 = CARTESIAN_POINT ( 'NONE',  ( 14.96132486540535567, 5.551115123125782702E-14, 2.500000000000002220 ) ) ;
#11100 = CARTESIAN_POINT ( 'NONE',  ( 2.775557561562891351E-14, -6.250000000000061284, -114.3169872981077901 ) ) ;
#11101 = CARTESIAN_POINT ( 'NONE',  ( -5.196152422706573404, -3.000000000000002665, -173.7886751345948255 ) ) ;
#11102 = AXIS2_PLACEMENT_3D ( 'NONE', #8717, #25125, #20385 ) ;
#11103 = CARTESIAN_POINT ( 'NONE',  ( 10.00000000000014744, 1.820239013128537087, 1.173872493019222585 ) ) ;
#11104 = VERTEX_POINT ( 'NONE', #27476 ) ;
#11105 = CARTESIAN_POINT ( 'NONE',  ( 144.2812500000000284, 2.485281374238585972, 6.000000000000005329 ) ) ;
#11106 = ORIENTED_EDGE ( 'NONE', *, *, #6128, .T. ) ;
#11107 = ORIENTED_EDGE ( 'NONE', *, *, #5413, .T. ) ;
#11108 =( NAMED_UNIT ( * ) PLANE_ANGLE_UNIT ( ) SI_UNIT ( $, .RADIAN. ) );
#11109 = AXIS2_PLACEMENT_3D ( 'NONE', #20978, #18682, #211 ) ;
#11110 = CARTESIAN_POINT ( 'NONE',  ( 6.000000000000000888, -3.330669073875464691E-16, -7.560779664488942560E-35 ) ) ;
#11111 = CARTESIAN_POINT ( 'NONE',  ( 21.56250000000015987, -1.999999999999911626, -0.8284271247462354770 ) ) ;
#11112 = FACE_OUTER_BOUND ( 'NONE', #755, .T. ) ;
#11113 = CARTESIAN_POINT ( 'NONE',  ( -5.412658773652739619, 3.124999999999975131, -69.18301270189225249 ) ) ;
#11114 = ADVANCED_FACE ( 'NONE', ( #6452 ), #25179, .T. ) ;
#11115 = CARTESIAN_POINT ( 'NONE',  ( 151.5788997308104058, -4.999999999999989342, 2.071067811865468400 ) ) ;
#11116 = DIRECTION ( 'NONE',  ( -7.147005652999508048E-36, 5.642372883946980038E-36, 1.000000000000000000 ) ) ;
#11117 = CARTESIAN_POINT ( 'NONE',  ( -3.464101615137725076, 5.999999999999979572, -165.1636751345948255 ) ) ;
#11118 = CARTESIAN_POINT ( 'NONE',  ( -1.000000000000000888, 9.000000000000007105, -3.000000000000002665 ) ) ;
#11119 = CARTESIAN_POINT ( 'NONE',  ( -0.5000000000000004441, -15.00000000000001421, -8.000000000000007105 ) ) ;
#11120 =( BOUNDED_CURVE ( )  B_SPLINE_CURVE ( 2, ( #23578, #11944, #209, #9900, #18985, #9595, #19124, #28455, #16835 ),
 .UNSPECIFIED., .F., .T. ) 
 B_SPLINE_CURVE_WITH_KNOTS ( ( 3, 2, 2, 2, 3 ),
 ( 0.4361111111111111160, 0.4370370370370370017, 0.4388888888888888840, 0.4407407407407407662, 0.4416666666666666519 ),
 .UNSPECIFIED. ) 
 CURVE ( )  GEOMETRIC_REPRESENTATION_ITEM ( )  RATIONAL_B_SPLINE_CURVE ( ( 0.9330127018922194093, 0.9330127018922194093, 1.000000000000000000, 0.8660254037844388186, 1.000000000000000000, 0.8660254037844388186, 1.000000000000000000, 0.9330127018922194093, 0.9330127018922194093 ) ) 
 REPRESENTATION_ITEM ( '' )  );
#11121 = CARTESIAN_POINT ( 'NONE',  ( -3.175426480542816066, 5.499999999999865885, -125.8749999999999858 ) ) ;
#11122 = CARTESIAN_POINT ( 'NONE',  ( 137.7261751345948539, -3.889087296526011706, -3.889087296526011706 ) ) ;
#11123 = CARTESIAN_POINT ( 'NONE',  ( 6.000000000000000888, -1.859271017917181981E-14, -159.0863248654052313 ) ) ;
#11124 = EDGE_LOOP ( 'NONE', ( #20346, #24518, #5734, #17736 ) ) ;
#11125 = CARTESIAN_POINT ( 'NONE',  ( 4.763139720814407951, 2.750000000000002665, -63.25000000000002842 ) ) ;
#11126 = CARTESIAN_POINT ( 'NONE',  ( -5.999999999999963585, -1.487416814333745711E-14, -154.4136751345947971 ) ) ;
#11127 = CARTESIAN_POINT ( 'NONE',  ( 5.196152422706629359, 3.000000000000002665, -70.46132486540524553 ) ) ;
#11128 = ORIENTED_EDGE ( 'NONE', *, *, #8260, .T. ) ;
#11129 = CARTESIAN_POINT ( 'NONE',  ( 109.7499999999999147, 5.551115123125782702E-14, -2.499999999999835687 ) ) ;
#11130 = CARTESIAN_POINT ( 'NONE',  ( 148.5937500000000284, 6.000000000000005329, 2.485281374238585972 ) ) ;
#11131 = CYLINDRICAL_SURFACE ( 'NONE', #596, 6.000000000000000888 ) ;
#11132 = CARTESIAN_POINT ( 'NONE',  ( 12.93750000000004086, 2.000000000000151879, -0.8284271247462955401 ) ) ;
#11133 = DIRECTION ( 'NONE',  ( -0.3589790793088787901, 0.3589790793088650789, -0.8615497903412834280 ) ) ;
#11134 = CARTESIAN_POINT ( 'NONE',  ( 0.000000000000000000, 0.000000000000000000, 0.000000000000000000 ) ) ;
#11135 = VECTOR ( 'NONE', #20937, 1000.000000000000000 ) ;
#11136 = ORIENTED_EDGE ( 'NONE', *, *, #10051, .F. ) ;
#11137 = ADVANCED_FACE ( 'NONE', ( #13566 ), #22904, .F. ) ;
#11138 = COLOUR_RGB ( '', 0.40784314, 0.44705882, 0.49803922) ;
#11139 = CARTESIAN_POINT ( 'NONE',  ( -3.175426480542816510, -5.500000000000057732, -143.3750000000000000 ) ) ;
#11140 = AXIS2_PLACEMENT_3D ( 'NONE', #1319, #20077, #22691 ) ;
#11141 = CARTESIAN_POINT ( 'NONE',  ( 14.37500000000016520, -1.414213562373034527, 1.414213562372979016 ) ) ;
#11142 = ORIENTED_EDGE ( 'NONE', *, *, #22400, .T. ) ;
#11143 = AXIS2_PLACEMENT_3D ( 'NONE', #3706, #4329, #13747 ) ;
#11144 = CARTESIAN_POINT ( 'NONE',  ( 3.175426480543072749, 5.499999999999865885, -72.12500000000005684 ) ) ;
#11145 = CARTESIAN_POINT ( 'NONE',  ( 10.00000000000014566, -0.2706188729083223721, -2.470526507789089443 ) ) ;
#11146 = CARTESIAN_POINT ( 'NONE',  ( 7.216878364870455975, -6.409875621278545621E-14, -87.80801270189223828 ) ) ;
#11147 = EDGE_CURVE ( 'NONE', #13151, #13576, #4503, .T. ) ;
#11148 = CARTESIAN_POINT ( 'NONE',  ( -4.520081486476279053, -10.03271082534599401, -28.96438617129773618 ) ) ;
#11149 = CARTESIAN_POINT ( 'NONE',  ( 5.999999999999949374, 1.607695154586804565, -107.0966878364870638 ) ) ;
#11150 = DIRECTION ( 'NONE',  ( 1.000000000000000000, -5.551115123125774690E-17, 0.000000000000000000 ) ) ;
#11151 = DIRECTION ( 'NONE',  ( 0.000000000000000000, 0.000000000000000000, 1.000000000000000000 ) ) ;
#11152 = APPLICATION_PROTOCOL_DEFINITION ( 'draft international standard', 'automotive_design', 1998, #27314 ) ;
#11153 = CARTESIAN_POINT ( 'NONE',  ( -3.175426480542816066, -5.500000000000057732, -159.8750000000000284 ) ) ;
#11154 = DIRECTION ( 'NONE',  ( -1.000000000000000000, -1.665334536937731113E-16, 1.526556658859586792E-16 ) ) ;
#11155 = CARTESIAN_POINT ( 'NONE',  ( 0.000000000000000000, -14.26438599474648683, -8.432200732276358579 ) ) ;
#11156 = AXIS2_PLACEMENT_3D ( 'NONE', #18671, #20656, #27991 ) ;
#11157 = PRODUCT_DEFINITION_SHAPE ( 'NONE', 'NONE',  #22683 ) ;
#11158 = CARTESIAN_POINT ( 'NONE',  ( -4.763139720814407951, -2.750000000000016431, -86.50000000000002842 ) ) ;
#11159 = VECTOR ( 'NONE', #29374, 1000.000000000000000 ) ;
#11160 = VECTOR ( 'NONE', #12022, 1000.000000000000000 ) ;
#11161 = DIRECTION ( 'NONE',  ( -1.000000000000000000, 1.040834085586083310E-14, 0.000000000000000000 ) ) ;
#11162 = CARTESIAN_POINT ( 'NONE',  ( -6.350852961085760029, -1.281975124255709124E-13, -73.12500000000005684 ) ) ;
#11163 = CARTESIAN_POINT ( 'NONE',  ( 149.3586002691896510, 2.071067811865468400, 4.999999999999989342 ) ) ;
#11164 = CARTESIAN_POINT ( 'NONE',  ( 6.000000000000000888, 7.762456499804234384E-14, -142.5863248654051745 ) ) ;
#11165 = CARTESIAN_POINT ( 'NONE',  ( 104.8544169799067731, -1.915947604159734308, -0.2177314441303023207 ) ) ;
#11166 =( GEOMETRIC_REPRESENTATION_CONTEXT ( 3 ) GLOBAL_UNCERTAINTY_ASSIGNED_CONTEXT ( ( #28367 ) ) GLOBAL_UNIT_ASSIGNED_CONTEXT ( ( #26791, #24660, #15168 ) ) REPRESENTATION_CONTEXT ( 'NONE', 'WORKASPACE' ) );
#11167 = CARTESIAN_POINT ( 'NONE',  ( 135.0000000000066223, -7.337284433953279894, -8.409043885017243980 ) ) ;
#11168 = CARTESIAN_POINT ( 'NONE',  ( 114.4613248654051603, 5.551115123125782702E-14, -2.000000000000001776 ) ) ;
#11169 = CARTESIAN_POINT ( 'NONE',  ( 18.75000000000015632, 1.110223024625156540E-13, -2.000000000000168310 ) ) ;
#11170 = CARTESIAN_POINT ( 'NONE',  ( 139.2261751345948539, -3.889087296526011706, -3.889087296526011706 ) ) ;
#11171 =( BOUNDED_CURVE ( )  B_SPLINE_CURVE ( 2, ( #4962, #2663, #25563, #28006, #6823, #16248, #25871, #7127, #13945 ),
 .UNSPECIFIED., .F., .F. ) 
 B_SPLINE_CURVE_WITH_KNOTS ( ( 3, 2, 2, 2, 3 ),
 ( 0.8823529411764705621, 0.8897058823529411242, 0.8970588235294117974, 0.9044117647058823595, 0.9117647058823529216 ),
 .UNSPECIFIED. ) 
 CURVE ( )  GEOMETRIC_REPRESENTATION_ITEM ( )  RATIONAL_B_SPLINE_CURVE ( ( 1.000000000000000000, 0.9238795325112867385, 1.000000000000000000, 0.9238795325112867385, 1.000000000000000000, 0.9238795325112867385, 1.000000000000000000, 0.9238795325112867385, 1.000000000000000000 ) ) 
 REPRESENTATION_ITEM ( '' )  );
#11172 = CARTESIAN_POINT ( 'NONE',  ( 0.000000000000000000, 5.999999999999977796, -134.7113248654052597 ) ) ;
#11173 = CARTESIAN_POINT ( 'NONE',  ( 3.464101615137852974, 5.999999999999884537, -169.9136751345948255 ) ) ;
#11174 = VERTEX_POINT ( 'NONE', #2005 ) ;
#11175 = CARTESIAN_POINT ( 'NONE',  ( 157.5000000000000284, 6.000000000000005329, 0.000000000000000000 ) ) ;
#11176 = CARTESIAN_POINT ( 'NONE',  ( 14.58632486540512119, 1.767766952966542959, -1.767766952966487448 ) ) ;
#11177 = AXIS2_PLACEMENT_3D ( 'NONE', #1310, #3448, #29103 ) ;
#11178 = EDGE_CURVE ( 'NONE', #24742, #18130, #5597, .T. ) ;
#11179 = CARTESIAN_POINT ( 'NONE',  ( 0.000000000000000000, 5.999999999999977796, -157.2113248654052313 ) ) ;
#11180 = VERTEX_POINT ( 'NONE', #9535 ) ;
#11181 = ORIENTED_EDGE ( 'NONE', *, *, #6922, .T. ) ;
#11182 = ORIENTED_EDGE ( 'NONE', *, *, #11786, .T. ) ;
#11183 = CARTESIAN_POINT ( 'NONE',  ( -3.175426480542816510, 5.499999999999865885, -95.87500000000002842 ) ) ;
#11184 = VECTOR ( 'NONE', #28882, 1000.000000000000000 ) ;
#11185 = CARTESIAN_POINT ( 'NONE',  ( 5.196152422706629359, 3.000000000000002665, -71.03867513459482552 ) ) ;
#11186 = ADVANCED_FACE ( 'NONE', ( #7370 ), #26101, .T. ) ;
#11187 = CARTESIAN_POINT ( 'NONE',  ( 2.775557561562891351E-14, -6.250000000000061284, -109.1830127018922383 ) ) ;
#11188 = EDGE_CURVE ( 'NONE', #7302, #15059, #5090, .T. ) ;
#11189 = CARTESIAN_POINT ( 'NONE',  ( 116.0000000000000142, 0.000000000000000000, 0.000000000000000000 ) ) ;
#11190 = CARTESIAN_POINT ( 'NONE',  ( 0.000000000000000000, -5.999999999999991118, -143.5386751345948255 ) ) ;
#11191 = CARTESIAN_POINT ( 'NONE',  ( -3.175426480542816510, 5.499999999999865885, -166.3750000000000568 ) ) ;
#11192 = CARTESIAN_POINT ( 'NONE',  ( 3.608439182435180470, 6.249999999999982236, -47.05801270189223118 ) ) ;
#11193 = DIRECTION ( 'NONE',  ( 1.000000000000000000, -5.551115123125773458E-17, -1.260129944081490338E-35 ) ) ;
#11194 = ORIENTED_EDGE ( 'NONE', *, *, #17850, .T. ) ;
#11195 = CARTESIAN_POINT ( 'NONE',  ( 6.000000000000052403, -1.607695154586662678, -56.23066243270260856 ) ) ;
#11196 = CARTESIAN_POINT ( 'NONE',  ( 6.000000000000000888, -3.330669073875464691E-16, -7.560779664488942560E-35 ) ) ;
#11197 = CARTESIAN_POINT ( 'NONE',  ( 0.000000000000000000, 5.499999999999991118, -160.5000000000000284 ) ) ;
#11198 = CARTESIAN_POINT ( 'NONE',  ( 117.6874999999997726, -1.035533905932719101, -2.499999999999844569 ) ) ;
#11199 = CARTESIAN_POINT ( 'NONE',  ( -0.04562205425674009662, -14.50000000000001243, 8.291335958003937634 ) ) ;
#11200 = CARTESIAN_POINT ( 'NONE',  ( 3.175426480543072749, -5.500000000000105693, -111.6249999999999858 ) ) ;
#11201 = CARTESIAN_POINT ( 'NONE',  ( 104.9999999999998863, -0.4876318259229017738, -1.939643060551943243 ) ) ;
#11202 = CARTESIAN_POINT ( 'NONE',  ( 145.6800748654052029, -2.278174593052012309, 5.500000000000012434 ) ) ;
#11203 = CARTESIAN_POINT ( 'NONE',  ( -2.775557561562891351E-14, -5.500000000000115463, -99.75000000000000000 ) ) ;
#11204 = CARTESIAN_POINT ( 'NONE',  ( 159.4836002691896226, 4.999999999999989342, -2.071067811865468400 ) ) ;
#11205 = DIRECTION ( 'NONE',  ( 0.000000000000000000, -1.000000000000000000, 0.000000000000000000 ) ) ;
#11206 = CARTESIAN_POINT ( 'NONE',  ( -0.07773347327279958585, -14.92041145833903393, 8.102883078117887550 ) ) ;
#11207 = ORIENTED_EDGE ( 'NONE', *, *, #18747, .F. ) ;
#11208 = CARTESIAN_POINT ( 'NONE',  ( 115.8749999999998579, 1.767766952966431937, -1.767766952966320915 ) ) ;
#11209 = CARTESIAN_POINT ( 'NONE',  ( 110.3752832217623592, 1.849990392679495832, 0.000000000000000000 ) ) ;
#11210 = CARTESIAN_POINT ( 'NONE',  ( 107.9613248654050892, 1.110223024625156540E-13, 2.000000000000001776 ) ) ;
#11211 =( BOUNDED_CURVE ( )  B_SPLINE_CURVE ( 2, ( #16265, #9006, #30344, #1773, #6534, #15957, #11176, #28325, #17144 ),
 .UNSPECIFIED., .F., .T. ) 
 B_SPLINE_CURVE_WITH_KNOTS ( ( 3, 2, 2, 2, 3 ),
 ( 0.6093750000000000000, 0.6171875000000000000, 0.6250000000000000000, 0.6328125000000000000, 0.6406250000000000000 ),
 .UNSPECIFIED. ) 
 CURVE ( )  GEOMETRIC_REPRESENTATION_ITEM ( )  RATIONAL_B_SPLINE_CURVE ( ( 1.000000000000000000, 0.9238795325112867385, 1.000000000000000000, 0.9238795325112867385, 1.000000000000000000, 0.9238795325112867385, 1.000000000000000000, 0.9238795325112867385, 1.000000000000000000 ) ) 
 REPRESENTATION_ITEM ( '' )  );
#11212 = VERTEX_POINT ( 'NONE', #21214 ) ;
#11213 = CARTESIAN_POINT ( 'NONE',  ( 108.8122167782374703, 0.7662911109077987781, 1.849990392679712103 ) ) ;
#11214 = CARTESIAN_POINT ( 'NONE',  ( -3.608439182435052128, -6.250000000000110134, -88.94198729810783277 ) ) ;
#11215 = EDGE_CURVE ( 'NONE', #23369, #29507, #8778, .T. ) ;
#11216 = DIRECTION ( 'NONE',  ( -7.147005652999508048E-36, 5.642372883946980038E-36, 1.000000000000000000 ) ) ;
#11217 = ORIENTED_EDGE ( 'NONE', *, *, #7172, .F. ) ;
#11218 = DIRECTION ( 'NONE',  ( -0.000000000000000000, -0.000000000000000000, -1.000000000000000000 ) ) ;
#11219 =( BOUNDED_SURFACE ( )  B_SPLINE_SURFACE ( 3, 2, ( 
 ( #29355, #8317, #24762 ),
 ( #22471, #1409, #20931 ),
 ( #25201, #11588, #4164 ),
 ( #25512, #20462, #22774 ),
 ( #23088, #15903, #11272 ),
 ( #22929, #4476, #20625 ),
 ( #2030, #11436, #18635 ),
 ( #6931, #8949, #20318 ) ),
 .UNSPECIFIED., .F., .F., .T. ) 
 B_SPLINE_SURFACE_WITH_KNOTS ( ( 4, 2, 2, 4 ),
 ( 3, 3 ),
 ( 0.006483209092139470726, 0.007220185479632802716, 0.007957161867126135574, 0.009431114642112801288 ),
 ( 0.000000000000000000, 1.000000000000000000 ),
 .UNSPECIFIED. ) 
 GEOMETRIC_REPRESENTATION_ITEM ( )  RATIONAL_B_SPLINE_SURFACE ( (
 ( 1.000000000000000000, 0.9165151389911680990, 1.000000000000000000),
 ( 1.000000000000000000, 0.9165811099392860983, 1.000000000000000000),
 ( 1.000000000000000000, 0.9096513889649350260, 1.000000000000000000),
 ( 1.000000000000000000, 0.8858533194321830395, 1.000000000000000000),
 ( 1.000000000000000000, 0.8692663461313614448, 1.000000000000000000),
 ( 1.000000000000000000, 0.8111162787353217718, 1.000000000000000000),
 ( 1.000000000000000000, 0.7613968795859874517, 1.000000000000000000),
 ( 1.000000000000000000, 0.7050799574960493477, 1.000000000000000000) ) ) 
 REPRESENTATION_ITEM ( '' )  SURFACE ( )  );
#11220 = ORIENTED_EDGE ( 'NONE', *, *, #29407, .T. ) ;
#11221 = CARTESIAN_POINT ( 'NONE',  ( 156.2812500000000284, 2.485281374238585972, 6.000000000000005329 ) ) ;
#11222 = CARTESIAN_POINT ( 'NONE',  ( 3.175426480543072749, -5.500000000000105693, -125.1250000000000426 ) ) ;
#11223 = EDGE_CURVE ( 'NONE', #24705, #25491, #15717, .T. ) ;
#11224 = CARTESIAN_POINT ( 'NONE',  ( 7.216878364870455975, -6.409875621278545621E-14, -128.3080127018922383 ) ) ;
#11225 = ORIENTED_EDGE ( 'NONE', *, *, #23724, .F. ) ;
#11226 = LINE ( 'NONE', #15696, #23447 ) ;
#11227 = CARTESIAN_POINT ( 'NONE',  ( -5.412658773652684552, -3.125000000000099920, -123.5669872981078328 ) ) ;
#11228 = CARTESIAN_POINT ( 'NONE',  ( -7.216878364870328078, 0.000000000000000000, -177.6919872981078186 ) ) ;
#11229 =( NAMED_UNIT ( * ) SI_UNIT ( $, .STERADIAN. ) SOLID_ANGLE_UNIT ( ) );
#11230 = DIRECTION ( 'NONE',  ( 1.000000000000000000, -0.000000000000000000, -0.000000000000000000 ) ) ;
#11231 = ORIENTED_EDGE ( 'NONE', *, *, #14028, .T. ) ;
#11232 = CARTESIAN_POINT ( 'NONE',  ( 13.50000000000015099, -1.999999999999890754, -5.551115123125782702E-14 ) ) ;
#11233 = CARTESIAN_POINT ( 'NONE',  ( -0.07940172813350243608, -15.22961641030811286, -7.558960887114970717 ) ) ;
#11234 = FACE_OUTER_BOUND ( 'NONE', #6199, .T. ) ;
#11235 = CARTESIAN_POINT ( 'NONE',  ( 3.464101615137852974, 5.999999999999884537, -90.41367513459483973 ) ) ;
#11236 = DIRECTION ( 'NONE',  ( 1.000000000000000000, 0.000000000000000000, 0.000000000000000000 ) ) ;
#11237 = LINE ( 'NONE', #1988, #26614 ) ;
#11238 = CARTESIAN_POINT ( 'NONE',  ( 113.2502832217622455, 1.308140751793612777, -1.308140751793640533 ) ) ;
#11239 = CARTESIAN_POINT ( 'NONE',  ( 2.775557561562891351E-14, 6.250000000000033751, -76.06698729810779014 ) ) ;
#11240 = CARTESIAN_POINT ( 'NONE',  ( -3.608439182435115633, 6.249999999999965361, -62.44198729810783988 ) ) ;
#11241 = CARTESIAN_POINT ( 'NONE',  ( 4.763139720814407951, 2.750000000000002665, -46.75000000000001421 ) ) ;
#11242 = CARTESIAN_POINT ( 'NONE',  ( 5.196152422706629359, -2.999999999999988898, -111.2113248654051887 ) ) ;
#11243 = CYLINDRICAL_SURFACE ( 'NONE', #15291, 5.500000000000000000 ) ;
#11244 = CARTESIAN_POINT ( 'NONE',  ( 4.763139720814407951, -2.749999999999988454, -120.5000000000000568 ) ) ;
#11245 = CARTESIAN_POINT ( 'NONE',  ( -6.000000000000000888, 1.067854986875958443E-15, 7.560779664488942560E-35 ) ) ;
#11246 = CARTESIAN_POINT ( 'NONE',  ( 154.5863248654052313, 0.000000000000000000, 5.500000000000005329 ) ) ;
#11247 = VERTEX_POINT ( 'NONE', #12172 ) ;
#11248 = CARTESIAN_POINT ( 'NONE',  ( 20.75000000000012790, 1.873492889145011997, 1.873492889144845464 ) ) ;
#11249 = CARTESIAN_POINT ( 'NONE',  ( 135.0000000000000000, 1.949781249179272091, -5.142796231657337458 ) ) ;
#11250 = CARTESIAN_POINT ( 'NONE',  ( 6.000000000000000888, -3.330669073875464691E-16, -7.560779664488942560E-35 ) ) ;
#11251 = CARTESIAN_POINT ( 'NONE',  ( 139.4211002691896795, -4.999999999999989342, -2.071067811865468400 ) ) ;
#11252 = ORIENTED_EDGE ( 'NONE', *, *, #16785, .T. ) ;
#11253 = CARTESIAN_POINT ( 'NONE',  ( 111.7497167782375129, 1.308140751793751555, 1.308140751793973600 ) ) ;
#11254 = CARTESIAN_POINT ( 'NONE',  ( 6.000000000000000888, -1.607695154586752384, -114.7306624327026157 ) ) ;
#11255 = CARTESIAN_POINT ( 'NONE',  ( 111.9372167782374703, -0.7662911109077388261, 1.849990392679652151 ) ) ;
#11256 = CARTESIAN_POINT ( 'NONE',  ( 3.608439182435180470, -6.249999999999997335, -117.1919872981078470 ) ) ;
#11257 = EDGE_CURVE ( 'NONE', #12739, #15355, #18835, .T. ) ;
#11258 = CARTESIAN_POINT ( 'NONE',  ( 140.5000000000000284, -10.99818166789400919, -4.800000000000004263 ) ) ;
#11259 = ADVANCED_FACE ( 'NONE', ( #300 ), #30411, .T. ) ;
#11260 = CARTESIAN_POINT ( 'NONE',  ( 10.00000000000014744, 1.738740874279711246, 1.328116326731191510 ) ) ;
#11261 = ORIENTED_EDGE ( 'NONE', *, *, #5654, .T. ) ;
#11262 = VERTEX_POINT ( 'NONE', #7067 ) ;
#11263 = CARTESIAN_POINT ( 'NONE',  ( 21.46132486540527751, 5.551115123125782702E-14, -2.500000000000002220 ) ) ;
#11264 = CARTESIAN_POINT ( 'NONE',  ( 142.3125000000000284, 4.242640687119298093, -4.242640687119298093 ) ) ;
#11265 = VERTEX_POINT ( 'NONE', #16479 ) ;
#11266 = CARTESIAN_POINT ( 'NONE',  ( 7.216878364870455975, -6.409875621278545621E-14, -149.9419872981078186 ) ) ;
#11267 = ORIENTED_EDGE ( 'NONE', *, *, #16161, .T. ) ;
#11268 = CARTESIAN_POINT ( 'NONE',  ( 23.31250000000007461, -0.8284271247460552878, 2.000000000000091926 ) ) ;
#11269 = CYLINDRICAL_SURFACE ( 'NONE', #27440, 2.499999999999999112 ) ;
#11270 = CARTESIAN_POINT ( 'NONE',  ( 105.0863248654051318, -1.414213562373034527, 1.414213562373145550 ) ) ;
#11271 = CARTESIAN_POINT ( 'NONE',  ( 2.775557561562891351E-14, -6.250000000000061284, -64.18301270189225249 ) ) ;
#11272 = CARTESIAN_POINT ( 'NONE',  ( 134.9486760519935444, -8.594915014407842335, -8.000000000000007105 ) ) ;
#11273 = CARTESIAN_POINT ( 'NONE',  ( 142.6726497308104342, -5.000000000000004441, 0.000000000000000000 ) ) ;
#11274 = CARTESIAN_POINT ( 'NONE',  ( 112.2886751345947118, 2.000000000000112799, 3.330669073875469621E-13 ) ) ;
#11275 = DIRECTION ( 'NONE',  ( -7.147005652999508048E-36, 5.642372883946980038E-36, 1.000000000000000000 ) ) ;
#11276 = CARTESIAN_POINT ( 'NONE',  ( 5.196152422706629359, -2.999999999999988898, -155.2886751345948824 ) ) ;
#11277 = CARTESIAN_POINT ( 'NONE',  ( 12.53867513459494631, 1.110223024625156540E-13, 2.500000000000002220 ) ) ;
#11278 = CARTESIAN_POINT ( 'NONE',  ( 5.999999999999949374, 1.607695154586804565, -115.5193375672974412 ) ) ;
#11279 = CARTESIAN_POINT ( 'NONE',  ( 108.8124999999997442, 1.035533905932839227, -2.499999999999964473 ) ) ;
#11280 = CARTESIAN_POINT ( 'NONE',  ( 106.6636751345947829, -1.414213562373090038, 1.414213562373145550 ) ) ;
#11281 = STYLED_ITEM ( 'NONE', ( #20929 ), #25858 ) ;
#11282 = CARTESIAN_POINT ( 'NONE',  ( -4.763139720814407951, 2.749999999999946709, -125.7500000000000284 ) ) ;
#11283 = CARTESIAN_POINT ( 'NONE',  ( 6.000000000000000888, 1.743066579297358182E-13, -92.16367513459482552 ) ) ;
#11284 = CARTESIAN_POINT ( 'NONE',  ( -3.608439182435052128, -6.250000000000110134, -145.3080127018922383 ) ) ;
#11285 = CARTESIAN_POINT ( 'NONE',  ( -6.000000000000000888, 1.067854986875958443E-15, 7.560779664488942560E-35 ) ) ;
#11286 = ORIENTED_EDGE ( 'NONE', *, *, #2588, .T. ) ;
#11287 = CARTESIAN_POINT ( 'NONE',  ( -4.763139720814407951, -2.750000000000016431, -56.49999999999999289 ) ) ;
#11288 = FACE_OUTER_BOUND ( 'NONE', #7095, .T. ) ;
#11289 = DIRECTION ( 'NONE',  ( -0.000000000000000000, -0.000000000000000000, -1.000000000000000000 ) ) ;
#11290 = ORIENTED_EDGE ( 'NONE', *, *, #8658, .T. ) ;
#11291 = CARTESIAN_POINT ( 'NONE',  ( 106.6249999999999289, -1.767766952966376426, -1.767766952966320915 ) ) ;
#11292 = CARTESIAN_POINT ( 'NONE',  ( 146.7187500000000284, 2.485281374238556218, -6.000000000000005329 ) ) ;
#11293 = CARTESIAN_POINT ( 'NONE',  ( 159.8704966968991243, -12.37217944490604360, -3.496373867771979782 ) ) ;
#11294 = CARTESIAN_POINT ( 'NONE',  ( 13.50000000000015099, -1.999999999999890754, -5.551115123125782702E-14 ) ) ;
#11295 = CARTESIAN_POINT ( 'NONE',  ( 140.5384615384615756, -11.53846153846155254, -4.807692307692318145 ) ) ;
#11296 = EDGE_CURVE ( 'NONE', #2328, #17215, #27395, .T. ) ;
#11297 = CARTESIAN_POINT ( 'NONE',  ( 136.6875000000000284, 4.242640687119269671, 4.242640687119298093 ) ) ;
#11298 = CARTESIAN_POINT ( 'NONE',  ( 119.6249999999999716, -1.767766952966404181, -1.767766952966320915 ) ) ;
#11299 = VECTOR ( 'NONE', #20500, 1000.000000000000000 ) ;
#11300 = CARTESIAN_POINT ( 'NONE',  ( 0.000000000000000000, 5.499999999999991118, -136.5000000000000000 ) ) ;
#11301 = CIRCLE ( 'NONE', #6857, 1.000000000000000000 ) ;
#11302 = ORIENTED_EDGE ( 'NONE', *, *, #14781, .F. ) ;
#11303 = CARTESIAN_POINT ( 'NONE',  ( 13.50000000000015099, -1.999999999999890754, -5.551115123125782702E-14 ) ) ;
#11304 = ORIENTED_EDGE ( 'NONE', *, *, #12034, .F. ) ;
#11305 = CARTESIAN_POINT ( 'NONE',  ( -4.763139720814407951, 2.749999999999946709, -65.75000000000002842 ) ) ;
#11306 = B_SPLINE_CURVE_WITH_KNOTS ( 'NONE', 3,
 ( #25703, #14522, #12075, #9587, #26003, #49, #2950, #24004, #21413, #346 ),
 .UNSPECIFIED., .F., .F.,
 ( 4, 2, 2, 2, 4 ),
 ( 0.000000000000000000, 0.0004268114089743834153, 0.0008536228179487668306, 0.001280434226923150192, 0.001707245635897533228 ),
 .UNSPECIFIED. ) ;
#11307 = LINE ( 'NONE', #4042, #19969 ) ;
#11308 = CARTESIAN_POINT ( 'NONE',  ( -3.608439182435115633, 6.249999999999965361, -90.30801270189225249 ) ) ;
#11309 =( BOUNDED_CURVE ( )  B_SPLINE_CURVE ( 2, ( #27116, #8390, #11185, #20534, #17798, #24826, #3773, #22538, #3917 ),
 .UNSPECIFIED., .F., .T. ) 
 B_SPLINE_CURVE_WITH_KNOTS ( ( 3, 2, 2, 2, 3 ),
 ( 0.8194444444444445308, 0.8203703703703704164, 0.8222222222222221877, 0.8240740740740740700, 0.8249999999999999556 ),
 .UNSPECIFIED. ) 
 CURVE ( )  GEOMETRIC_REPRESENTATION_ITEM ( )  RATIONAL_B_SPLINE_CURVE ( ( 0.9330127018922194093, 0.9330127018922234061, 1.000000000000000000, 0.8660254037844388186, 1.000000000000000000, 0.8660254037844388186, 1.000000000000000000, 0.9330127018922234061, 0.9330127018922194093 ) ) 
 REPRESENTATION_ITEM ( '' )  );
#11310 = CARTESIAN_POINT ( 'NONE',  ( 105.0386751345947971, 2.775557561562891351E-14, -2.000000000000001776 ) ) ;
#11311 = DIRECTION ( 'NONE',  ( -7.147005652999508048E-36, 5.642372883946980038E-36, 1.000000000000000000 ) ) ;
#11312 = DIRECTION ( 'NONE',  ( 1.000000000000000000, 6.938893903907222067E-15, 0.000000000000000000 ) ) ;
#11313 = DIRECTION ( 'NONE',  ( -7.147005652999508048E-36, 5.642372883946980038E-36, 1.000000000000000000 ) ) ;
#11314 = CARTESIAN_POINT ( 'NONE',  ( 118.8752832217621460, -1.849990392679384810, 2.220446049250313081E-13 ) ) ;
#11315 =( NAMED_UNIT ( * ) SI_UNIT ( $, .STERADIAN. ) SOLID_ANGLE_UNIT ( ) );
#11316 = CARTESIAN_POINT ( 'NONE',  ( 4.763139720814407951, 2.750000000000002665, -151.7500000000000568 ) ) ;
#11317 = CARTESIAN_POINT ( 'NONE',  ( 6.055081547227420202, 8.369191085434727264E-16, 12.50000000000003375 ) ) ;
#11318 = CARTESIAN_POINT ( 'NONE',  ( -3.175426480542816510, -5.500000000000057732, -141.8750000000000568 ) ) ;
#11319 = CARTESIAN_POINT ( 'NONE',  ( 5.412658773652712085, -3.125000000000086153, -161.4330127018922667 ) ) ;
#11320 = CARTESIAN_POINT ( 'NONE',  ( -0.5043617743979548207, -9.495638225601934934, 4.110987936241946805 ) ) ;
#11321 = CARTESIAN_POINT ( 'NONE',  ( 0.000000000000000000, 0.000000000000000000, 0.000000000000000000 ) ) ;
#11322 = ADVANCED_FACE ( 'NONE', ( #3442 ), #1147, .T. ) ;
#11323 = CARTESIAN_POINT ( 'NONE',  ( 4.763139720814407951, 2.750000000000002665, -76.74999999999998579 ) ) ;
#11324 = LINE ( 'NONE', #17930, #27700 ) ;
#11325 = CARTESIAN_POINT ( 'NONE',  ( 3.175426480543072749, -5.500000000000105693, -72.62500000000005684 ) ) ;
#11326 = CARTESIAN_POINT ( 'NONE',  ( 147.9523502691896510, 0.000000000000000000, 5.000000000000004441 ) ) ;
#11327 = CARTESIAN_POINT ( 'NONE',  ( -5.999999999999963585, 1.780251999655701777E-13, -64.41367513459483973 ) ) ;
#11328 = CARTESIAN_POINT ( 'NONE',  ( -5.196152422706573404, -3.000000000000002665, -71.78867513459485394 ) ) ;
#11329 = CARTESIAN_POINT ( 'NONE',  ( 144.1800748654052597, -2.278174593051981223, 5.500000000000041744 ) ) ;
#11330 = CARTESIAN_POINT ( 'NONE',  ( 19.43750000000013145, -1.999999999999851674, 0.8284271247462354770 ) ) ;
#11331 = AXIS2_PLACEMENT_3D ( 'NONE', #15079, #12951, #19974 ) ;
#11332 = CARTESIAN_POINT ( 'NONE',  ( -5.999999999999971578, 1.607695154586715303, -118.4806624327026299 ) ) ;
#11333 = CARTESIAN_POINT ( 'NONE',  ( 116.3747167782375840, 5.551115123125782702E-14, -1.849990392679190521 ) ) ;
#11334 = CARTESIAN_POINT ( 'NONE',  ( 3.464101615137852974, 5.999999999999884537, -139.3363248654051745 ) ) ;
#11335 = EDGE_CURVE ( 'NONE', #1220, #28323, #15902, .T. ) ;
#11336 = ORIENTED_EDGE ( 'NONE', *, *, #20032, .F. ) ;
#11337 = CARTESIAN_POINT ( 'NONE',  ( 153.3750000000000284, 0.000000000000000000, 6.000000000000005329 ) ) ;
#11338 = CARTESIAN_POINT ( 'NONE',  ( 6.000000000000014211, -1.607695154586730180, -156.7306624327026157 ) ) ;
#11339 = CARTESIAN_POINT ( 'NONE',  ( 117.9377832217621744, -1.849990392679441875, -0.7662911109075883909 ) ) ;
#11340 = CARTESIAN_POINT ( 'NONE',  ( 5.196152422706629359, 3.000000000000002665, -179.9613248654052313 ) ) ;
#11341 = ORIENTED_EDGE ( 'NONE', *, *, #21025, .T. ) ;
#11342 = VERTEX_POINT ( 'NONE', #18232 ) ;
#11343 = EDGE_LOOP ( 'NONE', ( #22230, #2880, #3376, #29173 ) ) ;
#11344 = CARTESIAN_POINT ( 'NONE',  ( -2.775557561562891351E-14, -5.500000000000115463, -95.25000000000000000 ) ) ;
#11345 = CARTESIAN_POINT ( 'NONE',  ( 2.775557561562891351E-14, 6.250000000000033751, -103.9330127018922525 ) ) ;
#11346 = ORIENTED_EDGE ( 'NONE', *, *, #14818, .T. ) ;
#11347 = VECTOR ( 'NONE', #25662, 1000.000000000000000 ) ;
#11348 = CARTESIAN_POINT ( 'NONE',  ( 140.5000000000000284, -9.510965941585999062, -7.318712077885313860 ) ) ;
#11349 = CARTESIAN_POINT ( 'NONE',  ( 0.7660981036491463225, -15.49911073742189416, 8.125819281016111617 ) ) ;
#11350 = CARTESIAN_POINT ( 'NONE',  ( 3.175426480543072749, -5.500000000000105693, -162.6250000000000284 ) ) ;
#11351 = CARTESIAN_POINT ( 'NONE',  ( -5.999999999999963585, 1.780251999655701777E-13, -63.83632486540523132 ) ) ;
#11352 = VERTEX_POINT ( 'NONE', #10547 ) ;
#11353 = CARTESIAN_POINT ( 'NONE',  ( 0.000000000000000000, 0.000000000000000000, 0.000000000000000000 ) ) ;
#11354 = B_SPLINE_CURVE_WITH_KNOTS ( 'NONE', 3,
 ( #24796, #22200, #15630, #15470, #17458, #29704, #27388, #1602, #22045, #13177, #983, #8513 ),
 .UNSPECIFIED., .F., .F.,
 ( 4, 2, 2, 2, 2, 4 ),
 ( 0.000000000000000000, 0.0002876650772533674311, 0.0005753301545067348623, 0.001150660309013472760, 0.001725990463520215212, 0.002301320618026957664 ),
 .UNSPECIFIED. ) ;
#11355 = CARTESIAN_POINT ( 'NONE',  ( -3.175426480542816066, 5.499999999999865885, -170.8750000000000853 ) ) ;
#11356 = CARTESIAN_POINT ( 'NONE',  ( 139.5000000000000000, -8.798545334315205579, 8.160000000000000142 ) ) ;
#11357 = CARTESIAN_POINT ( 'NONE',  ( -2.775557561562891351E-14, -5.500000000000115463, -165.7500000000000000 ) ) ;
#11358 = CARTESIAN_POINT ( 'NONE',  ( 114.3124999999997726, -1.035533905932719101, 2.500000000000205169 ) ) ;
#11359 = ADVANCED_FACE ( 'NONE', ( #8210 ), #6526, .F. ) ;
#11360 =( BOUNDED_CURVE ( )  B_SPLINE_CURVE ( 2, ( #5591, #14995, #10707, #3748, #8839, #24645, #24800, #20356, #29396 ),
 .UNSPECIFIED., .F., .F. ) 
 B_SPLINE_CURVE_WITH_KNOTS ( ( 3, 2, 2, 2, 3 ),
 ( 0.2968750000000000000, 0.3046875000000000000, 0.3125000000000000000, 0.3203125000000000000, 0.3281250000000000000 ),
 .UNSPECIFIED. ) 
 CURVE ( )  GEOMETRIC_REPRESENTATION_ITEM ( )  RATIONAL_B_SPLINE_CURVE ( ( 1.000000000000000000, 0.9238795325112867385, 1.000000000000000000, 0.9238795325112867385, 1.000000000000000000, 0.9238795325112867385, 1.000000000000000000, 0.9238795325112867385, 1.000000000000000000 ) ) 
 REPRESENTATION_ITEM ( '' )  );
#11361 = CARTESIAN_POINT ( 'NONE',  ( -4.763139720814407951, -2.750000000000016431, -111.9999999999999858 ) ) ;
#11362 = CARTESIAN_POINT ( 'NONE',  ( -5.999999999999962697, 3.323446944526963260E-14, -159.8363248654052597 ) ) ;
#11363 = CARTESIAN_POINT ( 'NONE',  ( 146.0550748654052313, -5.500000000000012434, -2.278174593052012309 ) ) ;
#11364 = CARTESIAN_POINT ( 'NONE',  ( 4.763139720814407951, -2.749999999999988454, -95.00000000000002842 ) ) ;
#11365 =( NAMED_UNIT ( * ) PLANE_ANGLE_UNIT ( ) SI_UNIT ( $, .RADIAN. ) );
#11366 = CARTESIAN_POINT ( 'NONE',  ( 0.7618037995490587466, -15.57909779039840181, 7.971327808482444155 ) ) ;
#11367 = ORIENTED_EDGE ( 'NONE', *, *, #23697, .F. ) ;
#11368 = CARTESIAN_POINT ( 'NONE',  ( 115.9999999999998153, 2.500000000000002220, 2.220446049250313081E-13 ) ) ;
#11369 = LINE ( 'NONE', #15414, #24192 ) ;
#11370 = VECTOR ( 'NONE', #28776, 1000.000000000000000 ) ;
#11371 = CARTESIAN_POINT ( 'NONE',  ( 105.7502832217622597, -1.308140751793557266, 1.308140751793751555 ) ) ;
#11372 = EDGE_CURVE ( 'NONE', #27983, #25655, #13334, .T. ) ;
#11373 = CARTESIAN_POINT ( 'NONE',  ( 6.000000000000052403, -1.607695154586662678, -85.65331216351297883 ) ) ;
#11374 = AXIS2_PLACEMENT_3D ( 'NONE', #1958, #20708, #8724 ) ;
#11375 = VERTEX_POINT ( 'NONE', #8692 ) ;
#11376 = CIRCLE ( 'NONE', #25560, 4.000000000000010658 ) ;
#11377 = CARTESIAN_POINT ( 'NONE',  ( 108.9997167782375698, -1.308140751793612777, 1.308140751793640533 ) ) ;
#11378 = CIRCLE ( 'NONE', #9394, 1.000000000000000000 ) ;
#11379 = CARTESIAN_POINT ( 'NONE',  ( -5.412658773652684552, -3.125000000000099920, -90.56698729810786119 ) ) ;
#11380 = ORIENTED_EDGE ( 'NONE', *, *, #26482, .T. ) ;
#11381 = PRESENTATION_LAYER_ASSIGNMENT (  '', '', ( #25574 ) ) ;
#11382 = CARTESIAN_POINT ( 'NONE',  ( 149.9062500000000568, 6.000000000000005329, -2.485281374238555774 ) ) ;
#11383 = ORIENTED_EDGE ( 'NONE', *, *, #14195, .T. ) ;
#11384 = CARTESIAN_POINT ( 'NONE',  ( -3.175426480542816510, -5.500000000000057732, -125.3749999999999858 ) ) ;
#11385 = CARTESIAN_POINT ( 'NONE',  ( 23.93750000000015277, -2.649519052838178457, -1.097466725451559322 ) ) ;
#11386 = CARTESIAN_POINT ( 'NONE',  ( 3.608439182435180470, 6.249999999999982236, -128.0580127018922383 ) ) ;
#11387 = ORIENTED_EDGE ( 'NONE', *, *, #7474, .F. ) ;
#11388 = CARTESIAN_POINT ( 'NONE',  ( 0.000000000000000000, 5.999999999999977796, -160.7886751345948255 ) ) ;
#11389 = CARTESIAN_POINT ( 'NONE',  ( -3.608439182435115633, 6.249999999999965361, -168.9419872981078186 ) ) ;
#11390 = CARTESIAN_POINT ( 'NONE',  ( 3.608439182435180470, 6.249999999999982236, -173.6919872981077901 ) ) ;
#11391 = FACE_OUTER_BOUND ( 'NONE', #11027, .T. ) ;
#11392 = AXIS2_PLACEMENT_3D ( 'NONE', #4781, #6635, #27959 ) ;
#11393 = CARTESIAN_POINT ( 'NONE',  ( 13.18750000000006750, 0.8284271247462955401, 2.000000000000031530 ) ) ;
#11394 = CYLINDRICAL_SURFACE ( 'NONE', #10840, 2.000000000000012879 ) ;
#11395 = DIRECTION ( 'NONE',  ( -7.147005652999508048E-36, 5.642372883946980038E-36, 1.000000000000000000 ) ) ;
#11396 = DIRECTION ( 'NONE',  ( 1.779758311459930738E-16, 1.000000000000000000, -5.642372883946978702E-36 ) ) ;
#11397 = CARTESIAN_POINT ( 'NONE',  ( 111.1252832217622597, -5.551115123125782702E-14, -1.849990392679523588 ) ) ;
#11398 = CARTESIAN_POINT ( 'NONE',  ( -7.216878364870328078, 0.000000000000000000, -75.69198729810783277 ) ) ;
#11399 = VECTOR ( 'NONE', #24087, 1000.000000000000000 ) ;
#11400 = CARTESIAN_POINT ( 'NONE',  ( -3.608439182435115633, 6.249999999999965361, -57.94198729810781145 ) ) ;
#11401 = CARTESIAN_POINT ( 'NONE',  ( -3.175426480542816510, 5.499999999999865885, -50.87500000000001421 ) ) ;
#11402 = CARTESIAN_POINT ( 'NONE',  ( -9.757819552369539906E-16, -9.500000000000008882, -5.000000000000004441 ) ) ;
#11403 = ADVANCED_FACE ( 'NONE', ( #15333 ), #17786, .T. ) ;
#11404 = CARTESIAN_POINT ( 'NONE',  ( -5.999999999999904965, -1.607695154586834541, -123.7693375672974554 ) ) ;
#11405 = DIRECTION ( 'NONE',  ( 0.000000000000000000, 0.000000000000000000, 1.000000000000000000 ) ) ;
#11406 =( BOUNDED_CURVE ( )  B_SPLINE_CURVE ( 2, ( #24721, #27015, #17689, #1372, #13250, #29158, #8758, #27456, #15553 ),
 .UNSPECIFIED., .F., .T. ) 
 B_SPLINE_CURVE_WITH_KNOTS ( ( 3, 2, 2, 2, 3 ),
 ( 0.7527777777777777679, 0.7537037037037037646, 0.7555555555555555358, 0.7574074074074074181, 0.7583333333333333037 ),
 .UNSPECIFIED. ) 
 CURVE ( )  GEOMETRIC_REPRESENTATION_ITEM ( )  RATIONAL_B_SPLINE_CURVE ( ( 0.9330127018922194093, 0.9330127018922154125, 1.000000000000000000, 0.8660254037844388186, 1.000000000000000000, 0.8660254037844388186, 1.000000000000000000, 0.9330127018922234061, 0.9330127018922194093 ) ) 
 REPRESENTATION_ITEM ( '' )  );
#11407 = CARTESIAN_POINT ( 'NONE',  ( -6.350852961085760029, -1.281975124255709124E-13, -118.1250000000000142 ) ) ;
#11408 = CARTESIAN_POINT ( 'NONE',  ( 6.350852961086080661, -9.614813431917819062E-14, -154.8750000000000000 ) ) ;
#11409 = AXIS2_PLACEMENT_3D ( 'NONE', #18318, #27631, #23064 ) ;
#11410 = ORIENTED_EDGE ( 'NONE', *, *, #22789, .F. ) ;
#11411 = CARTESIAN_POINT ( 'NONE',  ( 22.56250000000008527, 2.649519052838478661, -1.097466725451499370 ) ) ;
#11412 = AXIS2_PLACEMENT_3D ( 'NONE', #28902, #20176, #18311 ) ;
#11413 = DIRECTION ( 'NONE',  ( -1.000000000000000000, -1.665334536937736783E-16, -2.220446049250315546E-16 ) ) ;
#11414 = EDGE_CURVE ( 'NONE', #10456, #18174, #3088, .T. ) ;
#11415 = CARTESIAN_POINT ( 'NONE',  ( 136.1398502691896510, -3.535533905932752852, 3.535533905932725318 ) ) ;
#11416 = EDGE_LOOP ( 'NONE', ( #19181, #7503, #30039, #13377 ) ) ;
#11417 = CIRCLE ( 'NONE', #26082, 12.50000000000000178 ) ;
#11418 = CARTESIAN_POINT ( 'NONE',  ( 111.2497167782375982, -1.308140751793640533, -1.308140751793640533 ) ) ;
#11419 = CARTESIAN_POINT ( 'NONE',  ( 141.0000000000000284, -54.99999999999989342, 4.000000000000003553 ) ) ;
#11420 = CARTESIAN_POINT ( 'NONE',  ( 111.9997167782376550, -1.308140751793640533, 1.308140751793640533 ) ) ;
#11421 = CARTESIAN_POINT ( 'NONE',  ( 3.608439182435180470, 6.249999999999982236, -107.6919872981077901 ) ) ;
#11422 = CARTESIAN_POINT ( 'NONE',  ( -5.999999999999919176, 1.607695154586804565, -107.9806624327026299 ) ) ;
#11423 = DIRECTION ( 'NONE',  ( -8.326672684688675286E-17, -2.081668171172168821E-17, 1.000000000000000000 ) ) ;
#11424 = ORIENTED_EDGE ( 'NONE', *, *, #23392, .F. ) ;
#11425 = ORIENTED_EDGE ( 'NONE', *, *, #25577, .T. ) ;
#11426 = CARTESIAN_POINT ( 'NONE',  ( 21.96132486540530593, 1.665334536937734811E-13, 2.499999999999946709 ) ) ;
#11427 = CARTESIAN_POINT ( 'NONE',  ( 139.0312500000000853, -2.485281374238555774, -6.000000000000005329 ) ) ;
#11428 = CARTESIAN_POINT ( 'NONE',  ( 3.608439182435180470, -6.249999999999997335, -49.69198729810783988 ) ) ;
#11429 = ORIENTED_EDGE ( 'NONE', *, *, #21685, .T. ) ;
#11430 = CARTESIAN_POINT ( 'NONE',  ( 7.216878364870455975, -6.409875621278545621E-14, -137.9419872981078186 ) ) ;
#11431 = CARTESIAN_POINT ( 'NONE',  ( 18.97617513459490723, -1.035533905932568999, -2.499999999999964473 ) ) ;
#11432 = CARTESIAN_POINT ( 'NONE',  ( -5.999999999999971578, 1.607695154586715303, -150.9033121635130499 ) ) ;
#11433 = CARTESIAN_POINT ( 'NONE',  ( 23.93750000000006750, 2.000000000000151879, -0.8284271247462955401 ) ) ;
#11434 = CARTESIAN_POINT ( 'NONE',  ( 6.000000000000000888, 1.607695154586715303, -120.5966878364870212 ) ) ;
#11435 = CARTESIAN_POINT ( 'NONE',  ( -5.412658773652684552, -3.125000000000099920, -64.43301270189222407 ) ) ;
#11436 = CARTESIAN_POINT ( 'NONE',  ( 134.9273262448178627, -7.354674723950151538, -8.000000000000007105 ) ) ;
#11437 = CARTESIAN_POINT ( 'NONE',  ( 142.1101497308104058, 3.535533905932725318, 3.535533905932725318 ) ) ;
#11438 = CYLINDRICAL_SURFACE ( 'NONE', #12396, 12.00000000000000178 ) ;
#11439 = CARTESIAN_POINT ( 'NONE',  ( 3.464101615137757051, -5.999999999999979572, -160.8363248654052313 ) ) ;
#11440 = CARTESIAN_POINT ( 'NONE',  ( -2.081668171172168020E-16, -5.204170427930420051E-17, 2.499999999999999112 ) ) ;
#11441 = FACE_OUTER_BOUND ( 'NONE', #24147, .T. ) ;
#11442 = CARTESIAN_POINT ( 'NONE',  ( 6.000000000000000888, -1.859271017917181981E-14, -115.5863248654052171 ) ) ;
#11443 = CARTESIAN_POINT ( 'NONE',  ( 108.7499999999998579, 8.326672684688674053E-14, -2.499999999999835687 ) ) ;
#11444 = EDGE_CURVE ( 'NONE', #3959, #18433, #19793, .T. ) ;
#11445 = CARTESIAN_POINT ( 'NONE',  ( 2.000000000000003109, -1.110223024625156540E-16, -2.520259888162984417E-35 ) ) ;
#11446 = EDGE_CURVE ( 'NONE', #9337, #13233, #21159, .T. ) ;
#11447 = CARTESIAN_POINT ( 'NONE',  ( 4.763139720814407951, 2.750000000000002665, -120.2500000000000284 ) ) ;
#11448 = CARTESIAN_POINT ( 'NONE',  ( 3.464101615137757051, -5.999999999999979572, -92.41367513459485394 ) ) ;
#11449 = CARTESIAN_POINT ( 'NONE',  ( -3.608439182435115633, 6.249999999999965361, -142.8080127018922383 ) ) ;
#11450 = CYLINDRICAL_SURFACE ( 'NONE', #23853, 5.500000000000000000 ) ;
#11451 = EDGE_LOOP ( 'NONE', ( #29384, #23643, #5502, #10491 ) ) ;
#11452 = CARTESIAN_POINT ( 'NONE',  ( -2.775557561562891351E-14, -5.500000000000115463, -56.25000000000002132 ) ) ;
#11453 = CARTESIAN_POINT ( 'NONE',  ( 5.999999999999999112, 2.951592740943527306E-14, -154.5863248654052029 ) ) ;
#11454 = DIRECTION ( 'NONE',  ( 0.000000000000000000, 1.000000000000000000, -0.000000000000000000 ) ) ;
#11455 = LINE ( 'NONE', #25842, #13128 ) ;
#11456 = ORIENTED_EDGE ( 'NONE', *, *, #4870, .F. ) ;
#11457 = CARTESIAN_POINT ( 'NONE',  ( 107.3124999999996589, -1.035533905932598975, 2.500000000000205169 ) ) ;
#11458 = CARTESIAN_POINT ( 'NONE',  ( 139.0312500000000568, -2.485281374238556218, -6.000000000000005329 ) ) ;
#11459 = CARTESIAN_POINT ( 'NONE',  ( 160.0398553692754149, -11.61772494185188265, -3.016142447635661306 ) ) ;
#11460 = CARTESIAN_POINT ( 'NONE',  ( 6.000000000000000888, 1.743066579297358182E-13, -91.58632486540523132 ) ) ;
#11461 = CARTESIAN_POINT ( 'NONE',  ( 138.0000000000000284, 6.000000000000005329, 0.000000000000000000 ) ) ;
#11462 = DIRECTION ( 'NONE',  ( 0.000000000000000000, 0.000000000000000000, 1.000000000000000000 ) ) ;
#11463 = EDGE_LOOP ( 'NONE', ( #22020, #29832, #5800, #29454, #24920, #13597, #2287, #27151, #8422, #21400, #26362, #28471, #16967, #23270, #8499, #15459, #11062 ) ) ;
#11464 = CARTESIAN_POINT ( 'NONE',  ( 4.763139720814407951, -2.749999999999988454, -141.5000000000000284 ) ) ;
#11465 = ORIENTED_EDGE ( 'NONE', *, *, #21231, .T. ) ;
#11466 = CARTESIAN_POINT ( 'NONE',  ( 13.43750000000012434, -1.999999999999971800, 0.8284271247462354770 ) ) ;
#11467 = ORIENTED_EDGE ( 'NONE', *, *, #24839, .F. ) ;
#11468 = CARTESIAN_POINT ( 'NONE',  ( -6.350852961085760029, -1.281975124255709124E-13, -65.62500000000002842 ) ) ;
#11469 = LINE ( 'NONE', #20814, #23898 ) ;
#11470 = CARTESIAN_POINT ( 'NONE',  ( 2.775557561562891351E-14, -6.250000000000061284, -89.68301270189226670 ) ) ;
#11471 = CARTESIAN_POINT ( 'NONE',  ( 6.000000000000052403, -1.607695154586662678, -113.2306624327025872 ) ) ;
#11472 = DIRECTION ( 'NONE',  ( 0.000000000000000000, 0.000000000000000000, -1.000000000000000000 ) ) ;
#11473 = CARTESIAN_POINT ( 'NONE',  ( 0.000000000000000000, 0.000000000000000000, -180.0000000000000568 ) ) ;
#11474 = ADVANCED_FACE ( 'NONE', ( #2527 ), #11901, .T. ) ;
#11475 = FACE_OUTER_BOUND ( 'NONE', #7629, .T. ) ;
#11476 = CARTESIAN_POINT ( 'NONE',  ( 120.6877832217621176, -0.7662911109077388261, 1.849990392679652151 ) ) ;
#11477 = CARTESIAN_POINT ( 'NONE',  ( -47.68387282962894602, 150.2326934200727919, 181.9927197319569530 ) ) ;
#11478 = ADVANCED_FACE ( 'NONE', ( #16405 ), #20677, .F. ) ;
#11479 = CARTESIAN_POINT ( 'NONE',  ( -4.763139720814407951, -2.750000000000016431, -146.5000000000000284 ) ) ;
#11480 = CARTESIAN_POINT ( 'NONE',  ( 19.41367513459493921, 1.767766952966487448, 1.767766952966098870 ) ) ;
#11481 = CARTESIAN_POINT ( 'NONE',  ( 5.412658773652712085, -3.125000000000086153, -162.9330127018922667 ) ) ;
#11482 = FACE_OUTER_BOUND ( 'NONE', #9126, .T. ) ;
#11483 = CARTESIAN_POINT ( 'NONE',  ( -6.350852961085760029, -1.281975124255709124E-13, -76.12500000000002842 ) ) ;
#11484 = CYLINDRICAL_SURFACE ( 'NONE', #20359, 6.000000000000000888 ) ;
#11485 = CARTESIAN_POINT ( 'NONE',  ( 4.763139720814407951, 2.750000000000002665, -76.74999999999998579 ) ) ;
#11486 = CARTESIAN_POINT ( 'NONE',  ( 5.999999999999999112, 2.951592740943527306E-14, -156.0863248654052597 ) ) ;
#11487 = CARTESIAN_POINT ( 'NONE',  ( 147.2023502691896510, 0.000000000000000000, -5.000000000000004441 ) ) ;
#11488 = LINE ( 'NONE', #8996, #13769 ) ;
#11489 = DIRECTION ( 'NONE',  ( 0.000000000000000000, 5.551115123125767911E-17, -1.000000000000000000 ) ) ;
#11490 = CARTESIAN_POINT ( 'NONE',  ( 156.9375000000000284, -4.242640687119298093, -4.242640687119298093 ) ) ;
#11491 = CARTESIAN_POINT ( 'NONE',  ( 13.99999999999999822, 0.000000000000000000, 0.000000000000000000 ) ) ;
#11492 = CARTESIAN_POINT ( 'NONE',  ( 3.464101615137852974, 5.999999999999884537, -94.91367513459479710 ) ) ;
#11493 = DIRECTION ( 'NONE',  ( -7.147005652999508048E-36, 5.642372883946980038E-36, 1.000000000000000000 ) ) ;
#11494 =( BOUNDED_CURVE ( )  B_SPLINE_CURVE ( 2, ( #20946, #2636, #30296, #9260, #18654, #16517, #2353, #11754, #9417 ),
 .UNSPECIFIED., .F., .T. ) 
 B_SPLINE_CURVE_WITH_KNOTS ( ( 3, 2, 2, 2, 3 ),
 ( 0.5527777777777778123, 0.5537037037037036979, 0.5555555555555555802, 0.5574074074074073515, 0.5583333333333333481 ),
 .UNSPECIFIED. ) 
 CURVE ( )  GEOMETRIC_REPRESENTATION_ITEM ( )  RATIONAL_B_SPLINE_CURVE ( ( 0.9330127018922194093, 0.9330127018922234061, 1.000000000000000000, 0.8660254037844388186, 1.000000000000000000, 0.8660254037844388186, 1.000000000000000000, 0.9330127018922154125, 0.9330127018922194093 ) ) 
 REPRESENTATION_ITEM ( '' )  );
#11495 = CARTESIAN_POINT ( 'NONE',  ( 5.412658773652739619, 3.124999999999988898, -110.8169872981078470 ) ) ;
#11496 = VERTEX_POINT ( 'NONE', #6685 ) ;
#11497 = CARTESIAN_POINT ( 'NONE',  ( 156.6562500000000284, -6.000000000000005329, 2.485281374238555774 ) ) ;
#11498 = CARTESIAN_POINT ( 'NONE',  ( -4.999999999999984013, -69.50000000000001421, 7.500000000000007105 ) ) ;
#11499 = CARTESIAN_POINT ( 'NONE',  ( 114.2502832217621602, 1.308140751793640533, -1.308140751793640533 ) ) ;
#11500 = FACE_OUTER_BOUND ( 'NONE', #16293, .T. ) ;
#11501 = ORIENTED_EDGE ( 'NONE', *, *, #28374, .F. ) ;
#11502 = VERTEX_POINT ( 'NONE', #11954 ) ;
#11503 =( BOUNDED_CURVE ( )  B_SPLINE_CURVE ( 2, ( #27270, #2102, #11509, #22696, #20848, #25597, #20379, #8713, #6242 ),
 .UNSPECIFIED., .F., .T. ) 
 B_SPLINE_CURVE_WITH_KNOTS ( ( 3, 2, 2, 2, 3 ),
 ( 0.04166666666666674068, 0.04259259259259262631, 0.04444444444444439757, 0.04629629629629627985, 0.04722222222222216548 ),
 .UNSPECIFIED. ) 
 CURVE ( )  GEOMETRIC_REPRESENTATION_ITEM ( )  RATIONAL_B_SPLINE_CURVE ( ( 0.9330127018922194093, 0.9330127018922234061, 1.000000000000000000, 0.8660254037844388186, 1.000000000000000000, 0.8660254037844388186, 1.000000000000000000, 0.9330127018922234061, 0.9330127018922194093 ) ) 
 REPRESENTATION_ITEM ( '' )  );
#11504 = ORIENTED_EDGE ( 'NONE', *, *, #24710, .T. ) ;
#11505 = ADVANCED_FACE ( 'NONE', ( #14252 ), #21281, .F. ) ;
#11506 = CARTESIAN_POINT ( 'NONE',  ( 3.175426480543072749, 5.499999999999865885, -88.62500000000001421 ) ) ;
#11507 = CARTESIAN_POINT ( 'NONE',  ( -5.412658773652739619, 3.124999999999975131, -105.1830127018922383 ) ) ;
#11508 = DIRECTION ( 'NONE',  ( -7.147005652999508048E-36, 5.642372883946980038E-36, 1.000000000000000000 ) ) ;
#11509 = CARTESIAN_POINT ( 'NONE',  ( -5.196152422706601826, 2.999999999999975131, -51.96132486540522422 ) ) ;
#11510 = CARTESIAN_POINT ( 'NONE',  ( 5.682342569962902878, -9.420267146893145593, -26.96534570410896592 ) ) ;
#11511 = ORIENTED_EDGE ( 'NONE', *, *, #8183, .F. ) ;
#11512 = CARTESIAN_POINT ( 'NONE',  ( 6.000000000000000888, 1.743066579297358182E-13, -56.16367513459481842 ) ) ;
#11513 = EDGE_CURVE ( 'NONE', #26144, #9352, #20984, .T. ) ;
#11514 = CARTESIAN_POINT ( 'NONE',  ( -2.775557561562891351E-14, -5.500000000000115463, -171.7500000000000000 ) ) ;
#11515 = DIRECTION ( 'NONE',  ( 0.000000000000000000, 0.000000000000000000, -1.000000000000000000 ) ) ;
#11516 = CARTESIAN_POINT ( 'NONE',  ( 3.175426480543072749, 5.499999999999865885, -162.1250000000000284 ) ) ;
#11517 = CARTESIAN_POINT ( 'NONE',  ( 111.4999999999998863, -2.499999999999946709, 1.110223024625156540E-13 ) ) ;
#11518 = CARTESIAN_POINT ( 'NONE',  ( 4.763139720814407951, 2.750000000000002665, -105.2500000000000142 ) ) ;
#11519 = CARTESIAN_POINT ( 'NONE',  ( 3.464101615137757051, -5.999999999999979572, -159.3363248654052313 ) ) ;
#11520 = CARTESIAN_POINT ( 'NONE',  ( -3.464101615137757051, -5.999999999999979572, -122.6636751345948113 ) ) ;
#11521 = CARTESIAN_POINT ( 'NONE',  ( -3.175426480542816510, -5.500000000000057732, -95.37500000000004263 ) ) ;
#11522 = CARTESIAN_POINT ( 'NONE',  ( 161.4523502691896510, 0.000000000000000000, 5.000000000000004441 ) ) ;
#11523 = LINE ( 'NONE', #23330, #18007 ) ;
#11524 = ORIENTED_EDGE ( 'NONE', *, *, #2956, .T. ) ;
#11525 = CARTESIAN_POINT ( 'NONE',  ( 10.31250000000007994, -1.097466725451499370, -2.649519052838358757 ) ) ;
#11526 = CARTESIAN_POINT ( 'NONE',  ( 117.1874999999997726, 1.035533905932659149, 2.500000000000205169 ) ) ;
#11527 = CARTESIAN_POINT ( 'NONE',  ( 105.5002832217622313, 1.308140751793696044, 1.308140751793640533 ) ) ;
#11528 = ORIENTED_EDGE ( 'NONE', *, *, #15719, .T. ) ;
#11529 = CARTESIAN_POINT ( 'NONE',  ( 110.2113248654050608, -1.999999999999946265, 0.000000000000000000 ) ) ;
#11530 = CARTESIAN_POINT ( 'NONE',  ( 105.9997167782375982, -1.308140751793612777, 1.308140751793640533 ) ) ;
#11531 = ORIENTED_EDGE ( 'NONE', *, *, #16481, .T. ) ;
#11532 = CARTESIAN_POINT ( 'NONE',  ( 106.9613248654050039, 1.110223024625156540E-13, 2.000000000000001776 ) ) ;
#11533 = ADVANCED_FACE ( 'NONE', ( #19285, #14678 ), #26022, .F. ) ;
#11534 = VERTEX_POINT ( 'NONE', #19436 ) ;
#11535 = CARTESIAN_POINT ( 'NONE',  ( 152.3437500000000568, -6.000000000000005329, -2.485281374238555774 ) ) ;
#11536 = ORIENTED_EDGE ( 'NONE', *, *, #29300, .F. ) ;
#11537 = EDGE_CURVE ( 'NONE', #9814, #23810, #4030, .T. ) ;
#11538 = CARTESIAN_POINT ( 'NONE',  ( -3.175426480542816510, -5.500000000000057732, -114.8749999999999858 ) ) ;
#11539 = CARTESIAN_POINT ( 'NONE',  ( 21.25000000000013145, 1.873492889145067508, -1.873492889145067508 ) ) ;
#11540 = CARTESIAN_POINT ( 'NONE',  ( -7.216878364870328078, 0.000000000000000000, -135.0580127018922667 ) ) ;
#11541 = VERTEX_POINT ( 'NONE', #5418 ) ;
#11542 = DIRECTION ( 'NONE',  ( 0.000000000000000000, 1.000000000000000000, -0.000000000000000000 ) ) ;
#11543 = CARTESIAN_POINT ( 'NONE',  ( 5.412658773652712085, -3.125000000000086153, -172.5669872981078186 ) ) ;
#11544 = CARTESIAN_POINT ( 'NONE',  ( 2.775557561562891351E-14, 6.250000000000033751, -179.5669872981078186 ) ) ;
#11545 = CARTESIAN_POINT ( 'NONE',  ( 160.0396984632319572, -11.61764268043064696, 3.016434873857221088 ) ) ;
#11546 = CARTESIAN_POINT ( 'NONE',  ( -3.464101615137725076, 5.999999999999979572, -147.1636751345947687 ) ) ;
#11547 = ORIENTED_EDGE ( 'NONE', *, *, #15605, .F. ) ;
#11548 = CARTESIAN_POINT ( 'NONE',  ( 11.50000000000006573, -1.999999999999835243, 0.000000000000000000 ) ) ;
#11549 = EDGE_CURVE ( 'NONE', #87, #13381, #20168, .T. ) ;
#11550 = DIRECTION ( 'NONE',  ( -0.000000000000000000, -0.000000000000000000, -1.000000000000000000 ) ) ;
#11551 = ADVANCED_FACE ( 'NONE', ( #14830 ), #23878, .T. ) ;
#11552 = CARTESIAN_POINT ( 'NONE',  ( 153.1949251345948539, 5.500000000000012434, -2.278174593052012309 ) ) ;
#11553 = FACE_OUTER_BOUND ( 'NONE', #26924, .T. ) ;
#11554 = DIRECTION ( 'NONE',  ( -1.000000000000000000, 1.779758311459930738E-16, 0.000000000000000000 ) ) ;
#11555 = CARTESIAN_POINT ( 'NONE',  ( -7.216878364870328078, 0.000000000000000000, -72.69198729810781856 ) ) ;
#11556 = CARTESIAN_POINT ( 'NONE',  ( -7.216878364870328078, 0.000000000000000000, -60.69198729810782567 ) ) ;
#11557 = CARTESIAN_POINT ( 'NONE',  ( -4.763139720814407951, 2.749999999999946709, -52.25000000000002132 ) ) ;
#11558 = CARTESIAN_POINT ( 'NONE',  ( -0.8691260360719468281, -9.261747927856070817, -4.026027341348647148 ) ) ;
#11559 = CARTESIAN_POINT ( 'NONE',  ( -5.196152422706573404, -3.000000000000002665, -153.7113248654052313 ) ) ;
#11560 = VECTOR ( 'NONE', #17514, 1000.000000000000000 ) ;
#11561 = CARTESIAN_POINT ( 'NONE',  ( 159.8739699821186093, -11.15087202985791848, -4.434002056370806244 ) ) ;
#11562 = CARTESIAN_POINT ( 'NONE',  ( -4.763139720814407951, 2.749999999999946709, -118.2500000000000284 ) ) ;
#11563 = CARTESIAN_POINT ( 'NONE',  ( 135.0000000000000284, -8.301012159643168076, -7.690749534758824169 ) ) ;
#11564 = CARTESIAN_POINT ( 'NONE',  ( -3.464101615137725076, 5.999999999999979572, -154.0863248654051745 ) ) ;
#11565 = ORIENTED_EDGE ( 'NONE', *, *, #28923, .F. ) ;
#11566 = CARTESIAN_POINT ( 'NONE',  ( -5.999999999999919176, 1.607695154586804565, -104.9806624327026014 ) ) ;
#11567 = VERTEX_POINT ( 'NONE', #7577 ) ;
#11568 = CARTESIAN_POINT ( 'NONE',  ( 109.0622167782374561, -1.849990392679501827, 0.7662911109077686911 ) ) ;
#11569 = FACE_OUTER_BOUND ( 'NONE', #5792, .T. ) ;
#11570 = CARTESIAN_POINT ( 'NONE',  ( 112.6247167782375271, 1.849990392679523588, 0.000000000000000000 ) ) ;
#11571 = CARTESIAN_POINT ( 'NONE',  ( 5.412658773652712085, -3.125000000000086153, -109.5669872981078186 ) ) ;
#11572 = CARTESIAN_POINT ( 'NONE',  ( 20.03867513459486815, 1.665334536937734811E-13, -2.500000000000057732 ) ) ;
#11573 = CARTESIAN_POINT ( 'NONE',  ( 110.4613248654051176, 5.551115123125782702E-14, -2.000000000000001776 ) ) ;
#11574 = ORIENTED_EDGE ( 'NONE', *, *, #15132, .F. ) ;
#11575 = CARTESIAN_POINT ( 'NONE',  ( 1.000000000000000888, 0.000000000000000000, -16.50000000000000355 ) ) ;
#11576 = CARTESIAN_POINT ( 'NONE',  ( 138.9375000000000568, -4.242640687119298093, -4.242640687119298093 ) ) ;
#11577 = EDGE_CURVE ( 'NONE', #12780, #9068, #6413, .T. ) ;
#11578 = AXIS2_PLACEMENT_3D ( 'NONE', #25627, #23344, #30380 ) ;
#11579 = CARTESIAN_POINT ( 'NONE',  ( -5.412658773652684552, -3.125000000000099920, -137.0669872981078470 ) ) ;
#11580 = CARTESIAN_POINT ( 'NONE',  ( 18.85117513459493566, -2.499999999999904521, -1.035533905932689347 ) ) ;
#11581 = DIRECTION ( 'NONE',  ( -1.000000000000000000, -1.665334536937731113E-16, 1.526556658859586792E-16 ) ) ;
#11582 = CARTESIAN_POINT ( 'NONE',  ( 22.68750000000017764, -0.8284271247460552878, -2.000000000000031530 ) ) ;
#11583 = CARTESIAN_POINT ( 'NONE',  ( 0.000000000000000000, 0.000000000000000000, 0.000000000000000000 ) ) ;
#11584 = EDGE_CURVE ( 'NONE', #14826, #27080, #4006, .T. ) ;
#11585 = FACE_OUTER_BOUND ( 'NONE', #20800, .T. ) ;
#11586 = CARTESIAN_POINT ( 'NONE',  ( 3.608439182435180470, 6.249999999999982236, -66.55801270189226670 ) ) ;
#11587 =( BOUNDED_CURVE ( )  B_SPLINE_CURVE ( 2, ( #24574, #10014, #29171, #17096, #17247, #19392, #10629, #17396, #14640 ),
 .UNSPECIFIED., .F., .F. ) 
 B_SPLINE_CURVE_WITH_KNOTS ( ( 3, 2, 2, 2, 3 ),
 ( 0.7058823529411765163, 0.7132352941176470784, 0.7205882352941176405, 0.7279411764705882026, 0.7352941176470588758 ),
 .UNSPECIFIED. ) 
 CURVE ( )  GEOMETRIC_REPRESENTATION_ITEM ( )  RATIONAL_B_SPLINE_CURVE ( ( 1.000000000000000000, 0.9238795325112867385, 1.000000000000000000, 0.9238795325112867385, 1.000000000000000000, 0.9238795325112867385, 1.000000000000000000, 0.9238795325112867385, 1.000000000000000000 ) ) 
 REPRESENTATION_ITEM ( '' )  );
#11588 = CARTESIAN_POINT ( 'NONE',  ( 135.6059727065479876, -8.864963804572132844, -8.000000000000007105 ) ) ;
#11589 = EDGE_CURVE ( 'NONE', #4075, #28330, #4970, .T. ) ;
#11590 = CARTESIAN_POINT ( 'NONE',  ( 145.2976497308104058, 0.000000000000000000, 5.000000000000004441 ) ) ;
#11591 = CARTESIAN_POINT ( 'NONE',  ( 3.464101615137852974, 5.999999999999884537, -102.4136751345948255 ) ) ;
#11592 = CARTESIAN_POINT ( 'NONE',  ( -5.196152422706573404, -3.000000000000002665, -161.2113248654052313 ) ) ;
#11593 = CARTESIAN_POINT ( 'NONE',  ( 124.9999999999999432, -69.50000000000000000, 8.000000000000007105 ) ) ;
#11594 = VECTOR ( 'NONE', #2085, 1000.000000000000000 ) ;
#11595 = CARTESIAN_POINT ( 'NONE',  ( 10.00000000000014744, 1.108974023722453239E-13, 5.999999999999945821 ) ) ;
#11596 = CARTESIAN_POINT ( 'NONE',  ( 109.3750000000000142, -1.767766952966320915, 1.767766952966431937 ) ) ;
#11597 = DIRECTION ( 'NONE',  ( -1.000000000000000000, -1.665334536937736783E-16, -2.220446049250315546E-16 ) ) ;
#11598 = CARTESIAN_POINT ( 'NONE',  ( -2.775557561562891351E-14, -5.500000000000115463, -125.2500000000000284 ) ) ;
#11599 = CARTESIAN_POINT ( 'NONE',  ( 14.35117513459479177, 2.500000000000024425, 1.035533905932689347 ) ) ;
#11600 = CARTESIAN_POINT ( 'NONE',  ( 6.000000000000000888, -1.859271017917181981E-14, -169.5863248654052029 ) ) ;
#11601 = ORIENTED_EDGE ( 'NONE', *, *, #28996, .F. ) ;
#11602 = CARTESIAN_POINT ( 'NONE',  ( -4.763139720814407951, 2.749999999999946709, -55.25000000000002132 ) ) ;
#11603 = CARTESIAN_POINT ( 'NONE',  ( -5.999999999999963585, -1.487416814333745711E-14, -123.8363248654052171 ) ) ;
#11604 = CARTESIAN_POINT ( 'NONE',  ( -5.999999999999963585, 1.780251999655701777E-13, -78.83632486540523132 ) ) ;
#11605 = CARTESIAN_POINT ( 'NONE',  ( -4.999999999999920952, -65.00000000000001421, 8.000000000000007105 ) ) ;
#11606 = AXIS2_PLACEMENT_3D ( 'NONE', #10742, #3782, #27426 ) ;
#11607 = ORIENTED_EDGE ( 'NONE', *, *, #8945, .T. ) ;
#11608 = CARTESIAN_POINT ( 'NONE',  ( 119.7497167782375556, 1.308140751793696044, 1.308140751793862577 ) ) ;
#11609 = CARTESIAN_POINT ( 'NONE',  ( 137.6250000000000284, 0.000000000000000000, -6.000000000000005329 ) ) ;
#11610 = CARTESIAN_POINT ( 'NONE',  ( 2.775557561562891351E-14, -6.250000000000061284, -102.3169872981078470 ) ) ;
#11611 = DIRECTION ( 'NONE',  ( -0.000000000000000000, -0.000000000000000000, -1.000000000000000000 ) ) ;
#11612 = CARTESIAN_POINT ( 'NONE',  ( 160.3913997308104058, -2.071067811865468400, 4.999999999999989342 ) ) ;
#11613 = CARTESIAN_POINT ( 'NONE',  ( 6.000000000000000888, -3.330669073875464691E-16, -7.560779664488942560E-35 ) ) ;
#11614 = CIRCLE ( 'NONE', #26271, 16.50000000000000355 ) ;
#11615 = EDGE_CURVE ( 'NONE', #9180, #3348, #29219, .T. ) ;
#11616 = CARTESIAN_POINT ( 'NONE',  ( -3.175426480542816510, -5.500000000000057732, -134.3750000000000284 ) ) ;
#11617 = CARTESIAN_POINT ( 'NONE',  ( 11.56250000000009237, -1.999999999999851674, -0.8284271247462354770 ) ) ;
#11618 = EDGE_LOOP ( 'NONE', ( #21552, #7742, #10767, #9343 ) ) ;
#11619 = CARTESIAN_POINT ( 'NONE',  ( 3.175426480543072749, -5.500000000000105693, -63.62500000000001421 ) ) ;
#11620 = CARTESIAN_POINT ( 'NONE',  ( 18.71132486540527751, 2.500000000000168754, -5.551115123125782702E-14 ) ) ;
#11621 = CARTESIAN_POINT ( 'NONE',  ( -5.999999999999963585, -1.487416814333745711E-14, -124.4136751345948255 ) ) ;
#11622 = EDGE_CURVE ( 'NONE', #25006, #234, #28466, .T. ) ;
#11623 = CARTESIAN_POINT ( 'NONE',  ( 3.608439182435180470, 6.249999999999982236, -89.05801270189225249 ) ) ;
#11624 = AXIS2_PLACEMENT_3D ( 'NONE', #20694, #13504, #13973 ) ;
#11625 = CARTESIAN_POINT ( 'NONE',  ( 106.1872167782374703, -1.849990392679381701, -0.7662911109075283278 ) ) ;
#11626 = CARTESIAN_POINT ( 'NONE',  ( 113.2886751345947118, 1.999999999999946265, 1.110223024625156540E-13 ) ) ;
#11627 = FACE_OUTER_BOUND ( 'NONE', #26579, .T. ) ;
#11628 = CARTESIAN_POINT ( 'NONE',  ( 117.6252832217623165, 0.000000000000000000, 1.849990392679523588 ) ) ;
#11629 = CARTESIAN_POINT ( 'NONE',  ( -6.350852961085760029, -1.281975124255709124E-13, -151.1250000000000284 ) ) ;
#11630 = CARTESIAN_POINT ( 'NONE',  ( 0.000000000000000000, 0.000000000000000000, -200.0000000000000000 ) ) ;
#11631 = CARTESIAN_POINT ( 'NONE',  ( -6.350852961085760029, -1.281975124255709124E-13, -134.6250000000000284 ) ) ;
#11632 = CARTESIAN_POINT ( 'NONE',  ( 5.412658773652739619, 3.124999999999988898, -164.1830127018922383 ) ) ;
#11633 = CYLINDRICAL_SURFACE ( 'NONE', #11109, 6.000000000000000888 ) ;
#11634 =( BOUNDED_CURVE ( )  B_SPLINE_CURVE ( 2, ( #6850, #14661, #9476, #17272, #3240, #19416, #14953, #12667, #26592 ),
 .UNSPECIFIED., .F., .F. ) 
 B_SPLINE_CURVE_WITH_KNOTS ( ( 3, 2, 2, 2, 3 ),
 ( 0.8416666666666666741, 0.8425925925925925597, 0.8444444444444444420, 0.8462962962962963243, 0.8472222222222222099 ),
 .UNSPECIFIED. ) 
 CURVE ( )  GEOMETRIC_REPRESENTATION_ITEM ( )  RATIONAL_B_SPLINE_CURVE ( ( 0.9330127018922194093, 0.9330127018922194093, 1.000000000000000000, 0.8660254037844388186, 1.000000000000000000, 0.8660254037844388186, 1.000000000000000000, 0.9330127018922194093, 0.9330127018922194093 ) ) 
 REPRESENTATION_ITEM ( '' )  );
#11635 = CARTESIAN_POINT ( 'NONE',  ( -6.350852961085760029, -1.281975124255709124E-13, -82.12500000000001421 ) ) ;
#11636 = CARTESIAN_POINT ( 'NONE',  ( -27.00000000000002487, 2.220446049250313081E-16, -4.000000000000010658 ) ) ;
#11637 = CARTESIAN_POINT ( 'NONE',  ( 4.763139720814407951, 2.750000000000002665, -64.75000000000002842 ) ) ;
#11638 = CARTESIAN_POINT ( 'NONE',  ( -5.999999999999904965, -1.607695154586834541, -156.7693375672974128 ) ) ;
#11639 = CARTESIAN_POINT ( 'NONE',  ( 150.6711002691896226, 4.999999999999989342, 2.071067811865468400 ) ) ;
#11640 = CARTESIAN_POINT ( 'NONE',  ( -3.464101615137757051, -5.999999999999979572, -114.5863248654051745 ) ) ;
#11641 = CARTESIAN_POINT ( 'NONE',  ( 9.433704689814137012, 0.000000000000000000, 0.000000000000000000 ) ) ;
#11642 = CARTESIAN_POINT ( 'NONE',  ( 159.4687500000000568, -2.485281374238585972, 6.000000000000005329 ) ) ;
#11643 = PRESENTATION_STYLE_ASSIGNMENT (( #28167 ) ) ;
#11644 = CARTESIAN_POINT ( 'NONE',  ( 18.93750000000016698, 2.000000000000091926, -0.8284271247462354770 ) ) ;
#11645 = CARTESIAN_POINT ( 'NONE',  ( 5.196152422706629359, 3.000000000000002665, -95.03867513459485394 ) ) ;
#11646 = CARTESIAN_POINT ( 'NONE',  ( 160.0000000000000284, -59.99999999999980105, 4.000000000000003553 ) ) ;
#11647 = CARTESIAN_POINT ( 'NONE',  ( 117.6247167782375840, 1.849990392679551343, 0.000000000000000000 ) ) ;
#11648 = SURFACE_STYLE_USAGE ( .BOTH. , #13960 ) ;
#11649 = EDGE_LOOP ( 'NONE', ( #18195, #25893, #24712, #2576 ) ) ;
#11650 = CARTESIAN_POINT ( 'NONE',  ( 154.9687500000000284, -2.485281374238585972, 6.000000000000005329 ) ) ;
#11651 = CARTESIAN_POINT ( 'NONE',  ( 113.3127832217621176, 1.849990392679501827, -0.7662911109077087390 ) ) ;
#11652 = PRESENTATION_LAYER_ASSIGNMENT (  '', '', ( #24836 ) ) ;
#11653 = CARTESIAN_POINT ( 'NONE',  ( -6.350852961085760029, -1.281975124255709124E-13, -154.1250000000000568 ) ) ;
#11654 = EDGE_CURVE ( 'NONE', #3053, #26392, #13896, .T. ) ;
#11655 = CARTESIAN_POINT ( 'NONE',  ( 5.453341115157027907, 2.554536117543700247, -179.9798858605075509 ) ) ;
#11656 = EDGE_LOOP ( 'NONE', ( #18060, #10144, #4912, #3420 ) ) ;
#11657 = VERTEX_POINT ( 'NONE', #5716 ) ;
#11658 = ADVANCED_FACE ( 'NONE', ( #12837 ), #11131, .T. ) ;
#11659 = VERTEX_POINT ( 'NONE', #24458 ) ;
#11660 = CARTESIAN_POINT ( 'NONE',  ( 3.175426480543072749, -5.500000000000105693, -90.62500000000001421 ) ) ;
#11661 = CARTESIAN_POINT ( 'NONE',  ( -7.216878364870328078, 0.000000000000000000, -105.0580127018922525 ) ) ;
#11662 = VERTEX_POINT ( 'NONE', #15610 ) ;
#11663 = FACE_OUTER_BOUND ( 'NONE', #20996, .T. ) ;
#11664 = CARTESIAN_POINT ( 'NONE',  ( 0.000000000000000000, -10.50000000000000888, 7.500000000000007105 ) ) ;
#11665 = AXIS2_PLACEMENT_3D ( 'NONE', #902, #10301, #15548 ) ;
#11666 = CARTESIAN_POINT ( 'NONE',  ( 6.000249633052443521, -9.219381998443749282, -24.80704692217345197 ) ) ;
#11667 = ORIENTED_EDGE ( 'NONE', *, *, #17666, .T. ) ;
#11668 = CARTESIAN_POINT ( 'NONE',  ( -5.999999999999971578, 1.607695154586715303, -92.98066243270261566 ) ) ;
#11669 = AXIS2_PLACEMENT_3D ( 'NONE', #29062, #21877, #17433 ) ;
#11670 = CARTESIAN_POINT ( 'NONE',  ( 6.350852961086080661, -9.614813431917819062E-14, -174.3750000000000284 ) ) ;
#11671 = CARTESIAN_POINT ( 'NONE',  ( 0.000000000000000000, -5.999999999999991118, -80.53867513459483973 ) ) ;
#11672 = CARTESIAN_POINT ( 'NONE',  ( 6.350852961086080661, -9.614813431917819062E-14, -156.3750000000000000 ) ) ;
#11673 = CARTESIAN_POINT ( 'NONE',  ( 114.1250000000000142, 1.767766952966293159, 1.767766952966320915 ) ) ;
#11674 = CARTESIAN_POINT ( 'NONE',  ( -5.999999999999963585, 1.780251999655701777E-13, -86.91367513459485394 ) ) ;
#11675 =( BOUNDED_SURFACE ( )  B_SPLINE_SURFACE ( 3, 2, ( 
 ( #19674, #15556, #6142 ),
 ( #12787, #15233, #22131 ),
 ( #29321, #12945, #29161 ),
 ( #10784, #10462, #1209 ) ),
 .UNSPECIFIED., .F., .F., .F. ) 
 B_SPLINE_SURFACE_WITH_KNOTS ( ( 4, 4 ),
 ( 3, 3 ),
 ( 2.710505431213761085E-18, 0.0007339382808609110857 ),
 ( 0.000000000000000000, 1.000000000000000000 ),
 .UNSPECIFIED. ) 
 GEOMETRIC_REPRESENTATION_ITEM ( )  RATIONAL_B_SPLINE_SURFACE ( (
 ( 1.000000000000000000, 0.7743236465966895077, 1.000000000000000000),
 ( 1.000000000000000000, 0.7550843754125133866, 1.000000000000000000),
 ( 1.000000000000000000, 0.7330092777270662552, 1.000000000000000000),
 ( 1.000000000000000000, 0.7071067811865475727, 1.000000000000000000) ) ) 
 REPRESENTATION_ITEM ( '' )  SURFACE ( )  );
#11676 = CARTESIAN_POINT ( 'NONE',  ( -4.763139720814407951, -2.750000000000016431, -95.50000000000002842 ) ) ;
#11677 = CARTESIAN_POINT ( 'NONE',  ( 0.1257426365907835797, -15.26923055284497366, 8.555419898867683060 ) ) ;
#11678 = ORIENTED_EDGE ( 'NONE', *, *, #29309, .T. ) ;
#11679 = CARTESIAN_POINT ( 'NONE',  ( 12.37500000000007994, 1.665334536937734811E-13, -2.649519052838500421 ) ) ;
#11680 = CARTESIAN_POINT ( 'NONE',  ( 111.6249999999998153, -1.767766952966376426, -1.767766952966431937 ) ) ;
#11681 = CARTESIAN_POINT ( 'NONE',  ( 15.60117513459495342, -1.035533905932689347, 2.499999999999904521 ) ) ;
#11682 = CARTESIAN_POINT ( 'NONE',  ( 105.0627832217622455, -0.7662911109076785410, -1.849990392679411677 ) ) ;
#11683 = CARTESIAN_POINT ( 'NONE',  ( 6.000000000000000888, -3.330669073875464691E-16, -7.560779664488942560E-35 ) ) ;
#11684 =( BOUNDED_CURVE ( )  B_SPLINE_CURVE ( 2, ( #11486, #20828, #18534, #6826, #25568, #2236, #18837, #11638, #14248 ),
 .UNSPECIFIED., .F., .T. ) 
 B_SPLINE_CURVE_WITH_KNOTS ( ( 3, 2, 2, 2, 3 ),
 ( 0.8138888888888888840, 0.8148148148148148806, 0.8166666666666666519, 0.8185185185185185341, 0.8194444444444444198 ),
 .UNSPECIFIED. ) 
 CURVE ( )  GEOMETRIC_REPRESENTATION_ITEM ( )  RATIONAL_B_SPLINE_CURVE ( ( 0.9330127018922194093, 0.9330127018922154125, 1.000000000000000000, 0.8660254037844388186, 1.000000000000000000, 0.8660254037844388186, 1.000000000000000000, 0.9330127018922234061, 0.9330127018922194093 ) ) 
 REPRESENTATION_ITEM ( '' )  );
#11685 = VERTEX_POINT ( 'NONE', #20479 ) ;
#11686 = VECTOR ( 'NONE', #28625, 1000.000000000000000 ) ;
#11687 = CARTESIAN_POINT ( 'NONE',  ( 113.9136751345947260, -1.414213562373256572, -1.414213562373034527 ) ) ;
#11688 = CARTESIAN_POINT ( 'NONE',  ( 19.99999999999998934, 0.000000000000000000, 0.000000000000000000 ) ) ;
#11689 = CARTESIAN_POINT ( 'NONE',  ( 105.3747167782376550, -5.551115123125782702E-14, -1.849990392679523588 ) ) ;
#11690 = ORIENTED_EDGE ( 'NONE', *, *, #18893, .F. ) ;
#11691 = ADVANCED_FACE ( 'NONE', ( #29684 ), #8030, .F. ) ;
#11692 = VERTEX_POINT ( 'NONE', #1112 ) ;
#11693 = CARTESIAN_POINT ( 'NONE',  ( 151.6875000000000284, 4.242640687119269671, 4.242640687119298093 ) ) ;
#11694 = VERTEX_POINT ( 'NONE', #29540 ) ;
#11695 = CARTESIAN_POINT ( 'NONE',  ( 6.350852961086080661, -9.614813431917819062E-14, -115.8750000000000000 ) ) ;
#11696 = CARTESIAN_POINT ( 'NONE',  ( 20.56250000000008171, 1.097466725451679892, 2.649519052838298805 ) ) ;
#11697 = CARTESIAN_POINT ( 'NONE',  ( 3.608439182435180470, 6.249999999999982236, -132.5580127018922383 ) ) ;
#11698 = EDGE_LOOP ( 'NONE', ( #2492, #410, #22541, #28577, #2197, #13001, #2866, #26130, #763, #25012, #10590, #8749, #2500, #15382, #18903, #16333 ) ) ;
#11699 = DIRECTION ( 'NONE',  ( 0.000000000000000000, 0.000000000000000000, -1.000000000000000000 ) ) ;
#11700 = CARTESIAN_POINT ( 'NONE',  ( -5.412658773652684552, -3.125000000000099920, -173.0669872981078186 ) ) ;
#11701 = CARTESIAN_POINT ( 'NONE',  ( 109.8749999999998437, 1.767766952966320915, -1.767766952966209892 ) ) ;
#11702 = CARTESIAN_POINT ( 'NONE',  ( 0.2138663749889929133, -15.56976101427718362, -7.989719758726499421 ) ) ;
#11703 = CARTESIAN_POINT ( 'NONE',  ( 0.000000000000000000, 5.499999999999991118, -180.0000000000000568 ) ) ;
#11704 = DIRECTION ( 'NONE',  ( 1.000000000000000000, 0.000000000000000000, 0.000000000000000000 ) ) ;
#11705 = CARTESIAN_POINT ( 'NONE',  ( 107.9377832217621886, -1.849990392679472073, -0.7662911109075283278 ) ) ;
#11706 = CARTESIAN_POINT ( 'NONE',  ( 2.775557561562891351E-14, -6.250000000000061284, -175.1830127018922383 ) ) ;
#11707 = FACE_OUTER_BOUND ( 'NONE', #8543, .T. ) ;
#11708 = CARTESIAN_POINT ( 'NONE',  ( 3.464101615137757051, -5.999999999999979572, -101.4136751345948255 ) ) ;
#11709 = PRESENTATION_LAYER_ASSIGNMENT (  '', '', ( #27832 ) ) ;
#11710 = CARTESIAN_POINT ( 'NONE',  ( 0.000000000000000000, 5.999999999999977796, -159.2886751345948255 ) ) ;
#11711 = CARTESIAN_POINT ( 'NONE',  ( -4.763139720814407951, 2.749999999999946709, -121.2500000000000284 ) ) ;
#11712 = CARTESIAN_POINT ( 'NONE',  ( -6.000000000000023093, 1.607695154586625819, -165.9033121635129646 ) ) ;
#11713 = CARTESIAN_POINT ( 'NONE',  ( 3.464101615137852974, 5.999999999999884537, -154.3363248654052029 ) ) ;
#11714 = ORIENTED_EDGE ( 'NONE', *, *, #6164, .T. ) ;
#11715 = CARTESIAN_POINT ( 'NONE',  ( 23.06250000000002487, -2.649519052838298805, 1.097466725451499370 ) ) ;
#11716 = EDGE_CURVE ( 'NONE', #22223, #4758, #22796, .T. ) ;
#11717 = CARTESIAN_POINT ( 'NONE',  ( 130.0000000000000284, -60.00000000000001421, 4.000000000000003553 ) ) ;
#11718 = DIRECTION ( 'NONE',  ( 0.000000000000000000, -2.081668171172248016E-17, 1.000000000000000000 ) ) ;
#11719 = DIRECTION ( 'NONE',  ( -7.147005652999508048E-36, 5.642372883946980038E-36, 1.000000000000000000 ) ) ;
#11720 = ORIENTED_EDGE ( 'NONE', *, *, #15265, .F. ) ;
#11721 = CARTESIAN_POINT ( 'NONE',  ( 111.0622167782374845, -1.849990392679501827, 0.7662911109078888172 ) ) ;
#11722 = CARTESIAN_POINT ( 'NONE',  ( 6.000000000000000888, 7.762456499804234384E-14, -122.1636751345948397 ) ) ;
#11723 = CARTESIAN_POINT ( 'NONE',  ( -5.412658773652739619, 3.124999999999975131, -108.8169872981078470 ) ) ;
#11724 = SURFACE_SIDE_STYLE ('',( #2324 ) ) ;
#11725 = CARTESIAN_POINT ( 'NONE',  ( -3.464101615137757051, -5.999999999999979572, -125.6636751345948113 ) ) ;
#11726 = EDGE_CURVE ( 'NONE', #11694, #27377, #13927, .T. ) ;
#11727 = CARTESIAN_POINT ( 'NONE',  ( 0.000000000000000000, 0.000000000000000000, 0.000000000000000000 ) ) ;
#11728 = STYLED_ITEM ( 'NONE', ( #12810 ), #3252 ) ;
#11729 = ORIENTED_EDGE ( 'NONE', *, *, #18026, .T. ) ;
#11730 = CARTESIAN_POINT ( 'NONE',  ( 151.9613248654052029, -5.500000000000005329, 0.000000000000000000 ) ) ;
#11731 = CARTESIAN_POINT ( 'NONE',  ( 134.6250000000000284, 0.000000000000000000, -6.000000000000005329 ) ) ;
#11732 = CARTESIAN_POINT ( 'NONE',  ( 2.775557561562891351E-14, -6.250000000000061284, -139.8169872981078186 ) ) ;
#11733 = CARTESIAN_POINT ( 'NONE',  ( -6.000000000000000888, 1.067854986875958443E-15, 7.560779664488942560E-35 ) ) ;
#11734 = CARTESIAN_POINT ( 'NONE',  ( 14.53867513459486460, 1.665334536937734811E-13, 2.499999999999835687 ) ) ;
#11735 = CARTESIAN_POINT ( 'NONE',  ( 18.75000000000015632, 1.110223024625156540E-13, -2.000000000000168310 ) ) ;
#11736 = CARTESIAN_POINT ( 'NONE',  ( -3.464101615137757051, -5.999999999999979572, -130.1636751345948539 ) ) ;
#11737 = DIRECTION ( 'NONE',  ( -7.147005652999508048E-36, 5.642372883946980038E-36, 1.000000000000000000 ) ) ;
#11738 = CARTESIAN_POINT ( 'NONE',  ( -7.216878364870328078, 0.000000000000000000, -63.05801270189225249 ) ) ;
#11739 = CARTESIAN_POINT ( 'NONE',  ( 0.000000000000000000, 0.000000000000000000, 0.000000000000000000 ) ) ;
#11740 = CARTESIAN_POINT ( 'NONE',  ( 145.7663997308104342, -4.999999999999989342, -2.071067811865468400 ) ) ;
#11741 = CARTESIAN_POINT ( 'NONE',  ( 11.53867513459497296, 5.551115123125782702E-14, 2.500000000000002220 ) ) ;
#11742 = CARTESIAN_POINT ( 'NONE',  ( 12.91367513459493210, -1.767766952966209892, -1.767766952966487448 ) ) ;
#11743 = CARTESIAN_POINT ( 'NONE',  ( -5.196152422706573404, -3.000000000000002665, -146.7886751345948255 ) ) ;
#11744 = CARTESIAN_POINT ( 'NONE',  ( -4.999999999999920952, -65.00000000000001421, -7.500000000000007105 ) ) ;
#11745 = CARTESIAN_POINT ( 'NONE',  ( 5.196152422706629359, 3.000000000000002665, -113.9613248654052171 ) ) ;
#11746 = CARTESIAN_POINT ( 'NONE',  ( 111.6249999999998153, -1.767766952966376426, -1.767766952966431937 ) ) ;
#11747 = CARTESIAN_POINT ( 'NONE',  ( 6.000000000000052403, -1.607695154586662678, -94.65331216351297883 ) ) ;
#11748 = FACE_OUTER_BOUND ( 'NONE', #28402, .T. ) ;
#11749 = SURFACE_STYLE_FILL_AREA ( #25525 ) ;
#11750 = VERTEX_POINT ( 'NONE', #1736 ) ;
#11751 = EDGE_CURVE ( 'NONE', #25219, #12504, #9580, .T. ) ;
#11752 = CARTESIAN_POINT ( 'NONE',  ( 0.000000000000000000, 5.499999999999991118, -55.49999999999999289 ) ) ;
#11753 = DIRECTION ( 'NONE',  ( -8.326672684688675286E-17, -2.081668171172168821E-17, 1.000000000000000000 ) ) ;
#11754 = CARTESIAN_POINT ( 'NONE',  ( 6.000000000000052403, 1.607695154586625819, -121.5193375672974412 ) ) ;
#11755 = CARTESIAN_POINT ( 'NONE',  ( -5.196152422706573404, -3.000000000000002665, -152.2113248654052313 ) ) ;
#11756 = AXIS2_PLACEMENT_3D ( 'NONE', #989, #18350, #15913 ) ;
#11757 = ORIENTED_EDGE ( 'NONE', *, *, #29874, .T. ) ;
#11758 = CARTESIAN_POINT ( 'NONE',  ( 106.0624999999998295, 2.500000000000114575, 1.035533905933049725 ) ) ;
#11759 = CARTESIAN_POINT ( 'NONE',  ( 137.2500000000000284, -6.000000000000005329, 0.000000000000000000 ) ) ;
#11760 = CARTESIAN_POINT ( 'NONE',  ( 7.216878364870455975, -6.409875621278545621E-14, -104.9419872981078470 ) ) ;
#11761 = CARTESIAN_POINT ( 'NONE',  ( 6.000000000000000888, 1.607695154586715303, -177.0193375672974696 ) ) ;
#11762 = ADVANCED_FACE ( 'NONE', ( #22332 ), #3873, .F. ) ;
#11763 = ADVANCED_FACE ( 'NONE', ( #19866 ), #15765, .T. ) ;
#11764 = CARTESIAN_POINT ( 'NONE',  ( 160.1101497308104058, 3.535533905932725318, 3.535533905932725318 ) ) ;
#11765 = CARTESIAN_POINT ( 'NONE',  ( 118.5624999999997016, -2.499999999999874767, -1.035533905932568999 ) ) ;
#11766 = CARTESIAN_POINT ( 'NONE',  ( -3.175426480542816510, -5.500000000000057732, -140.3750000000000568 ) ) ;
#11767 =( BOUNDED_CURVE ( )  B_SPLINE_CURVE ( 2, ( #19312, #28631, #5592, #12563, #3141, #10243, #23908, #28942, #2851 ),
 .UNSPECIFIED., .F., .T. ) 
 B_SPLINE_CURVE_WITH_KNOTS ( ( 3, 2, 2, 2, 3 ),
 ( 0.4125000000000008105, 0.4187500000000006217, 0.4250000000000003775, 0.4312500000000001887, 0.4374999999999999445 ),
 .UNSPECIFIED. ) 
 CURVE ( )  GEOMETRIC_REPRESENTATION_ITEM ( )  RATIONAL_B_SPLINE_CURVE ( ( 0.9999999999999898970, 0.9238795325112968415, 1.000000000000000000, 0.9238795325112867385, 1.000000000000000000, 0.9238795325112867385, 1.000000000000000000, 0.9238795325112874046, 0.9999999999999993339 ) ) 
 REPRESENTATION_ITEM ( '' )  );
#11768 = EDGE_LOOP ( 'NONE', ( #24067, #18772, #11128, #25305 ) ) ;
#11769 = CARTESIAN_POINT ( 'NONE',  ( 3.330669073875473566E-16, -6.000000000000005329, -5.329070518200757705E-15 ) ) ;
#11770 = CARTESIAN_POINT ( 'NONE',  ( 3.175426480543072749, 5.499999999999865885, -67.62500000000002842 ) ) ;
#11771 = CARTESIAN_POINT ( 'NONE',  ( 6.000000000000014211, -1.607695154586730180, -164.2306624327026157 ) ) ;
#11772 = LINE ( 'NONE', #7277, #22546 ) ;
#11773 = CARTESIAN_POINT ( 'NONE',  ( 7.216878364870455975, -6.409875621278545621E-14, -80.30801270189225249 ) ) ;
#11774 = CIRCLE ( 'NONE', #24957, 1.000000000000000888 ) ;
#11775 = CARTESIAN_POINT ( 'NONE',  ( 152.5386751345948539, -5.500000000000005329, 0.000000000000000000 ) ) ;
#11776 = CARTESIAN_POINT ( 'NONE',  ( 107.4997167782375982, 1.308140751793723799, -1.308140751793640533 ) ) ;
#11777 = DIRECTION ( 'NONE',  ( -7.147005652999508048E-36, 5.642372883946980038E-36, 1.000000000000000000 ) ) ;
#11778 = DIRECTION ( 'NONE',  ( 1.000000000000000000, -5.551115123125773458E-17, -1.260129944081490338E-35 ) ) ;
#11779 = CARTESIAN_POINT ( 'NONE',  ( 120.4377832217621176, 1.849990392679562001, 0.7662911109080692285 ) ) ;
#11780 = CARTESIAN_POINT ( 'NONE',  ( -4.763139720814407951, -2.750000000000016431, -145.0000000000000284 ) ) ;
#11781 = CARTESIAN_POINT ( 'NONE',  ( 19.10117513459493566, 1.035533905932809473, -2.499999999999964473 ) ) ;
#11782 = CARTESIAN_POINT ( 'NONE',  ( -4.763139720814407951, 2.749999999999946709, -139.2499999999999716 ) ) ;
#11783 = CARTESIAN_POINT ( 'NONE',  ( 5.412658773652739619, 3.124999999999988898, -161.1830127018922667 ) ) ;
#11784 = CARTESIAN_POINT ( 'NONE',  ( 5.196152422706629359, 3.000000000000002665, -116.9613248654052313 ) ) ;
#11785 = DIRECTION ( 'NONE',  ( -7.147005652999508048E-36, 5.642372883946980038E-36, 1.000000000000000000 ) ) ;
#11786 = EDGE_CURVE ( 'NONE', #379, #1732, #14844, .T. ) ;
#11787 = CARTESIAN_POINT ( 'NONE',  ( -4.763139720814407951, -2.750000000000016431, -77.50000000000001421 ) ) ;
#11788 = DIRECTION ( 'NONE',  ( 0.000000000000000000, 0.000000000000000000, -1.000000000000000000 ) ) ;
#11789 = CARTESIAN_POINT ( 'NONE',  ( -4.763139720814407951, -2.750000000000016431, -62.50000000000000000 ) ) ;
#11790 = DIRECTION ( 'NONE',  ( -0.000000000000000000, -0.000000000000000000, -1.000000000000000000 ) ) ;
#11791 = CARTESIAN_POINT ( 'NONE',  ( 145.7023502691896510, 0.000000000000000000, -5.000000000000004441 ) ) ;
#11792 = CARTESIAN_POINT ( 'NONE',  ( 6.000000000000000888, -3.330669073875464691E-16, -7.560779664488942560E-35 ) ) ;
#11793 = FACE_OUTER_BOUND ( 'NONE', #2016, .T. ) ;
#11794 = CARTESIAN_POINT ( 'NONE',  ( 159.0937500000000284, 6.000000000000005329, 2.485281374238585972 ) ) ;
#11795 = CARTESIAN_POINT ( 'NONE',  ( 144.2738248654052313, -3.889087296526011706, 3.889087296526011706 ) ) ;
#11796 = CARTESIAN_POINT ( 'NONE',  ( 6.000000000000052403, -1.607695154586662678, -49.65331216351296462 ) ) ;
#11797 = FACE_OUTER_BOUND ( 'NONE', #11852, .T. ) ;
#11798 = CARTESIAN_POINT ( 'NONE',  ( 116.6872167782373708, 1.849990392679501827, 0.7662911109079489913 ) ) ;
#11799 = ADVANCED_FACE ( 'NONE', ( #20024 ), #17590, .T. ) ;
#11800 = CARTESIAN_POINT ( 'NONE',  ( -6.000000000000007105, -1.607695154586655129, -98.26933756729742697 ) ) ;
#11801 = ORIENTED_EDGE ( 'NONE', *, *, #21426, .F. ) ;
#11802 = VECTOR ( 'NONE', #16800, 1000.000000000000000 ) ;
#11803 = CARTESIAN_POINT ( 'NONE',  ( 147.6562500000000284, -6.000000000000005329, 2.485281374238555774 ) ) ;
#11804 = LINE ( 'NONE', #25111, #10175 ) ;
#11805 = CARTESIAN_POINT ( 'NONE',  ( 114.6252832217623450, 0.000000000000000000, 1.849990392679523588 ) ) ;
#11806 = AXIS2_PLACEMENT_3D ( 'NONE', #3067, #22848, #28863 ) ;
#11807 = CARTESIAN_POINT ( 'NONE',  ( -5.999999999999919176, 1.607695154586804565, -179.4033121635130215 ) ) ;
#11808 = ORIENTED_EDGE ( 'NONE', *, *, #3430, .T. ) ;
#11809 = ORIENTED_EDGE ( 'NONE', *, *, #21231, .F. ) ;
#11810 = CARTESIAN_POINT ( 'NONE',  ( 21.06250000000004619, 2.000000000000151879, 0.8284271247461153509 ) ) ;
#11811 = ORIENTED_EDGE ( 'NONE', *, *, #8908, .T. ) ;
#11812 = CARTESIAN_POINT ( 'NONE',  ( -2.775557561562891351E-14, -5.500000000000115463, -86.25000000000004263 ) ) ;
#11813 = CARTESIAN_POINT ( 'NONE',  ( -3.608439182435115633, 6.249999999999965361, -106.8080127018922667 ) ) ;
#11814 = VERTEX_POINT ( 'NONE', #22643 ) ;
#11815 = CARTESIAN_POINT ( 'NONE',  ( 3.199609099280345870, 10.52573284576699386, -30.07939160056614014 ) ) ;
#11816 = CARTESIAN_POINT ( 'NONE',  ( 158.2351497308104058, 3.535533905932725318, -3.535533905932725318 ) ) ;
#11817 =( BOUNDED_CURVE ( )  B_SPLINE_CURVE ( 2, ( #4951, #18978, #51, #23427, #6669, #2656, #6813, #9440, #21264 ),
 .UNSPECIFIED., .F., .F. ) 
 B_SPLINE_CURVE_WITH_KNOTS ( ( 3, 2, 2, 2, 3 ),
 ( 0.3083333333333333481, 0.3092592592592592338, 0.3111111111111111160, 0.3129629629629629428, 0.3138888888888888840 ),
 .UNSPECIFIED. ) 
 CURVE ( )  GEOMETRIC_REPRESENTATION_ITEM ( )  RATIONAL_B_SPLINE_CURVE ( ( 0.9330127018922194093, 0.9330127018922214077, 1.000000000000000000, 0.8660254037844388186, 1.000000000000000000, 0.8660254037844388186, 1.000000000000000000, 0.9330127018922194093, 0.9330127018922194093 ) ) 
 REPRESENTATION_ITEM ( '' )  );
#11818 = CARTESIAN_POINT ( 'NONE',  ( 5.412658773652712085, -3.125000000000086153, -47.43301270189226670 ) ) ;
#11819 = AXIS2_PLACEMENT_3D ( 'NONE', #9239, #21229, #21382 ) ;
#11820 = CARTESIAN_POINT ( 'NONE',  ( 135.5105870461044617, -9.078052452533968975, 8.000000000000007105 ) ) ;
#11821 = AXIS2_PLACEMENT_3D ( 'NONE', #24327, #836, #10233 ) ;
#11822 = CARTESIAN_POINT ( 'NONE',  ( -3.175426480542816066, 5.499999999999865885, -169.3750000000000568 ) ) ;
#11823 = CARTESIAN_POINT ( 'NONE',  ( 147.8363248654052029, 0.000000000000000000, -5.500000000000005329 ) ) ;
#11824 = CARTESIAN_POINT ( 'NONE',  ( 0.000000000000000000, 5.499999999999991118, -151.5000000000000284 ) ) ;
#11825 = CIRCLE ( 'NONE', #1954, 12.00000000000000178 ) ;
#11826 = CARTESIAN_POINT ( 'NONE',  ( 113.4374999999998863, -2.499999999999994671, 1.035533905932869425 ) ) ;
#11827 = ADVANCED_FACE ( 'NONE', ( #6034 ), #19977, .F. ) ;
#11828 = CARTESIAN_POINT ( 'NONE',  ( 4.763139720814407951, 2.750000000000002665, -102.2500000000000142 ) ) ;
#11829 = PLANE ( 'NONE',  #16403 ) ;
#11830 = CARTESIAN_POINT ( 'NONE',  ( -9.999999999999994671, -9.000000000000007105, 5.000000000000004441 ) ) ;
#11831 = EDGE_CURVE ( 'NONE', #26790, #23931, #7923, .T. ) ;
#11832 = CARTESIAN_POINT ( 'NONE',  ( -6.350852961085760029, -1.281975124255709124E-13, -91.12500000000001421 ) ) ;
#11833 = DIRECTION ( 'NONE',  ( 1.000000000000000000, -0.000000000000000000, -0.000000000000000000 ) ) ;
#11834 =( LENGTH_UNIT ( ) NAMED_UNIT ( * ) SI_UNIT ( .MILLI., .METRE. ) );
#11835 = ORIENTED_EDGE ( 'NONE', *, *, #10508, .T. ) ;
#11836 = CARTESIAN_POINT ( 'NONE',  ( 9.812500000000087041, 1.097466725451679892, 2.649519052838298805 ) ) ;
#11837 = CARTESIAN_POINT ( 'NONE',  ( 113.2499999999998437, 2.775557561562891351E-14, 2.500000000000168754 ) ) ;
#11838 = CARTESIAN_POINT ( 'NONE',  ( 15.78867513459494809, -2.499999999999946709, -2.220446049250313081E-13 ) ) ;
#11839 = CARTESIAN_POINT ( 'NONE',  ( 107.0627832217620892, -0.7662911109076184779, -1.849990392679351725 ) ) ;
#11840 = DIRECTION ( 'NONE',  ( -7.147005652999508048E-36, 5.642372883946980038E-36, 1.000000000000000000 ) ) ;
#11841 = ORIENTED_EDGE ( 'NONE', *, *, #16874, .F. ) ;
#11842 = CARTESIAN_POINT ( 'NONE',  ( 9.750000000000119016, 1.665334536937734811E-13, -1.999999999999890754 ) ) ;
#11843 = DIRECTION ( 'NONE',  ( -7.147005652999508048E-36, 5.642372883946980038E-36, 1.000000000000000000 ) ) ;
#11844 = PRESENTATION_LAYER_ASSIGNMENT (  '', '', ( #5393 ) ) ;
#11845 = ORIENTED_EDGE ( 'NONE', *, *, #17517, .T. ) ;
#11846 = CARTESIAN_POINT ( 'NONE',  ( -5.999999999999963585, 1.780251999655701777E-13, -53.33632486540522422 ) ) ;
#11847 = ORIENTED_EDGE ( 'NONE', *, *, #7532, .F. ) ;
#11848 = CARTESIAN_POINT ( 'NONE',  ( 149.8125000000000568, 4.242640687119298093, -4.242640687119298093 ) ) ;
#11849 = CARTESIAN_POINT ( 'NONE',  ( 6.350852961086080661, -9.614813431917819062E-14, -111.3750000000000568 ) ) ;
#11850 = CARTESIAN_POINT ( 'NONE',  ( 22.43750000000008882, 2.649519052838419153, 1.097466725451499370 ) ) ;
#11851 = CARTESIAN_POINT ( 'NONE',  ( 3.608439182435180470, 6.249999999999982236, -131.0580127018922383 ) ) ;
#11852 = EDGE_LOOP ( 'NONE', ( #25690, #23308, #4833, #17191 ) ) ;
#11853 = CYLINDRICAL_SURFACE ( 'NONE', #14233, 6.000000000000000888 ) ;
#11854 = CARTESIAN_POINT ( 'NONE',  ( 2.775557561562891351E-14, 6.250000000000033751, -169.0669872981078186 ) ) ;
#11855 = CARTESIAN_POINT ( 'NONE',  ( 109.0624999999997868, 2.500000000000055067, 1.035533905932809473 ) ) ;
#11856 = CARTESIAN_POINT ( 'NONE',  ( 131.7038997308104342, 2.071067811865468400, 4.999999999999989342 ) ) ;
#11857 = ORIENTED_EDGE ( 'NONE', *, *, #14457, .F. ) ;
#11858 = CARTESIAN_POINT ( 'NONE',  ( 0.7667967985550546706, -15.49901982636443343, -8.125930293112922698 ) ) ;
#11859 =( BOUNDED_CURVE ( )  B_SPLINE_CURVE ( 2, ( #9604, #18994, #28317, #4968, #2667, #1227, #8929, #1698, #10948 ),
 .UNSPECIFIED., .F., .T. ) 
 B_SPLINE_CURVE_WITH_KNOTS ( ( 3, 2, 2, 2, 3 ),
 ( 0.2472222222222222043, 0.2481481481481481455, 0.2500000000000000000, 0.2518518518518518268, 0.2527777777777777679 ),
 .UNSPECIFIED. ) 
 CURVE ( )  GEOMETRIC_REPRESENTATION_ITEM ( )  RATIONAL_B_SPLINE_CURVE ( ( 0.9330127018922196314, 0.9330127018922185211, 1.000000000000000000, 0.8660254037844388186, 1.000000000000000000, 0.8660254037844388186, 1.000000000000000000, 0.9330127018922194093, 0.9330127018922194093 ) ) 
 REPRESENTATION_ITEM ( '' )  );
#11860 = CARTESIAN_POINT ( 'NONE',  ( 109.5386751345946834, 5.551115123125782702E-14, 2.000000000000001776 ) ) ;
#11861 = CARTESIAN_POINT ( 'NONE',  ( 6.000000000000000888, 1.607695154586715303, -137.0966878364870354 ) ) ;
#11862 = CARTESIAN_POINT ( 'NONE',  ( 3.175426480543072749, -5.500000000000105693, -177.6250000000000284 ) ) ;
#11863 = CARTESIAN_POINT ( 'NONE',  ( 106.3127832217621318, 1.849990392679501827, -0.7662911109075883909 ) ) ;
#11864 = CARTESIAN_POINT ( 'NONE',  ( 5.412658773652712085, -3.125000000000086153, -179.4330127018922667 ) ) ;
#11865 = CARTESIAN_POINT ( 'NONE',  ( -0.8012806810451161832, -9.198719318954823976, -4.013103574300090237 ) ) ;
#11866 = CARTESIAN_POINT ( 'NONE',  ( 19.99999999999998934, 2.678141147339105664E-16, 4.000000000000000000 ) ) ;
#11867 = MECHANICAL_DESIGN_GEOMETRIC_PRESENTATION_REPRESENTATION (  '', ( #28458 ), #12829 ) ;
#11868 = CARTESIAN_POINT ( 'NONE',  ( 160.9860446771581621, -11.61458924544450966, -3.019433540031084551 ) ) ;
#11869 = EDGE_CURVE ( 'NONE', #12687, #8567, #29016, .T. ) ;
#11870 = CARTESIAN_POINT ( 'NONE',  ( -3.175426480542816510, -5.500000000000057732, -111.8750000000000568 ) ) ;
#11871 =( BOUNDED_CURVE ( )  B_SPLINE_CURVE ( 2, ( #3869, #8170, #3721, #27516, #27368, #13601, #15761, #1884, #13150 ),
 .UNSPECIFIED., .F., .T. ) 
 B_SPLINE_CURVE_WITH_KNOTS ( ( 3, 2, 2, 2, 3 ),
 ( 0.1361111111111110994, 0.1370370370370370405, 0.1388888888888888951, 0.1407407407407407496, 0.1416666666666666907 ),
 .UNSPECIFIED. ) 
 CURVE ( )  GEOMETRIC_REPRESENTATION_ITEM ( )  RATIONAL_B_SPLINE_CURVE ( ( 0.9330127018922196314, 0.9330127018922185211, 1.000000000000000000, 0.8660254037844388186, 1.000000000000000000, 0.8660254037844388186, 1.000000000000000000, 0.9330127018922184101, 0.9330127018922194093 ) ) 
 REPRESENTATION_ITEM ( '' )  );
#11872 = CARTESIAN_POINT ( 'NONE',  ( 134.9999999999992895, -6.982120021884475669, -8.500000000000007105 ) ) ;
#11873 = CYLINDRICAL_SURFACE ( 'NONE', #24311, 2.499999999999999112 ) ;
#11874 = ORIENTED_EDGE ( 'NONE', *, *, #26530, .T. ) ;
#11875 = CARTESIAN_POINT ( 'NONE',  ( 21.37500000000019895, 1.110223024625156540E-13, -2.649519052838333888 ) ) ;
#11876 = CARTESIAN_POINT ( 'NONE',  ( 0.1991573574402268343, -15.94692260098227621, 7.215108609433896092 ) ) ;
#11877 = CARTESIAN_POINT ( 'NONE',  ( 6.000000000000052403, -1.607695154586662678, -55.65331216351297172 ) ) ;
#11878 = DIRECTION ( 'NONE',  ( 1.000000000000000000, -5.551115123125773458E-17, -1.260129944081490338E-35 ) ) ;
#11879 = FACE_OUTER_BOUND ( 'NONE', #23164, .T. ) ;
#11880 = VECTOR ( 'NONE', #351, 1000.000000000000000 ) ;
#11881 = ORIENTED_EDGE ( 'NONE', *, *, #28809, .F. ) ;
#11882 = DIRECTION ( 'NONE',  ( -1.000000000000000000, -1.665334536937731113E-16, 1.526556658859586792E-16 ) ) ;
#11883 = CYLINDRICAL_SURFACE ( 'NONE', #26827, 15.00000000000000000 ) ;
#11884 = CARTESIAN_POINT ( 'NONE',  ( -3.464101615137757051, -5.999999999999979572, -95.66367513459481131 ) ) ;
#11885 = CARTESIAN_POINT ( 'NONE',  ( 140.5238248654052029, 3.889087296526011706, -3.889087296526011706 ) ) ;
#11886 = ORIENTED_EDGE ( 'NONE', *, *, #9891, .T. ) ;
#11887 = VERTEX_POINT ( 'NONE', #6433 ) ;
#11888 = CARTESIAN_POINT ( 'NONE',  ( 151.6800748654052029, -2.278174593052058938, 5.499999999999964473 ) ) ;
#11889 = CARTESIAN_POINT ( 'NONE',  ( 134.1562500000000568, -6.000000000000005329, 2.485281374238555774 ) ) ;
#11890 = CIRCLE ( 'NONE', #24088, 6.000000000000001776 ) ;
#11891 = CARTESIAN_POINT ( 'NONE',  ( -3.608439182435052128, -6.250000000000110134, -136.9419872981078186 ) ) ;
#11892 = CARTESIAN_POINT ( 'NONE',  ( 10.03867513459497118, 1.110223024625156540E-13, -2.500000000000113243 ) ) ;
#11893 = CARTESIAN_POINT ( 'NONE',  ( 11.31250000000006395, 2.649519052838419153, -1.097466725451559322 ) ) ;
#11894 = EDGE_CURVE ( 'NONE', #27647, #11657, #157, .T. ) ;
#11895 = CARTESIAN_POINT ( 'NONE',  ( 20.18750000000014566, 0.8284271247463557142, 1.999999999999911626 ) ) ;
#11896 = CARTESIAN_POINT ( 'NONE',  ( -0.01457429254692333212, -14.38985900264256834, 8.358944243794823592 ) ) ;
#11897 = CARTESIAN_POINT ( 'NONE',  ( -5.999999999999956479, -1.607695154586745057, -137.8466878364870638 ) ) ;
#11898 = DIRECTION ( 'NONE',  ( -1.000000000000000000, -1.665334536937731113E-16, 1.526556658859586792E-16 ) ) ;
#11899 = CARTESIAN_POINT ( 'NONE',  ( 146.4226497308104342, 5.000000000000004441, 0.000000000000000000 ) ) ;
#11900 = CARTESIAN_POINT ( 'NONE',  ( 119.9999999999997868, 1.387778780781445676E-13, 1.110223024625156540E-13 ) ) ;
#11901 = TOROIDAL_SURFACE ( 'NONE', #26544, 16.50000000000000355, 1.000000000000000000 ) ;
#11902 = CARTESIAN_POINT ( 'NONE',  ( 12.78867513459486283, -2.499999999999891198, -2.220446049250313081E-13 ) ) ;
#11903 = PRESENTATION_STYLE_ASSIGNMENT (( #23980 ) ) ;
#11904 = CARTESIAN_POINT ( 'NONE',  ( 24.78514766611641562, -1.168806754308282292, -1.887491515121927588 ) ) ;
#11905 = CARTESIAN_POINT ( 'NONE',  ( 109.0238248654049045, -0.8284271247461453269, 2.000000000000271783 ) ) ;
#11906 = CARTESIAN_POINT ( 'NONE',  ( 110.9374999999997158, 2.500000000000054623, -1.035533905932388699 ) ) ;
#11907 = EDGE_CURVE ( 'NONE', #6421, #17999, #19720, .T. ) ;
#11908 =( LENGTH_UNIT ( ) NAMED_UNIT ( * ) SI_UNIT ( .MILLI., .METRE. ) );
#11909 = CARTESIAN_POINT ( 'NONE',  ( -3.464101615137725076, 5.999999999999979572, -148.6636751345947403 ) ) ;
#11910 = ORIENTED_EDGE ( 'NONE', *, *, #7985, .F. ) ;
#11911 =( BOUNDED_CURVE ( )  B_SPLINE_CURVE ( 2, ( #27843, #4512, #18823, #16239, #4810, #23572, #13936 ),
 .UNSPECIFIED., .F., .F. ) 
 B_SPLINE_CURVE_WITH_KNOTS ( ( 3, 2, 2, 3 ),
 ( 0.04179654864244304602, 0.04411764705882353227, 0.05147058823529411520, 0.05882352941176470507 ),
 .UNSPECIFIED. ) 
 CURVE ( )  GEOMETRIC_REPRESENTATION_ITEM ( )  RATIONAL_B_SPLINE_CURVE ( ( 0.9671125746063340411, 0.9759710988702614554, 1.000000000000000000, 0.9238795325112867385, 1.000000000000000000, 0.9238795325112867385, 1.000000000000000000 ) ) 
 REPRESENTATION_ITEM ( '' )  );
#11912 = AXIS2_PLACEMENT_3D ( 'NONE', #20584, #29932, #8912 ) ;
#11913 = CARTESIAN_POINT ( 'NONE',  ( -4.763139720814407951, 2.749999999999946709, -52.25000000000002132 ) ) ;
#11914 = CARTESIAN_POINT ( 'NONE',  ( -5.196152422706601826, 2.999999999999975131, -87.96132486540520290 ) ) ;
#11915 = DIRECTION ( 'NONE',  ( -7.147005652999508048E-36, 5.642372883946980038E-36, 1.000000000000000000 ) ) ;
#11916 = CARTESIAN_POINT ( 'NONE',  ( 139.5000000000000284, -54.99999999999990763, 8.000000000000007105 ) ) ;
#11917 = ORIENTED_EDGE ( 'NONE', *, *, #22581, .T. ) ;
#11918 = CARTESIAN_POINT ( 'NONE',  ( 118.9997167782376266, -1.308140751793529510, 1.308140751793973600 ) ) ;
#11919 = CARTESIAN_POINT ( 'NONE',  ( 141.2812500000000284, 2.485281374238585972, 6.000000000000005329 ) ) ;
#11920 = CARTESIAN_POINT ( 'NONE',  ( -5.412658773652739619, 3.124999999999975131, -99.81698729810784698 ) ) ;
#11921 = CARTESIAN_POINT ( 'NONE',  ( 161.0000000000000284, 0.000000000000000000, 0.000000000000000000 ) ) ;
#11922 = CARTESIAN_POINT ( 'NONE',  ( 135.0937500000000284, 6.000000000000005329, 2.485281374238585972 ) ) ;
#11923 = CARTESIAN_POINT ( 'NONE',  ( 117.8749999999998010, 1.767766952966320915, -1.767766952966209892 ) ) ;
#11924 = VERTEX_POINT ( 'NONE', #17690 ) ;
#11925 = CIRCLE ( 'NONE', #18768, 4.000000000000006217 ) ;
#11926 = CARTESIAN_POINT ( 'NONE',  ( 0.000000000000000000, 5.499999999999991118, -141.0000000000000000 ) ) ;
#11927 = ORIENTED_EDGE ( 'NONE', *, *, #6301, .F. ) ;
#11928 = CARTESIAN_POINT ( 'NONE',  ( 115.6488248654049187, 2.000000000000151879, -0.8284271247459350507 ) ) ;
#11929 = EDGE_CURVE ( 'NONE', #25500, #9277, #7244, .T. ) ;
#11930 = CARTESIAN_POINT ( 'NONE',  ( 3.175426480543072749, 5.499999999999865885, -64.62500000000001421 ) ) ;
#11931 = AXIS2_PLACEMENT_3D ( 'NONE', #1719, #24764, #29357 ) ;
#11932 = DIRECTION ( 'NONE',  ( -7.147005652999508048E-36, 5.642372883946980038E-36, 1.000000000000000000 ) ) ;
#11933 = CARTESIAN_POINT ( 'NONE',  ( 108.7886751345946834, -1.999999999999946265, 1.110223024625156540E-13 ) ) ;
#11934 = CARTESIAN_POINT ( 'NONE',  ( 5.412658773652739619, 3.124999999999988898, -80.18301270189220986 ) ) ;
#11935 = CARTESIAN_POINT ( 'NONE',  ( 10.53867513459491612, 5.551115123125782702E-14, 2.499999999999724665 ) ) ;
#11936 = CARTESIAN_POINT ( 'NONE',  ( 152.1636751345948255, 0.000000000000000000, 5.500000000000005329 ) ) ;
#11937 = CARTESIAN_POINT ( 'NONE',  ( 104.8747167782376550, -2.775557561562891351E-14, 1.849990392679523588 ) ) ;
#11938 = CARTESIAN_POINT ( 'NONE',  ( 140.5000000000000284, -11.02592621076652790, 4.736429266082377687 ) ) ;
#11939 = CARTESIAN_POINT ( 'NONE',  ( -5.999999999999919176, 1.607695154586804565, -60.90331216351300725 ) ) ;
#11940 = CARTESIAN_POINT ( 'NONE',  ( 119.1252832217622597, -5.551115123125782702E-14, -1.849990392679412565 ) ) ;
#11941 = EDGE_CURVE ( 'NONE', #8039, #25268, #3820, .T. ) ;
#11942 = EDGE_CURVE ( 'NONE', #17742, #1935, #18909, .T. ) ;
#11943 = CARTESIAN_POINT ( 'NONE',  ( 3.175426480543072749, -5.500000000000105693, -147.6250000000000284 ) ) ;
#11944 = CARTESIAN_POINT ( 'NONE',  ( 6.000000000000000888, -1.607695154586752384, -105.1533121635130215 ) ) ;
#11945 = EDGE_CURVE ( 'NONE', #29849, #14641, #2537, .T. ) ;
#11946 = CARTESIAN_POINT ( 'NONE',  ( -5.412658773652684552, -3.125000000000099920, -160.4330127018922667 ) ) ;
#11947 = CARTESIAN_POINT ( 'NONE',  ( -3.464101615137725076, 5.999999999999979572, -89.58632486540521711 ) ) ;
#11948 = AXIS2_PLACEMENT_3D ( 'NONE', #17867, #22606, #1541 ) ;
#11949 = CARTESIAN_POINT ( 'NONE',  ( -4.763139720814407951, 2.749999999999946709, -77.74999999999998579 ) ) ;
#11950 = CARTESIAN_POINT ( 'NONE',  ( 3.175426480543072749, -5.500000000000105693, -66.62500000000002842 ) ) ;
#11951 = CARTESIAN_POINT ( 'NONE',  ( 143.7336002691896795, -4.999999999999989342, 2.071067811865468400 ) ) ;
#11952 = CARTESIAN_POINT ( 'NONE',  ( 0.8619745489090032686, -15.74670610583283548, 7.642883928913009939 ) ) ;
#11953 = CARTESIAN_POINT ( 'NONE',  ( 155.1562500000000284, -6.000000000000005329, 2.485281374238556218 ) ) ;
#11954 = CARTESIAN_POINT ( 'NONE',  ( 160.0000000000000284, -59.99999999999980105, 3.000000000000002665 ) ) ;
#11955 = CARTESIAN_POINT ( 'NONE',  ( 16.56250000000011369, -1.999999999999911626, -0.8284271247462354770 ) ) ;
#11956 = DIRECTION ( 'NONE',  ( -1.000000000000000000, -1.665334536937736783E-16, -2.220446049250315546E-16 ) ) ;
#11957 = CARTESIAN_POINT ( 'NONE',  ( 117.5622167782373992, 1.849990392679562001, -0.7662911109076485650 ) ) ;
#11958 = DIRECTION ( 'NONE',  ( -7.147005652999508048E-36, 5.642372883946980038E-36, 1.000000000000000000 ) ) ;
#11959 =( BOUNDED_CURVE ( )  B_SPLINE_CURVE ( 2, ( #12864, #22051, #29086, #15151, #22519, #24643, #1291, #13182, #13019 ),
 .UNSPECIFIED., .F., .F. ) 
 B_SPLINE_CURVE_WITH_KNOTS ( ( 3, 2, 2, 2, 3 ),
 ( 0.1470588235294117696, 0.1544117647058823595, 0.1617647058823529493, 0.1691176470588235392, 0.1764705882352941291 ),
 .UNSPECIFIED. ) 
 CURVE ( )  GEOMETRIC_REPRESENTATION_ITEM ( )  RATIONAL_B_SPLINE_CURVE ( ( 1.000000000000000000, 0.9238795325112867385, 1.000000000000000000, 0.9238795325112867385, 1.000000000000000000, 0.9238795325112867385, 1.000000000000000000, 0.9238795325112867385, 1.000000000000000000 ) ) 
 REPRESENTATION_ITEM ( '' )  );
#11960 = ORIENTED_EDGE ( 'NONE', *, *, #11999, .T. ) ;
#11961 = CARTESIAN_POINT ( 'NONE',  ( 148.5000000000000284, 6.000000000000005329, 0.000000000000000000 ) ) ;
#11962 = CARTESIAN_POINT ( 'NONE',  ( 115.5002832217623308, 1.308140751793640533, 1.308140751793640533 ) ) ;
#11963 = CARTESIAN_POINT ( 'NONE',  ( 4.763139720814407951, 2.750000000000002665, -153.2500000000000000 ) ) ;
#11964 = STYLED_ITEM ( 'NONE', ( #24330 ), #24617 ) ;
#11965 = CARTESIAN_POINT ( 'NONE',  ( 20.12500000000011369, 1.414213562373201061, 1.414213562373034527 ) ) ;
#11966 = CARTESIAN_POINT ( 'NONE',  ( 7.216878364870455975, -6.409875621278545621E-14, -154.4419872981078186 ) ) ;
#11967 = EDGE_LOOP ( 'NONE', ( #9031, #3769, #8472, #20570 ) ) ;
#11968 = EDGE_CURVE ( 'NONE', #14907, #28127, #4882, .T. ) ;
#11969 = CARTESIAN_POINT ( 'NONE',  ( 4.763139720814407951, -2.749999999999988454, -93.50000000000002842 ) ) ;
#11970 = CARTESIAN_POINT ( 'NONE',  ( 15.81250000000006395, -2.649519052838178457, 1.097466725451439196 ) ) ;
#11971 = ORIENTED_EDGE ( 'NONE', *, *, #19553, .F. ) ;
#11972 = CARTESIAN_POINT ( 'NONE',  ( 155.7038997308104058, 2.071067811865468400, 4.999999999999989342 ) ) ;
#11973 = CARTESIAN_POINT ( 'NONE',  ( 4.763139720814407951, -2.749999999999988454, -168.4999999999999716 ) ) ;
#11974 = DIRECTION ( 'NONE',  ( -7.147005652999508048E-36, 5.642372883946980038E-36, 1.000000000000000000 ) ) ;
#11975 = EDGE_CURVE ( 'NONE', #2318, #25700, #16868, .T. ) ;
#11976 = ADVANCED_FACE ( 'NONE', ( #30395 ), #25472, .T. ) ;
#11977 = CARTESIAN_POINT ( 'NONE',  ( 3.175426480543072749, 5.499999999999865885, -171.1250000000000000 ) ) ;
#11978 = CARTESIAN_POINT ( 'NONE',  ( 143.8988248654052313, 3.889087296526011706, 3.889087296526011706 ) ) ;
#11979 = CARTESIAN_POINT ( 'NONE',  ( 3.175426480543072749, -5.500000000000105693, -153.6250000000000568 ) ) ;
#11980 = CARTESIAN_POINT ( 'NONE',  ( -3.175426480542816066, 5.499999999999865885, -101.8750000000000142 ) ) ;
#11981 = LINE ( 'NONE', #7754, #9372 ) ;
#11983 = CARTESIAN_POINT ( 'NONE',  ( 4.763139720814407951, 2.750000000000002665, -93.25000000000000000 ) ) ;
#11982 = CARTESIAN_POINT ( 'NONE',  ( 4.763139720814407951, -2.749999999999988454, -156.5000000000000284 ) ) ;
#11984 = CARTESIAN_POINT ( 'NONE',  ( 156.0148502691896510, -3.535533905932725318, -3.535533905932725318 ) ) ;
#11985 = CARTESIAN_POINT ( 'NONE',  ( 107.1636751345947545, 1.414213562373062283, -1.414213562372812483 ) ) ;
#11986 = ORIENTED_EDGE ( 'NONE', *, *, #14124, .F. ) ;
#11987 = CARTESIAN_POINT ( 'NONE',  ( 24.62500000000012079, -1.414213562372923505, -1.414213562373145550 ) ) ;
#11988 = CARTESIAN_POINT ( 'NONE',  ( 112.8124999999998579, 1.035533905932779275, -2.499999999999904521 ) ) ;
#11989 = DIRECTION ( 'NONE',  ( 0.000000000000000000, 0.000000000000000000, 1.000000000000000000 ) ) ;
#11990 = CARTESIAN_POINT ( 'NONE',  ( 108.3127832217620181, 1.849990392679562001, -0.7662911109076485650 ) ) ;
#11991 = CARTESIAN_POINT ( 'NONE',  ( 161.0701415566729509, 1.250657853440976686, 5.437060510562927718 ) ) ;
#11992 = VERTEX_POINT ( 'NONE', #30241 ) ;
#11993 = DIRECTION ( 'NONE',  ( 0.000000000000000000, 0.2307692307692307543, 0.9730085108210398959 ) ) ;
#11994 = CARTESIAN_POINT ( 'NONE',  ( 0.000000000000000000, 0.000000000000000000, 0.000000000000000000 ) ) ;
#11995 = ORIENTED_EDGE ( 'NONE', *, *, #19625, .F. ) ;
#11996 = CARTESIAN_POINT ( 'NONE',  ( -5.999999999999956479, -1.607695154586745057, -141.7693375672974128 ) ) ;
#11997 = CARTESIAN_POINT ( 'NONE',  ( 148.0312500000000284, -2.485281374238555774, -6.000000000000005329 ) ) ;
#11998 = VERTEX_POINT ( 'NONE', #12009 ) ;
#11999 = EDGE_CURVE ( 'NONE', #30347, #23965, #26246, .T. ) ;
#12000 = CARTESIAN_POINT ( 'NONE',  ( -4.763139720814407951, 2.749999999999946709, -116.7500000000000142 ) ) ;
#12001 = CARTESIAN_POINT ( 'NONE',  ( 20.00000000000018474, -1.873492889144845464, -1.873492889144956486 ) ) ;
#12002 = CARTESIAN_POINT ( 'NONE',  ( 5.412658773652739619, 3.124999999999988898, -120.6830127018922383 ) ) ;
#12003 = ORIENTED_EDGE ( 'NONE', *, *, #20230, .T. ) ;
#12004 = DIRECTION ( 'NONE',  ( -7.147005652999508048E-36, 5.642372883946980038E-36, 1.000000000000000000 ) ) ;
#12005 = CARTESIAN_POINT ( 'NONE',  ( 2.775557561562891351E-14, 6.250000000000033751, -166.0669872981078186 ) ) ;
#12006 = CARTESIAN_POINT ( 'NONE',  ( 109.3124999999999147, -1.035533905932598975, 2.500000000000265121 ) ) ;
#12007 = ORIENTED_EDGE ( 'NONE', *, *, #26577, .F. ) ;
#12008 = EDGE_CURVE ( 'NONE', #6343, #6339, #6237, .T. ) ;
#12009 = CARTESIAN_POINT ( 'NONE',  ( -5.999999999999962697, 3.323446944526963891E-14, -152.9136751345948255 ) ) ;
#12010 = CARTESIAN_POINT ( 'NONE',  ( -6.350852961085760029, -1.281975124255709124E-13, -176.6250000000000568 ) ) ;
#12011 = CARTESIAN_POINT ( 'NONE',  ( 108.3752832217622739, 1.849990392679523588, 0.000000000000000000 ) ) ;
#12012 = CARTESIAN_POINT ( 'NONE',  ( -5.412658773652684552, -3.125000000000099920, -173.9330127018922099 ) ) ;
#12013 = CARTESIAN_POINT ( 'NONE',  ( 135.0000000000000284, -9.165151389911669000, 8.500000000000007105 ) ) ;
#12014 =( NAMED_UNIT ( * ) SI_UNIT ( $, .STERADIAN. ) SOLID_ANGLE_UNIT ( ) );
#12015 = LINE ( 'NONE', #18762, #14352 ) ;
#12016 = CARTESIAN_POINT ( 'NONE',  ( -2.775557561562891351E-14, -5.500000000000115463, -111.7500000000000142 ) ) ;
#12017 = DIRECTION ( 'NONE',  ( 0.000000000000000000, 0.000000000000000000, -1.000000000000000000 ) ) ;
#12018 = CARTESIAN_POINT ( 'NONE',  ( 6.000000000000000888, -1.859271017917181981E-14, -89.16367513459485394 ) ) ;
#12019 = VERTEX_POINT ( 'NONE', #9206 ) ;
#12020 = CARTESIAN_POINT ( 'NONE',  ( 18.37500000000002842, 1.665334536937734811E-13, -2.649519052838444910 ) ) ;
#12021 = DIRECTION ( 'NONE',  ( 1.000000000000000000, 0.000000000000000000, 0.000000000000000000 ) ) ;
#12022 = DIRECTION ( 'NONE',  ( -7.147005652999508048E-36, 5.642372883946980038E-36, 1.000000000000000000 ) ) ;
#12023 = CARTESIAN_POINT ( 'NONE',  ( 0.000000000000000000, 5.999999999999977796, -131.7113248654052029 ) ) ;
#12024 = EDGE_LOOP ( 'NONE', ( #20486, #16916, #21513, #20723 ) ) ;
#12025 = CARTESIAN_POINT ( 'NONE',  ( 2.081668171172167281E-16, 3.582034040661430693E-16, -2.499999999999999112 ) ) ;
#12026 = CARTESIAN_POINT ( 'NONE',  ( -4.763139720814407951, -2.750000000000016431, -179.5000000000000000 ) ) ;
#12027 = CARTESIAN_POINT ( 'NONE',  ( 22.08632486540518158, -1.767766952966320915, 1.767766952966320915 ) ) ;
#12028 = CARTESIAN_POINT ( 'NONE',  ( -5.999999999999963585, 1.780251999655701777E-13, -77.91367513459482552 ) ) ;
#12029 = CARTESIAN_POINT ( 'NONE',  ( 6.000000000000000888, 1.743066579297358182E-13, -57.66367513459481842 ) ) ;
#12030 = ORIENTED_EDGE ( 'NONE', *, *, #10090, .T. ) ;
#12031 = ORIENTED_EDGE ( 'NONE', *, *, #10185, .T. ) ;
#12032 = CARTESIAN_POINT ( 'NONE',  ( 106.1011751345946266, 0.8284271247462955401, -1.999999999999731104 ) ) ;
#12033 = CARTESIAN_POINT ( 'NONE',  ( 137.2500000000000284, -6.000000000000005329, 0.000000000000000000 ) ) ;
#12034 = EDGE_CURVE ( 'NONE', #28360, #22536, #18599, .T. ) ;
#12035 =( BOUNDED_SURFACE ( )  B_SPLINE_SURFACE ( 2, 3, ( 
 ( #30326, #18528, #9448, #20824 ),
 ( #14245, #9287, #9136, #23729 ),
 ( #27853, #23437, #6822, #21270 ) ),
 .UNSPECIFIED., .F., .F., .T. ) 
 B_SPLINE_SURFACE_WITH_KNOTS ( ( 3, 3 ),
 ( 4, 4 ),
 ( 0.000000000000000000, 1.000000000000000000 ),
 ( 0.000000000000000000, 1.000000000000000000 ),
 .UNSPECIFIED. ) 
 GEOMETRIC_REPRESENTATION_ITEM ( )  RATIONAL_B_SPLINE_SURFACE ( (
 ( 1.000000000000000000, 0.3333333333333334259, 0.3333333333333334259, 1.000000000000000000),
 ( 1.000000000000000000, 0.3333333333333334259, 0.3333333333333334259, 1.000000000000000000),
 ( 1.000000000000000000, 0.3333333333333334259, 0.3333333333333334259, 1.000000000000000000) ) ) 
 REPRESENTATION_ITEM ( '' )  SURFACE ( )  );
#12036 = EDGE_CURVE ( 'NONE', #4573, #20271, #28215, .T. ) ;
#12037 = VERTEX_POINT ( 'NONE', #24101 ) ;
#12038 = CARTESIAN_POINT ( 'NONE',  ( 5.412658773652712085, -3.125000000000086153, -142.5669872981077901 ) ) ;
#12039 = SURFACE_STYLE_FILL_AREA ( #21378 ) ;
#12040 = CARTESIAN_POINT ( 'NONE',  ( 11.18750000000003908, 1.097466725451679892, -2.649519052838298805 ) ) ;
#12041 = CARTESIAN_POINT ( 'NONE',  ( -3.464101615137725076, 5.999999999999979572, -129.1636751345948255 ) ) ;
#12042 = MECHANICAL_DESIGN_GEOMETRIC_PRESENTATION_REPRESENTATION (  '', ( #6600 ), #5131 ) ;
#12043 = CARTESIAN_POINT ( 'NONE',  ( 17.87500000000008527, 1.414213562373312083, -1.414213562373145550 ) ) ;
#12044 = CARTESIAN_POINT ( 'NONE',  ( -4.999999999999886313, -14.50000000000001243, 7.500000000000007105 ) ) ;
#12045 = CARTESIAN_POINT ( 'NONE',  ( 136.2038997308104058, 2.071067811865468400, 4.999999999999989342 ) ) ;
#12046 = CARTESIAN_POINT ( 'NONE',  ( -5.999999999999963585, 1.780251999655701777E-13, -56.91367513459483973 ) ) ;
#12047 = CARTESIAN_POINT ( 'NONE',  ( 0.000000000000000000, -5.999999999999991118, -99.46132486540525974 ) ) ;
#12048 = CARTESIAN_POINT ( 'NONE',  ( 11.00000000000001599, -6.106226635438360972E-16, -43.99152654425658682 ) ) ;
#12049 = CARTESIAN_POINT ( 'NONE',  ( -3.464101615137725076, 5.999999999999979572, -60.16367513459481842 ) ) ;
#12050 = CARTESIAN_POINT ( 'NONE',  ( 106.5624999999998295, -2.499999999999874767, -1.035533905932629173 ) ) ;
#12051 = CARTESIAN_POINT ( 'NONE',  ( 15.89882486540525974, 1.035533905932869425, 2.499999999999844569 ) ) ;
#12052 = CARTESIAN_POINT ( 'NONE',  ( -5.999999999999919176, 1.607695154586804565, -112.4806624327025872 ) ) ;
#12053 = ORIENTED_EDGE ( 'NONE', *, *, #21571, .F. ) ;
#12054 = CARTESIAN_POINT ( 'NONE',  ( -6.000000000000007105, -1.607695154586655129, -107.2693375672974838 ) ) ;
#12055 = DIRECTION ( 'NONE',  ( 0.000000000000000000, 1.000000000000000000, 0.000000000000000000 ) ) ;
#12056 =( LENGTH_UNIT ( ) NAMED_UNIT ( * ) SI_UNIT ( .MILLI., .METRE. ) );
#12057 = ORIENTED_EDGE ( 'NONE', *, *, #29025, .F. ) ;
#12058 = CARTESIAN_POINT ( 'NONE',  ( 116.9372167782374845, -0.7662911109078588412, 1.849990392679652151 ) ) ;
#12059 = DIRECTION ( 'NONE',  ( 1.000000000000000000, 0.000000000000000000, 0.000000000000000000 ) ) ;
#12060 = CARTESIAN_POINT ( 'NONE',  ( 12.18750000000008349, 0.8284271247463557142, 1.999999999999851674 ) ) ;
#12061 = CARTESIAN_POINT ( 'NONE',  ( 5.412658773652712085, -3.125000000000086153, -105.0669872981078186 ) ) ;
#12062 = CARTESIAN_POINT ( 'NONE',  ( 5.196152422706629359, 3.000000000000002665, -176.9613248654052313 ) ) ;
#12063 = CARTESIAN_POINT ( 'NONE',  ( 132.0000000000000284, 6.000000000000005329, 0.000000000000000000 ) ) ;
#12064 = CARTESIAN_POINT ( 'NONE',  ( 116.8124999999998010, 1.035533905932719101, -2.499999999999784173 ) ) ;
#12065 = CIRCLE ( 'NONE', #24284, 2.000000000000012879 ) ;
#12066 = CARTESIAN_POINT ( 'NONE',  ( -3.175426480542816510, 5.499999999999865885, -133.3750000000000284 ) ) ;
#12067 = EDGE_CURVE ( 'NONE', #3090, #25526, #16483, .T. ) ;
#12068 = VERTEX_POINT ( 'NONE', #19208 ) ;
#12069 = CIRCLE ( 'NONE', #14516, 29.00000000000000000 ) ;
#12070 = ORIENTED_EDGE ( 'NONE', *, *, #7375, .F. ) ;
#12071 = CARTESIAN_POINT ( 'NONE',  ( 115.7113248654050466, 2.000000000000112799, 0.000000000000000000 ) ) ;
#12072 = CIRCLE ( 'NONE', #28688, 16.50000000000000355 ) ;
#12073 = CARTESIAN_POINT ( 'NONE',  ( -3.175426480542816510, 5.499999999999865885, -56.87500000000004974 ) ) ;
#12074 = CARTESIAN_POINT ( 'NONE',  ( 22.03867513459498184, 1.110223024625156540E-13, -2.500000000000057732 ) ) ;
#12075 = CARTESIAN_POINT ( 'NONE',  ( 159.9752036821340653, -12.51993663517088429, -3.254295310666532437 ) ) ;
#12076 = CARTESIAN_POINT ( 'NONE',  ( -5.412658773652739619, 3.124999999999975131, -87.18301270189220986 ) ) ;
#12077 = DIRECTION ( 'NONE',  ( 0.000000000000000000, 0.000000000000000000, -1.000000000000000000 ) ) ;
#12078 =( BOUNDED_CURVE ( )  B_SPLINE_CURVE ( 2, ( #20934, #7247, #13904, #4327, #14351, #27809, #2186, #28267, #16356 ),
 .UNSPECIFIED., .F., .F. ) 
 B_SPLINE_CURVE_WITH_KNOTS ( ( 3, 2, 2, 2, 3 ),
 ( 0.8249999999999999556, 0.8259259259259259522, 0.8277777777777777235, 0.8296296296296296058, 0.8305555555555556024 ),
 .UNSPECIFIED. ) 
 CURVE ( )  GEOMETRIC_REPRESENTATION_ITEM ( )  RATIONAL_B_SPLINE_CURVE ( ( 0.9330127018922194093, 0.9330127018922154125, 1.000000000000000000, 0.8660254037844388186, 1.000000000000000000, 0.8660254037844388186, 1.000000000000000000, 0.9330127018922154125, 0.9330127018922194093 ) ) 
 REPRESENTATION_ITEM ( '' )  );
#12079 = CARTESIAN_POINT ( 'NONE',  ( 106.1247167782374987, -1.849990392679412565, 2.220446049250313081E-13 ) ) ;
#12080 = CARTESIAN_POINT ( 'NONE',  ( 140.6818792730027496, -11.36375854600486690, -4.222310544175439162 ) ) ;
#12081 = CARTESIAN_POINT ( 'NONE',  ( 116.5002832217622171, 1.308140751793696044, 1.308140751793640533 ) ) ;
#12082 = CARTESIAN_POINT ( 'NONE',  ( -2.775557561562891351E-14, -5.500000000000115463, -141.7500000000000568 ) ) ;
#12083 = CARTESIAN_POINT ( 'NONE',  ( 140.0000000000000000, -9.600000000000004974, 7.199999999999999289 ) ) ;
#12084 = CARTESIAN_POINT ( 'NONE',  ( 5.412658773652712085, -3.125000000000086153, -150.9330127018922383 ) ) ;
#12085 = CARTESIAN_POINT ( 'NONE',  ( -5.196152422706601826, 2.999999999999975131, -116.4613248654052313 ) ) ;
#12086 = CARTESIAN_POINT ( 'NONE',  ( 0.000000000000000000, -5.999999999999991118, -73.03867513459482552 ) ) ;
#12087 = CARTESIAN_POINT ( 'NONE',  ( -4.763139720814407951, 2.749999999999946709, -68.75000000000002842 ) ) ;
#12088 = CARTESIAN_POINT ( 'NONE',  ( -5.999999999999919176, 1.607695154586804565, -85.48066243270261566 ) ) ;
#12089 = SURFACE_SIDE_STYLE ('',( #14103 ) ) ;
#12090 = CARTESIAN_POINT ( 'NONE',  ( 0.000000000000000000, 5.499999999999991118, -61.50000000000000000 ) ) ;
#12091 = CARTESIAN_POINT ( 'NONE',  ( 139.7187733625200394, -9.255022275057855907, 7.951101893190698711 ) ) ;
#12092 = CARTESIAN_POINT ( 'NONE',  ( 160.8750000000000568, 0.000000000000000000, 6.000000000000005329 ) ) ;
#12093 = AXIS2_PLACEMENT_3D ( 'NONE', #26789, #20367, #22216 ) ;
#12094 = EDGE_CURVE ( 'NONE', #24705, #26328, #21216, .T. ) ;
#12095 = SURFACE_STYLE_USAGE ( .BOTH. , #2529 ) ;
#12096 = CARTESIAN_POINT ( 'NONE',  ( 1.000000000000000888, 0.000000000000000000, 0.000000000000000000 ) ) ;
#12097 = CARTESIAN_POINT ( 'NONE',  ( 115.8122167782375982, 0.7662911109078588412, 1.849990392679712103 ) ) ;
#12098 = DIRECTION ( 'NONE',  ( 0.000000000000000000, 0.000000000000000000, -1.000000000000000000 ) ) ;
#12099 = ORIENTED_EDGE ( 'NONE', *, *, #21518, .T. ) ;
#12100 = CARTESIAN_POINT ( 'NONE',  ( 148.9687500000000284, -2.485281374238585972, 6.000000000000005329 ) ) ;
#12101 = CARTESIAN_POINT ( 'NONE',  ( -3.175426480542816510, 5.499999999999865885, -154.3749999999999716 ) ) ;
#12102 = CARTESIAN_POINT ( 'NONE',  ( 0.000000000000000000, 0.000000000000000000, 8.500000000000007105 ) ) ;
#12103 = CARTESIAN_POINT ( 'NONE',  ( -3.464101615137757051, -5.999999999999979572, -158.6636751345948255 ) ) ;
#12104 = EDGE_CURVE ( 'NONE', #3609, #3090, #28536, .T. ) ;
#12105 = CARTESIAN_POINT ( 'NONE',  ( -4.763139720814407951, 2.749999999999946709, -181.2500000000000284 ) ) ;
#12106 = CARTESIAN_POINT ( 'NONE',  ( 21.12500000000011724, 1.414213562373201061, 1.414213562373034527 ) ) ;
#12107 = ORIENTED_EDGE ( 'NONE', *, *, #21874, .F. ) ;
#12108 = CARTESIAN_POINT ( 'NONE',  ( 5.412658773652739619, 3.124999999999988898, -154.3169872981078470 ) ) ;
#12109 = STYLED_ITEM ( 'NONE', ( #15676 ), #7443 ) ;
#12110 = VERTEX_POINT ( 'NONE', #14611 ) ;
#12111 = CARTESIAN_POINT ( 'NONE',  ( 4.763139720814407951, 2.750000000000002665, -87.25000000000005684 ) ) ;
#12112 = ORIENTED_EDGE ( 'NONE', *, *, #17767, .T. ) ;
#12113 = FILL_AREA_STYLE_COLOUR ( '', #22619 ) ;
#12114 = CARTESIAN_POINT ( 'NONE',  ( 153.4538997308104058, -2.071067811865468400, -4.999999999999989342 ) ) ;
#12115 = AXIS2_PLACEMENT_3D ( 'NONE', #21577, #12380, #14962 ) ;
#12116 = CARTESIAN_POINT ( 'NONE',  ( 107.7886751345947403, -1.999999999999835243, 1.110223024625156540E-13 ) ) ;
#12117 = CARTESIAN_POINT ( 'NONE',  ( 1.580833713216741820, -10.88751498504594473, -19.20858708930976277 ) ) ;
#12118 = DIRECTION ( 'NONE',  ( 1.000000000000000000, -5.551115123125773458E-17, -1.260129944081490338E-35 ) ) ;
#12119 = SURFACE_STYLE_USAGE ( .BOTH. , #2409 ) ;
#12120 = CARTESIAN_POINT ( 'NONE',  ( 4.763139720814407951, 2.750000000000002665, -165.2500000000000000 ) ) ;
#12121 = CARTESIAN_POINT ( 'NONE',  ( 6.350852961086080661, -9.614813431917819062E-14, -151.8749999999999716 ) ) ;
#12122 = CARTESIAN_POINT ( 'NONE',  ( 112.4999999999999147, -2.499999999999835687, 0.000000000000000000 ) ) ;
#12123 = CARTESIAN_POINT ( 'NONE',  ( 140.6185434356032715, -11.23708687120643646, 4.230991509104588211 ) ) ;
#12124 = CARTESIAN_POINT ( 'NONE',  ( -4.763139720814407951, -2.750000000000016431, -101.5000000000000284 ) ) ;
#12125 = CARTESIAN_POINT ( 'NONE',  ( 142.2113248654052313, 5.500000000000005329, 0.000000000000000000 ) ) ;
#12126 = CARTESIAN_POINT ( 'NONE',  ( 161.5000000000000853, -2.984449860524901688, -5.205099329504969674 ) ) ;
#12127 = CARTESIAN_POINT ( 'NONE',  ( 3.175426480543072749, 5.499999999999865885, -87.12500000000000000 ) ) ;
#12128 =( BOUNDED_CURVE ( )  B_SPLINE_CURVE ( 2, ( #15831, #1338, #15516, #27577, #3932, #13361, #22855, #20254, #24529 ),
 .UNSPECIFIED., .F., .T. ) 
 B_SPLINE_CURVE_WITH_KNOTS ( ( 3, 2, 2, 2, 3 ),
 ( 0.04687500000000000000, 0.05468750000000000000, 0.06250000000000000000, 0.07031250000000000000, 0.07812500000000000000 ),
 .UNSPECIFIED. ) 
 CURVE ( )  GEOMETRIC_REPRESENTATION_ITEM ( )  RATIONAL_B_SPLINE_CURVE ( ( 1.000000000000000000, 0.9238795325112867385, 1.000000000000000000, 0.9238795325112867385, 1.000000000000000000, 0.9238795325112867385, 1.000000000000000000, 0.9238795325112867385, 1.000000000000000000 ) ) 
 REPRESENTATION_ITEM ( '' )  );
#12129 = CARTESIAN_POINT ( 'NONE',  ( -5.999999999999963585, 8.134310703387671600E-14, -136.4136751345948255 ) ) ;
#12130 = UNCERTAINTY_MEASURE_WITH_UNIT (LENGTH_MEASURE( 1.000000000000000082E-05 ), #678, 'distance_accuracy_value', 'NONE');
#12131 = CARTESIAN_POINT ( 'NONE',  ( 113.9374999999997300, 2.500000000000114575, -1.035533905932629173 ) ) ;
#12132 = ADVANCED_FACE ( 'NONE', ( #4902 ), #302, .T. ) ;
#12133 = CARTESIAN_POINT ( 'NONE',  ( -0.5000000000000004441, -10.50000000000000888, 7.500000000000007105 ) ) ;
#12134 = CARTESIAN_POINT ( 'NONE',  ( -5.999999999999971578, 1.607695154586715303, -71.98066243270261566 ) ) ;
#12135 = CARTESIAN_POINT ( 'NONE',  ( 20.53867513459481486, 0.000000000000000000, 2.500000000000002220 ) ) ;
#12136 = ORIENTED_EDGE ( 'NONE', *, *, #21116, .T. ) ;
#12137 = CARTESIAN_POINT ( 'NONE',  ( 118.2886751345946976, 2.000000000000085265, 0.000000000000000000 ) ) ;
#12138 = CARTESIAN_POINT ( 'NONE',  ( -6.000000000000000888, 1.067854986875958443E-15, 7.560779664488942560E-35 ) ) ;
#12139 = CARTESIAN_POINT ( 'NONE',  ( 110.7738248654050608, 2.000000000000061728, 0.8284271247464157772 ) ) ;
#12140 = VERTEX_POINT ( 'NONE', #14758 ) ;
#12141 = EDGE_CURVE ( 'NONE', #3222, #371, #11376, .T. ) ;
#12142 = CARTESIAN_POINT ( 'NONE',  ( 145.3125000000000284, 4.242640687119298093, -4.242640687119298093 ) ) ;
#12143 = VERTEX_POINT ( 'NONE', #19077 ) ;
#12144 = CARTESIAN_POINT ( 'NONE',  ( 3.175426480543072749, -5.500000000000105693, -116.1250000000000000 ) ) ;
#12145 = CARTESIAN_POINT ( 'NONE',  ( 17.25000000000012790, 1.873492889145123019, -1.873492889144956486 ) ) ;
#12146 = CARTESIAN_POINT ( 'NONE',  ( -5.412658773652684552, -3.125000000000099920, -125.9330127018922809 ) ) ;
#12147 = UNCERTAINTY_MEASURE_WITH_UNIT (LENGTH_MEASURE( 1.000000000000000082E-05 ), #28013, 'distance_accuracy_value', 'NONE');
#12148 = ORIENTED_EDGE ( 'NONE', *, *, #22431, .F. ) ;
#12149 = CARTESIAN_POINT ( 'NONE',  ( 114.0863248654051603, -1.414213562373034527, 1.414213562373145550 ) ) ;
#12150 = CARTESIAN_POINT ( 'NONE',  ( -7.216878364870328078, 0.000000000000000000, -159.6919872981078754 ) ) ;
#12151 = CARTESIAN_POINT ( 'NONE',  ( 109.1874999999997584, 1.035533905932839449, 2.500000000000205169 ) ) ;
#12152 = CARTESIAN_POINT ( 'NONE',  ( 132.8288997308104342, 4.999999999999989342, -2.071067811865468400 ) ) ;
#12153 = VECTOR ( 'NONE', #23693, 1000.000000000000000 ) ;
#12154 = VERTEX_POINT ( 'NONE', #28394 ) ;
#12155 = CARTESIAN_POINT ( 'NONE',  ( 158.4449251345948255, -5.500000000000012434, 2.278174593052012309 ) ) ;
#12156 = FACE_OUTER_BOUND ( 'NONE', #29378, .T. ) ;
#12157 = CARTESIAN_POINT ( 'NONE',  ( 4.763139720814407951, 2.750000000000002665, -175.7500000000000284 ) ) ;
#12158 = CARTESIAN_POINT ( 'NONE',  ( 107.4377832217621744, 1.849990392679562001, 0.7662911109080692285 ) ) ;
#12159 = CARTESIAN_POINT ( 'NONE',  ( -9.992007221626473945E-16, 6.000000000000000888, 1.170861610602040338E-13 ) ) ;
#12160 = CARTESIAN_POINT ( 'NONE',  ( -3.608439182435052128, -6.250000000000110134, -173.8080127018922383 ) ) ;
#12161 = CARTESIAN_POINT ( 'NONE',  ( 119.2886751345947260, 1.999999999999946265, 1.110223024625156540E-13 ) ) ;
#12162 = CARTESIAN_POINT ( 'NONE',  ( -6.350852961085760029, -1.281975124255709124E-13, -122.6250000000000426 ) ) ;
#12163 = UNCERTAINTY_MEASURE_WITH_UNIT (LENGTH_MEASURE( 1.000000000000000082E-05 ), #769, 'distance_accuracy_value', 'NONE');
#12164 = CARTESIAN_POINT ( 'NONE',  ( -4.763139720814407951, 2.749999999999946709, -116.7500000000000142 ) ) ;
#12165 = CARTESIAN_POINT ( 'NONE',  ( 135.0000000000000284, -9.047800747816998168, -7.500000000000007105 ) ) ;
#12166 = CARTESIAN_POINT ( 'NONE',  ( 3.464101615137852974, 5.999999999999884537, -100.9136751345948255 ) ) ;
#12167 = ORIENTED_EDGE ( 'NONE', *, *, #12719, .T. ) ;
#12168 = CARTESIAN_POINT ( 'NONE',  ( 17.12500000000011369, -2.649519052838111843, 0.000000000000000000 ) ) ;
#12169 = CARTESIAN_POINT ( 'NONE',  ( -2.117582368135750848E-19, -15.46244542726873306, -5.965557206115555289 ) ) ;
#12170 = EDGE_CURVE ( 'NONE', #7855, #12780, #7416, .T. ) ;
#12171 = CARTESIAN_POINT ( 'NONE',  ( 0.000000000000000000, -5.999999999999991118, -136.9613248654052313 ) ) ;
#12172 = CARTESIAN_POINT ( 'NONE',  ( -4.999999999999886313, -14.50000000000001243, 8.000000000000007105 ) ) ;
#12173 = TOROIDAL_SURFACE ( 'NONE', #16574, 16.50000000000000355, 1.000000000000000000 ) ;
#12174 = AXIS2_PLACEMENT_3D ( 'NONE', #15245, #13113, #8293 ) ;
#12175 = ORIENTED_EDGE ( 'NONE', *, *, #7375, .T. ) ;
#12176 = STYLED_ITEM ( 'NONE', ( #15736 ), #6884 ) ;
#12177 = SURFACE_SIDE_STYLE ('',( #10142 ) ) ;
#12178 = CARTESIAN_POINT ( 'NONE',  ( -3.175426480542816066, -5.500000000000057732, -177.8750000000000284 ) ) ;
#12179 =( BOUNDED_SURFACE ( )  B_SPLINE_SURFACE ( 3, 2, ( 
 ( #28263, #19090, #18790 ),
 ( #16352, #4776, #7391 ),
 ( #11896, #318, #7242 ),
 ( #16650, #463, #12336 ) ),
 .UNSPECIFIED., .F., .F., .F. ) 
 B_SPLINE_SURFACE_WITH_KNOTS ( ( 4, 4 ),
 ( 3, 3 ),
 ( 0.005369593351152912065, 0.006104230743885358246 ),
 ( 0.000000000000000000, 1.000000000000000000 ),
 .UNSPECIFIED. ) 
 GEOMETRIC_REPRESENTATION_ITEM ( )  RATIONAL_B_SPLINE_SURFACE ( (
 ( 1.000000000000000000, 0.7071067811865475727, 1.000000000000000000),
 ( 1.000000000000000000, 0.7328765725615882243, 1.000000000000000000),
 ( 1.000000000000000000, 0.7551281783742019860, 1.000000000000000000),
 ( 1.000000000000000000, 0.7743236465966906179, 1.000000000000000000) ) ) 
 REPRESENTATION_ITEM ( '' )  SURFACE ( )  );
#12180 = DIRECTION ( 'NONE',  ( 0.000000000000000000, 0.000000000000000000, -1.000000000000000000 ) ) ;
#12181 = ORIENTED_EDGE ( 'NONE', *, *, #17955, .T. ) ;
#12182 = EDGE_CURVE ( 'NONE', #20260, #29031, #3454, .T. ) ;
#12183 = CARTESIAN_POINT ( 'NONE',  ( 22.03867513459498184, 1.110223024625156540E-13, -2.500000000000057732 ) ) ;
#12184 = AXIS2_PLACEMENT_3D ( 'NONE', #9215, #6444, #18606 ) ;
#12185 = ORIENTED_EDGE ( 'NONE', *, *, #10200, .F. ) ;
#12186 = EDGE_LOOP ( 'NONE', ( #10696, #8897, #7480, #8613 ) ) ;
#12187 = CARTESIAN_POINT ( 'NONE',  ( 105.9761751345945839, -0.8284271247461453269, -1.999999999999791278 ) ) ;
#12188 = CARTESIAN_POINT ( 'NONE',  ( 135.9523502691896510, 0.000000000000000000, 5.000000000000004441 ) ) ;
#12189 = ORIENTED_EDGE ( 'NONE', *, *, #29631, .F. ) ;
#12190 = CARTESIAN_POINT ( 'NONE',  ( 5.412658773652739619, 3.124999999999988898, -128.8169872981078186 ) ) ;
#12191 = CARTESIAN_POINT ( 'NONE',  ( 11.93750000000008527, -2.649519052838178457, -1.097466725451559322 ) ) ;
#12192 = CARTESIAN_POINT ( 'NONE',  ( 19.02382486540536632, -1.035533905932689347, 2.499999999999904521 ) ) ;
#12193 = ORIENTED_EDGE ( 'NONE', *, *, #1820, .F. ) ;
#12194 = AXIS2_PLACEMENT_3D ( 'NONE', #7616, #15008, #850 ) ;
#12195 = FACE_OUTER_BOUND ( 'NONE', #8179, .T. ) ;
#12196 = LINE ( 'NONE', #23977, #15725 ) ;
#12197 = CARTESIAN_POINT ( 'NONE',  ( 140.7038997308104058, 2.071067811865468400, 4.999999999999989342 ) ) ;
#12198 = DIRECTION ( 'NONE',  ( -0.000000000000000000, 1.000000000000000000, -0.000000000000000000 ) ) ;
#12199 = CARTESIAN_POINT ( 'NONE',  ( 3.464101615137757051, -5.999999999999979572, -99.33632486540518869 ) ) ;
#12200 = CARTESIAN_POINT ( 'NONE',  ( 15.10117513459490013, 1.035533905932809473, -2.499999999999904521 ) ) ;
#12201 = CARTESIAN_POINT ( 'NONE',  ( 24.69040286737535794, -2.307700622106291455, -0.1780978345574568689 ) ) ;
#12202 = CARTESIAN_POINT ( 'NONE',  ( 0.000000000000000000, 5.999999999999977796, -113.7113248654052455 ) ) ;
#12203 = CARTESIAN_POINT ( 'NONE',  ( 107.0624999999998153, 2.500000000000115019, 1.035533905932989551 ) ) ;
#12205 = CARTESIAN_POINT ( 'NONE',  ( 15.52382486540526507, 1.035533905932809473, -2.499999999999904521 ) ) ;
#12204 = VECTOR ( 'NONE', #19826, 1000.000000000000000 ) ;
#12206 = ORIENTED_EDGE ( 'NONE', *, *, #26065, .T. ) ;
#12207 = EDGE_CURVE ( 'NONE', #19051, #16860, #5422, .T. ) ;
#12208 = CARTESIAN_POINT ( 'NONE',  ( 3.175426480543072749, -5.500000000000105693, -47.12500000000006395 ) ) ;
#12209 =( NAMED_UNIT ( * ) PLANE_ANGLE_UNIT ( ) SI_UNIT ( $, .RADIAN. ) );
#12210 = EDGE_CURVE ( 'NONE', #22270, #9839, #17037, .T. ) ;
#12211 = ORIENTED_EDGE ( 'NONE', *, *, #25214, .T. ) ;
#12212 = PRODUCT_RELATED_PRODUCT_CATEGORY ( 'part', '', ( #6474 ) ) ;
#12213 = CARTESIAN_POINT ( 'NONE',  ( 118.3747167782375129, 0.000000000000000000, -1.849990392679301543 ) ) ;
#12214 =( GEOMETRIC_REPRESENTATION_CONTEXT ( 3 ) GLOBAL_UNCERTAINTY_ASSIGNED_CONTEXT ( ( #523 ) ) GLOBAL_UNIT_ASSIGNED_CONTEXT ( ( #26176, #374, #7442 ) ) REPRESENTATION_CONTEXT ( 'NONE', 'WORKASPACE' ) );
#12215 = CARTESIAN_POINT ( 'NONE',  ( 11.87500000000007994, 1.414213562373312083, -1.414213562373090038 ) ) ;
#12216 = CARTESIAN_POINT ( 'NONE',  ( 5.412658773652712085, -3.125000000000086153, -106.5669872981078186 ) ) ;
#12217 =( BOUNDED_CURVE ( )  B_SPLINE_CURVE ( 2, ( #27201, #27500, #12977, #13131, #8633, #22469, #22311, #1563, #6014 ),
 .UNSPECIFIED., .F., .T. ) 
 B_SPLINE_CURVE_WITH_KNOTS ( ( 3, 2, 2, 2, 3 ),
 ( 0.2472222222222222321, 0.2481481481481481177, 0.2500000000000000000, 0.2518518518518518823, 0.2527777777777777679 ),
 .UNSPECIFIED. ) 
 CURVE ( )  GEOMETRIC_REPRESENTATION_ITEM ( )  RATIONAL_B_SPLINE_CURVE ( ( 0.9330127018922194093, 0.9330127018922194093, 1.000000000000000000, 0.8660254037844388186, 1.000000000000000000, 0.8660254037844388186, 1.000000000000000000, 0.9330127018922194093, 0.9330127018922194093 ) ) 
 REPRESENTATION_ITEM ( '' )  );
#12218 = CARTESIAN_POINT ( 'NONE',  ( 161.3288997308104626, 4.999999999999989342, -2.071067811865468400 ) ) ;
#12219 = CARTESIAN_POINT ( 'NONE',  ( 117.1874999999997584, 1.035533905932659149, 2.500000000000205169 ) ) ;
#12220 = CARTESIAN_POINT ( 'NONE',  ( -4.763139720814407951, 2.749999999999946709, -131.7500000000000284 ) ) ;
#12221 = ORIENTED_EDGE ( 'NONE', *, *, #4249, .T. ) ;
#12222 = CIRCLE ( 'NONE', #7736, 0.5000000000000004441 ) ;
#12223 = ORIENTED_EDGE ( 'NONE', *, *, #19829, .F. ) ;
#12224 = FILL_AREA_STYLE ('',( #24001 ) ) ;
#12225 = CARTESIAN_POINT ( 'NONE',  ( -3.175426480542816510, -5.500000000000057732, -57.87500000000004974 ) ) ;
#12226 = CARTESIAN_POINT ( 'NONE',  ( -5.999999999999944933, 1.607695154586759934, -115.4806624327025872 ) ) ;
#12227 = CARTESIAN_POINT ( 'NONE',  ( 6.000000000000000888, 5.577813053751546416E-15, -177.0863248654052597 ) ) ;
#12228 = CARTESIAN_POINT ( 'NONE',  ( 5.412658773652739619, 3.124999999999988898, -84.68301270189226670 ) ) ;
#12229 = UNCERTAINTY_MEASURE_WITH_UNIT (LENGTH_MEASURE( 1.000000000000000082E-05 ), #7162, 'distance_accuracy_value', 'NONE');
#12230 = CARTESIAN_POINT ( 'NONE',  ( -1.110223024625164676E-16, 2.000000000000012879, 2.021286199229734960E-15 ) ) ;
#12231 = CARTESIAN_POINT ( 'NONE',  ( 106.8122167782374277, 0.7662911109079189043, 1.849990392679712103 ) ) ;
#12232 = CARTESIAN_POINT ( 'NONE',  ( 140.5384615384615756, -11.07692307692306777, 4.615384615384604317 ) ) ;
#12233 = CARTESIAN_POINT ( 'NONE',  ( 115.1252832217622881, -2.220446049250313081E-13, -1.849990392679523588 ) ) ;
#12234 = CARTESIAN_POINT ( 'NONE',  ( -2.775557561562891351E-14, -5.500000000000115463, -138.7500000000000284 ) ) ;
#12235 = PLANE ( 'NONE',  #7925 ) ;
#12236 = CARTESIAN_POINT ( 'NONE',  ( -5.412658773652684552, -3.125000000000099920, -149.9330127018922383 ) ) ;
#12237 = CARTESIAN_POINT ( 'NONE',  ( 6.000000000000000888, 1.743066579297358182E-13, -102.0863248654051887 ) ) ;
#12238 = CARTESIAN_POINT ( 'NONE',  ( 146.5238248654052029, 3.889087296526011706, -3.889087296526011706 ) ) ;
#12239 = CARTESIAN_POINT ( 'NONE',  ( -2.775557561562891351E-14, -5.500000000000115463, -74.25000000000004263 ) ) ;
#12240 = CARTESIAN_POINT ( 'NONE',  ( 6.350852961086080661, -9.614813431917819062E-14, -69.37500000000004263 ) ) ;
#12241 = EDGE_CURVE ( 'NONE', #24992, #9072, #12558, .T. ) ;
#12242 = CARTESIAN_POINT ( 'NONE',  ( -3.464101615137725076, 5.999999999999979572, -53.58632486540517448 ) ) ;
#12243 = CARTESIAN_POINT ( 'NONE',  ( 144.7648502691896510, 3.535533905932725318, 3.535533905932752852 ) ) ;
#12244 = CARTESIAN_POINT ( 'NONE',  ( -4.999999999999990230, -24.99999999999999289, 7.500000000000007105 ) ) ;
#12245 = CARTESIAN_POINT ( 'NONE',  ( 150.6562500000000568, -6.000000000000005329, 2.485281374238556218 ) ) ;
#12246 = DIRECTION ( 'NONE',  ( 0.000000000000000000, 1.000000000000000000, -0.000000000000000000 ) ) ;
#12247 = CARTESIAN_POINT ( 'NONE',  ( 3.464101615137757051, -5.999999999999979572, -147.3363248654051745 ) ) ;
#12248 = CARTESIAN_POINT ( 'NONE',  ( 115.7497167782375698, 1.308140751793751555, 1.308140751793973600 ) ) ;
#12249 = CARTESIAN_POINT ( 'NONE',  ( -5.999999999999982236, -1.607695154586700426, -145.3466878364870354 ) ) ;
#12250 = ORIENTED_EDGE ( 'NONE', *, *, #26126, .T. ) ;
#12251 = CARTESIAN_POINT ( 'NONE',  ( 150.6562500000000284, -6.000000000000005329, 2.485281374238555774 ) ) ;
#12252 = CARTESIAN_POINT ( 'NONE',  ( 119.9999999999997868, 1.387778780781445676E-13, 1.110223024625156540E-13 ) ) ;
#12253 = UNCERTAINTY_MEASURE_WITH_UNIT (LENGTH_MEASURE( 1.000000000000000082E-05 ), #4803, 'distance_accuracy_value', 'NONE');
#12254 = CARTESIAN_POINT ( 'NONE',  ( 104.4999999999998863, -2.499999999999919176, 0.000000000000000000 ) ) ;
#12255 = CARTESIAN_POINT ( 'NONE',  ( 4.763139720814407951, -2.749999999999988454, -177.5000000000000000 ) ) ;
#12256 = CARTESIAN_POINT ( 'NONE',  ( 20.68750000000011369, -0.8284271247459952248, -1.999999999999971800 ) ) ;
#12257 = VERTEX_POINT ( 'NONE', #29298 ) ;
#12258 = CARTESIAN_POINT ( 'NONE',  ( 6.350852961086080661, -9.614813431917819062E-14, -81.37500000000004263 ) ) ;
#12259 = FACE_OUTER_BOUND ( 'NONE', #6722, .T. ) ;
#12260 = EDGE_CURVE ( 'NONE', #42, #4270, #21659, .T. ) ;
#12261 = CARTESIAN_POINT ( 'NONE',  ( -2.775557561562891351E-14, -5.500000000000115463, -168.7500000000000000 ) ) ;
#12262 = CARTESIAN_POINT ( 'NONE',  ( 6.000000000000000888, 1.607695154586715303, -54.59668783648703538 ) ) ;
#12263 = CARTESIAN_POINT ( 'NONE',  ( 5.196152422706629359, 3.000000000000002665, -59.03867513459481842 ) ) ;
#12264 = CARTESIAN_POINT ( 'NONE',  ( 111.5238248654049329, 0.8284271247462955401, -1.999999999999791278 ) ) ;
#12265 =( NAMED_UNIT ( * ) SI_UNIT ( $, .STERADIAN. ) SOLID_ANGLE_UNIT ( ) );
#12266 = CARTESIAN_POINT ( 'NONE',  ( -4.763139720814407951, 2.749999999999946709, -163.2500000000000000 ) ) ;
#12267 = CARTESIAN_POINT ( 'NONE',  ( 0.000000000000000000, 5.999999999999977796, -161.7113248654051745 ) ) ;
#12268 = CARTESIAN_POINT ( 'NONE',  ( -3.175426480542816510, 5.499999999999865885, -154.3749999999999716 ) ) ;
#12269 = CARTESIAN_POINT ( 'NONE',  ( -5.196152422706601826, 2.999999999999975131, -76.53867513459483973 ) ) ;
#12270 = CARTESIAN_POINT ( 'NONE',  ( 140.7917870674316987, -11.58357413486331566, 4.000000000000005329 ) ) ;
#12271 = PRESENTATION_LAYER_ASSIGNMENT (  '', '', ( #9785 ) ) ;
#12272 = CARTESIAN_POINT ( 'NONE',  ( 0.000000000000000000, 5.499999999999991118, -97.50000000000002842 ) ) ;
#12273 = CARTESIAN_POINT ( 'NONE',  ( 145.1324251345948539, -5.500000000000012434, -2.278174593052012309 ) ) ;
#12274 = CARTESIAN_POINT ( 'NONE',  ( -4.763139720814407951, -2.750000000000016431, -88.00000000000002842 ) ) ;
#12275 = EDGE_CURVE ( 'NONE', #1827, #9271, #24264, .T. ) ;
#12276 = CARTESIAN_POINT ( 'NONE',  ( 135.6488248654052597, -3.889087296526011706, -3.889087296526011706 ) ) ;
#12277 = CARTESIAN_POINT ( 'NONE',  ( 157.7023502691896510, 0.000000000000000000, -5.000000000000004441 ) ) ;
#12278 = CARTESIAN_POINT ( 'NONE',  ( 109.3988248654050039, -0.8284271247461453269, -1.999999999999731104 ) ) ;
#12279 = CARTESIAN_POINT ( 'NONE',  ( 114.2499999999999147, -1.110223024625156540E-13, 2.500000000000057732 ) ) ;
#12280 = CARTESIAN_POINT ( 'NONE',  ( 6.000000000000000888, 1.607695154586715303, -126.5966878364870638 ) ) ;
#12281 = CARTESIAN_POINT ( 'NONE',  ( 6.000000000000052403, -1.607695154586662678, -73.65331216351297883 ) ) ;
#12282 = CARTESIAN_POINT ( 'NONE',  ( 20.47617513459485394, 1.035533905932869425, 2.499999999999904521 ) ) ;
#12283 = ORIENTED_EDGE ( 'NONE', *, *, #9647, .T. ) ;
#12284 = SURFACE_STYLE_FILL_AREA ( #23776 ) ;
#12285 = FACE_OUTER_BOUND ( 'NONE', #10944, .T. ) ;
#12286 = CARTESIAN_POINT ( 'NONE',  ( 121.0002832217622739, -1.308140751793557266, -1.308140751793529510 ) ) ;
#12287 = VERTEX_POINT ( 'NONE', #7959 ) ;
#12288 = CARTESIAN_POINT ( 'NONE',  ( 145.2187500000000000, 2.485281374238555774, -6.000000000000005329 ) ) ;
#12289 = CARTESIAN_POINT ( 'NONE',  ( -6.350852961085760029, -1.281975124255709124E-13, -106.1250000000000142 ) ) ;
#12290 = VECTOR ( 'NONE', #22390, 1000.000000000000000 ) ;
#12291 = CARTESIAN_POINT ( 'NONE',  ( 18.37500000000011369, 2.649519052838444910, -1.110223024625156540E-13 ) ) ;
#12292 = CARTESIAN_POINT ( 'NONE',  ( 2.775557561562891351E-14, 6.250000000000033751, -121.9330127018922667 ) ) ;
#12293 = ORIENTED_EDGE ( 'NONE', *, *, #5754, .T. ) ;
#12294 = AXIS2_PLACEMENT_3D ( 'NONE', #20460, #10968, #29819 ) ;
#12295 = CARTESIAN_POINT ( 'NONE',  ( 5.412658773652739619, 3.124999999999988898, -161.8169872981078470 ) ) ;
#12296 = CARTESIAN_POINT ( 'NONE',  ( 108.5000000000000000, -2.500000000000002220, 2.220446049250313081E-13 ) ) ;
#12297 = AXIS2_PLACEMENT_3D ( 'NONE', #17016, #14703, #24049 ) ;
#12298 = CARTESIAN_POINT ( 'NONE',  ( 134.0476497308104058, 0.000000000000000000, -5.000000000000004441 ) ) ;
#12299 = EDGE_CURVE ( 'NONE', #14750, #11534, #1659, .T. ) ;
#12300 = CARTESIAN_POINT ( 'NONE',  ( 7.216878364870455975, -6.409875621278545621E-14, -57.80801270189221697 ) ) ;
#12301 = ORIENTED_EDGE ( 'NONE', *, *, #11615, .F. ) ;
#12302 = FACE_OUTER_BOUND ( 'NONE', #3504, .T. ) ;
#12303 =( BOUNDED_CURVE ( )  B_SPLINE_CURVE ( 2, ( #29883, #1629, #1473, #29729, #27562, #14518, #2947, #5091, #19410 ),
 .UNSPECIFIED., .F., .T. ) 
 B_SPLINE_CURVE_WITH_KNOTS ( ( 3, 2, 2, 2, 3 ),
 ( 0.6305555555555556468, 0.6314814814814815325, 0.6333333333333333037, 0.6351851851851851860, 0.6361111111111110716 ),
 .UNSPECIFIED. ) 
 CURVE ( )  GEOMETRIC_REPRESENTATION_ITEM ( )  RATIONAL_B_SPLINE_CURVE ( ( 0.9330127018922194093, 0.9330127018922234061, 1.000000000000000000, 0.8660254037844388186, 1.000000000000000000, 0.8660254037844388186, 1.000000000000000000, 0.9330127018922234061, 0.9330127018922194093 ) ) 
 REPRESENTATION_ITEM ( '' )  );
#12304 = DIRECTION ( 'NONE',  ( -7.147005652999508048E-36, 5.642372883946980038E-36, 1.000000000000000000 ) ) ;
#12305 = CARTESIAN_POINT ( 'NONE',  ( 6.000000000000000000, 2.951592740943527306E-14, -156.0863248654052597 ) ) ;
#12306 = CARTESIAN_POINT ( 'NONE',  ( 4.763139720814407951, 2.750000000000002665, -180.2500000000000284 ) ) ;
#12307 = CARTESIAN_POINT ( 'NONE',  ( 107.3752832217621886, 1.849990392679523588, 0.000000000000000000 ) ) ;
#12308 = CARTESIAN_POINT ( 'NONE',  ( -7.216878364870328078, 0.000000000000000000, -178.5580127018922383 ) ) ;
#12309 = CARTESIAN_POINT ( 'NONE',  ( 6.000000000000000888, -6.507448562710137091E-15, -176.1636751345947971 ) ) ;
#12310 = CARTESIAN_POINT ( 'NONE',  ( 0.000000000000000000, -5.999999999999991118, -101.5386751345947971 ) ) ;
#12311 = CARTESIAN_POINT ( 'NONE',  ( -6.350852961085760029, -1.281975124255709124E-13, -113.6249999999999858 ) ) ;
#12312 = CARTESIAN_POINT ( 'NONE',  ( -5.999999999999919176, 1.607695154586804565, -83.98066243270260145 ) ) ;
#12313 = EDGE_CURVE ( 'NONE', #2458, #19518, #24099, .T. ) ;
#12314 = CARTESIAN_POINT ( 'NONE',  ( -3.175426480542816510, -5.500000000000057732, -113.3750000000000568 ) ) ;
#12315 = CARTESIAN_POINT ( 'NONE',  ( 6.000000000000000888, -1.607695154586752384, -131.2306624327026441 ) ) ;
#12316 = ORIENTED_EDGE ( 'NONE', *, *, #21573, .T. ) ;
#12317 = CARTESIAN_POINT ( 'NONE',  ( 0.1950273200666236550, -15.66255992321437951, 7.807776097887586531 ) ) ;
#12318 = MECHANICAL_DESIGN_GEOMETRIC_PRESENTATION_REPRESENTATION (  '', ( #25508 ), #10838 ) ;
#12319 = CARTESIAN_POINT ( 'NONE',  ( 3.464101615137757051, -5.999999999999979572, -145.8363248654052029 ) ) ;
#12320 = AXIS2_PLACEMENT_3D ( 'NONE', #7314, #9057, #26046 ) ;
#12321 = ORIENTED_EDGE ( 'NONE', *, *, #22224, .T. ) ;
#12322 = CARTESIAN_POINT ( 'NONE',  ( -5.999999999999956479, -1.607695154586745057, -126.7693375672974838 ) ) ;
#12323 = CARTESIAN_POINT ( 'NONE',  ( 4.763139720814407951, 2.750000000000002665, -177.2500000000000284 ) ) ;
#12324 = CARTESIAN_POINT ( 'NONE',  ( 22.77382486540519224, 2.500000000000144773, 1.035533905932689347 ) ) ;
#12325 = ORIENTED_EDGE ( 'NONE', *, *, #18332, .T. ) ;
#12326 = ORIENTED_EDGE ( 'NONE', *, *, #13916, .T. ) ;
#12327 = CARTESIAN_POINT ( 'NONE',  ( -3.464101615137725076, 5.999999999999979572, -85.08632486540520290 ) ) ;
#12328 = CARTESIAN_POINT ( 'NONE',  ( 160.7812500000000568, 2.485281374238585972, 6.000000000000005329 ) ) ;
#12329 = ORIENTED_EDGE ( 'NONE', *, *, #23170, .F. ) ;
#12330 = CARTESIAN_POINT ( 'NONE',  ( 3.608439182435180470, 6.249999999999982236, -131.6919872981078470 ) ) ;
#12331 = DIRECTION ( 'NONE',  ( 1.734723475976843579E-16, -1.000000000000000000, 0.000000000000000000 ) ) ;
#12332 = CARTESIAN_POINT ( 'NONE',  ( -5.999999999999956479, -1.607695154586745057, -167.8466878364870354 ) ) ;
#12333 = DIRECTION ( 'NONE',  ( 1.000000000000000000, 0.000000000000000000, 0.000000000000000000 ) ) ;
#12334 = EDGE_CURVE ( 'NONE', #21338, #13036, #29477, .T. ) ;
#12335 = VERTEX_POINT ( 'NONE', #8573 ) ;
#12336 = CARTESIAN_POINT ( 'NONE',  ( 0.8631338372299254269, -15.37878787878792686, 8.351220472436690301 ) ) ;
#12337 = CARTESIAN_POINT ( 'NONE',  ( 139.9538997308103774, -2.071067811865468400, -4.999999999999989342 ) ) ;
#12338 = DIRECTION ( 'NONE',  ( -7.147005652999508048E-36, 5.642372883946980038E-36, 1.000000000000000000 ) ) ;
#12339 = CARTESIAN_POINT ( 'NONE',  ( 6.000000000000000888, -1.859271017917181981E-14, -114.0863248654052029 ) ) ;
#12340 = CARTESIAN_POINT ( 'NONE',  ( 104.8749999999998437, 1.767766952966320915, -1.767766952966431937 ) ) ;
#12341 = B_SPLINE_CURVE_WITH_KNOTS ( 'NONE', 3,
 ( #13011, #8831, #20496, #20206, #6207, #15783, #27534, #27086, #1283, #1749, #1444, #17920, #8356, #29389, #15934, #22808, #10697, #3886, #24936, #20659, #6511, #25229, #13174, #20043, #22659, #24637, #11148, #18070, #22512, #15312, #4200, #29556, #13617, #15627, #3583, #25089, #4045, #22964 ),
 .UNSPECIFIED., .F., .F.,
 ( 4, 2, 2, 2, 2, 2, 2, 2, 2, 2, 2, 2, 2, 2, 2, 2, 2, 2, 4 ),
 ( 0.01915730813553680537, 0.01975454893833630127, 0.02035178974113580064, 0.02154627134673479244, 0.02274075295233378424, 0.02393523455793277604, 0.02512971616353176785, 0.02632419776913075965, 0.02751867937472975145, 0.02871316098032874325, 0.02990764258592773506, 0.03110212419152672686, 0.03229660579712571866, 0.03349108740272471046, 0.03468556900832370227, 0.03528280981112319470, 0.03588005061392268713, 0.03707453221952168587, 0.03826901382512067074 ),
 .UNSPECIFIED. ) ;
#12342 = EDGE_CURVE ( 'NONE', #13173, #14623, #15287, .T. ) ;
#12343 = CARTESIAN_POINT ( 'NONE',  ( -3.175426480542816510, -5.500000000000057732, -140.3750000000000568 ) ) ;
#12344 = VECTOR ( 'NONE', #10044, 1000.000000000000000 ) ;
#12345 = DIRECTION ( 'NONE',  ( -7.147005652999508048E-36, 5.642372883946980038E-36, 1.000000000000000000 ) ) ;
#12346 = ORIENTED_EDGE ( 'NONE', *, *, #2292, .F. ) ;
#12347 =( BOUNDED_CURVE ( )  B_SPLINE_CURVE ( 2, ( #8012, #10495, #12522, #12976, #3392, #10340, #17420, #804, #3699 ),
 .UNSPECIFIED., .F., .F. ) 
 B_SPLINE_CURVE_WITH_KNOTS ( ( 3, 2, 2, 2, 3 ),
 ( 0.03611111111111109384, 0.03703703703703709049, 0.03888888888888886175, 0.04074074074074074403, 0.04166666666666674068 ),
 .UNSPECIFIED. ) 
 CURVE ( )  GEOMETRIC_REPRESENTATION_ITEM ( )  RATIONAL_B_SPLINE_CURVE ( ( 0.9330127018922194093, 0.9330127018922154125, 1.000000000000000000, 0.8660254037844388186, 1.000000000000000000, 0.8660254037844388186, 1.000000000000000000, 0.9330127018922154125, 0.9330127018922194093 ) ) 
 REPRESENTATION_ITEM ( '' )  );
#12348 = CARTESIAN_POINT ( 'NONE',  ( -3.175426480542816066, -5.500000000000057732, -50.37500000000001421 ) ) ;
#12349 = FACE_OUTER_BOUND ( 'NONE', #17494, .T. ) ;
#12350 = CARTESIAN_POINT ( 'NONE',  ( -5.999999999999963585, 1.780251999655701777E-13, -102.8363248654052313 ) ) ;
#12351 = VERTEX_POINT ( 'NONE', #13682 ) ;
#12352 = CARTESIAN_POINT ( 'NONE',  ( 117.6872167782374845, 1.849990392679621953, 0.7662911109078287542 ) ) ;
#12353 = CARTESIAN_POINT ( 'NONE',  ( 109.2113248654051745, -1.999999999999946265, 0.000000000000000000 ) ) ;
#12354 = CARTESIAN_POINT ( 'NONE',  ( 5.412658773652739619, 3.124999999999988898, -97.31698729810783277 ) ) ;
#12355 = CIRCLE ( 'NONE', #26532, 5.000000000000001776 ) ;
#12356 = CARTESIAN_POINT ( 'NONE',  ( 20.58632486540526330, 1.767766952966487448, -1.767766952966376426 ) ) ;
#12357 = CARTESIAN_POINT ( 'NONE',  ( 117.6874999999997726, -1.035533905932719101, -2.499999999999844569 ) ) ;
#12358 = DIRECTION ( 'NONE',  ( 1.000000000000000000, 0.000000000000000000, 0.000000000000000000 ) ) ;
#12359 = VECTOR ( 'NONE', #881, 1000.000000000000000 ) ;
#12360 = CARTESIAN_POINT ( 'NONE',  ( 4.763139720814407951, -2.749999999999988454, -128.0000000000000000 ) ) ;
#12361 = ORIENTED_EDGE ( 'NONE', *, *, #22612, .F. ) ;
#12362 = PLANE ( 'NONE',  #5227 ) ;
#12363 = CARTESIAN_POINT ( 'NONE',  ( -2.775557561562891351E-14, -5.500000000000115463, -59.25000000000002842 ) ) ;
#12364 = EDGE_CURVE ( 'NONE', #14656, #15734, #27223, .T. ) ;
#12365 = DIRECTION ( 'NONE',  ( -1.000000000000000000, 0.000000000000000000, 0.000000000000000000 ) ) ;
#12366 = CARTESIAN_POINT ( 'NONE',  ( 140.5126539824821634, -11.05214782318283184, -4.674845224361170004 ) ) ;
#12367 = CARTESIAN_POINT ( 'NONE',  ( 5.999340830937940794, 9.219973438021412449, -24.59179872956898549 ) ) ;
#12368 = ADVANCED_FACE ( 'NONE', ( #13529 ), #27748, .F. ) ;
#12369 = CARTESIAN_POINT ( 'NONE',  ( 5.412658773652739619, 3.124999999999988898, -83.18301270189220986 ) ) ;
#12370 = CARTESIAN_POINT ( 'NONE',  ( 6.000000000000000888, -1.859271017917181981E-14, -100.5863248654052171 ) ) ;
#12371 = DIRECTION ( 'NONE',  ( -7.147005652999508048E-36, 5.642372883946980038E-36, 1.000000000000000000 ) ) ;
#12372 = CARTESIAN_POINT ( 'NONE',  ( 140.4831164018241054, -11.48311640182297388, -4.126236462591093002 ) ) ;
#12373 =( GEOMETRIC_REPRESENTATION_CONTEXT ( 3 ) GLOBAL_UNCERTAINTY_ASSIGNED_CONTEXT ( ( #18916 ) ) GLOBAL_UNIT_ASSIGNED_CONTEXT ( ( #19637, #7356, #4883 ) ) REPRESENTATION_CONTEXT ( 'NONE', 'WORKASPACE' ) );
#12374 = LINE ( 'NONE', #21722, #12344 ) ;
#12375 = CARTESIAN_POINT ( 'NONE',  ( 115.6877832217621744, -0.7662911109077087390, 1.849990392679712103 ) ) ;
#12376 = CARTESIAN_POINT ( 'NONE',  ( 0.000000000000000000, 5.499999999999991118, -136.5000000000000000 ) ) ;
#12377 = CARTESIAN_POINT ( 'NONE',  ( 139.8749506744242410, -9.075050735211396713, 7.854018104365544595 ) ) ;
#12378 = CIRCLE ( 'NONE', #29505, 28.99999999999999645 ) ;
#12379 = CARTESIAN_POINT ( 'NONE',  ( 3.608439182435180470, -6.249999999999997335, -151.0580127018922951 ) ) ;
#12380 = DIRECTION ( 'NONE',  ( 0.000000000000000000, 1.000000000000000000, -1.224646799147353207E-16 ) ) ;
#12381 = CARTESIAN_POINT ( 'NONE',  ( 146.4300748654051745, 2.278174593051733421, -5.500000000000292211 ) ) ;
#12382 = CARTESIAN_POINT ( 'NONE',  ( 0.000000000000000000, 5.499999999999991118, -67.50000000000000000 ) ) ;
#12383 = CARTESIAN_POINT ( 'NONE',  ( 0.000000000000000000, 5.999999999999977796, -85.78867513459481131 ) ) ;
#12384 = CARTESIAN_POINT ( 'NONE',  ( -4.763139720814407951, 2.749999999999946709, -59.75000000000002842 ) ) ;
#12385 =( BOUNDED_CURVE ( )  B_SPLINE_CURVE ( 2, ( #4227, #22832, #23150, #15805, #4538, #27872, #13645, #6374, #18699 ),
 .UNSPECIFIED., .F., .F. ) 
 B_SPLINE_CURVE_WITH_KNOTS ( ( 3, 2, 2, 2, 3 ),
 ( 0.5361111111111110938, 0.5370370370370370905, 0.5388888888888888618, 0.5407407407407407440, 0.5416666666666667407 ),
 .UNSPECIFIED. ) 
 CURVE ( )  GEOMETRIC_REPRESENTATION_ITEM ( )  RATIONAL_B_SPLINE_CURVE ( ( 0.9330127018922194093, 0.9330127018922154125, 1.000000000000000000, 0.8660254037844388186, 1.000000000000000000, 0.8660254037844388186, 1.000000000000000000, 0.9330127018922154125, 0.9330127018922194093 ) ) 
 REPRESENTATION_ITEM ( '' )  );
#12386 = CARTESIAN_POINT ( 'NONE',  ( 0.000000000000000000, 5.999999999999977796, -53.71132486540519579 ) ) ;
#12387 = CARTESIAN_POINT ( 'NONE',  ( 146.0773502691896510, 5.000000000000004441, 0.000000000000000000 ) ) ;
#12388 = AXIS2_PLACEMENT_3D ( 'NONE', #20362, #20060, #27105 ) ;
#12389 = CARTESIAN_POINT ( 'NONE',  ( 150.9375000000000284, -4.242640687119298093, -4.242640687119298093 ) ) ;
#12390 = DIRECTION ( 'NONE',  ( 0.7071067811865555663, 8.659560562354835483E-17, 0.7071067811865394681 ) ) ;
#12391 = VECTOR ( 'NONE', #10386, 1000.000000000000000 ) ;
#12392 = DIRECTION ( 'NONE',  ( -7.147005652999508048E-36, 5.642372883946980038E-36, 1.000000000000000000 ) ) ;
#12393 = CARTESIAN_POINT ( 'NONE',  ( 115.9997167782376266, -1.308140751793668288, 1.308140751793751555 ) ) ;
#12394 = ORIENTED_EDGE ( 'NONE', *, *, #7774, .T. ) ;
#12395 = CARTESIAN_POINT ( 'NONE',  ( 143.1562500000000284, -6.000000000000005329, 2.485281374238555774 ) ) ;
#12396 = AXIS2_PLACEMENT_3D ( 'NONE', #14203, #6634, #25830 ) ;
#12397 = CARTESIAN_POINT ( 'NONE',  ( -5.196152422706601826, 2.999999999999975131, -63.96132486540523132 ) ) ;
#12398 = CARTESIAN_POINT ( 'NONE',  ( 3.175426480543072749, 5.499999999999865885, -177.1250000000000284 ) ) ;
#12399 = CARTESIAN_POINT ( 'NONE',  ( 20.31250000000011724, -0.8284271247461153509, 2.000000000000031530 ) ) ;
#12400 = CARTESIAN_POINT ( 'NONE',  ( -5.412658773652684552, -3.125000000000099920, -153.5669872981077901 ) ) ;
#12401 = ORIENTED_EDGE ( 'NONE', *, *, #12104, .T. ) ;
#12402 = CARTESIAN_POINT ( 'NONE',  ( 6.350852961086080661, -9.614813431917819062E-14, -79.87500000000001421 ) ) ;
#12403 = EDGE_CURVE ( 'NONE', #3266, #22716, #14697, .T. ) ;
#12404 = CARTESIAN_POINT ( 'NONE',  ( 15.68750000000015277, -1.097466725451499370, 2.649519052838118061 ) ) ;
#12405 = EDGE_CURVE ( 'NONE', #14826, #5798, #682, .T. ) ;
#12406 = ORIENTED_EDGE ( 'NONE', *, *, #12334, .T. ) ;
#12407 = DIRECTION ( 'NONE',  ( -1.000000000000000000, -1.665334536937731113E-16, 1.526556658859586792E-16 ) ) ;
#12408 = CARTESIAN_POINT ( 'NONE',  ( 0.000000000000000000, 5.499999999999991118, -168.0000000000000284 ) ) ;
#12409 = CARTESIAN_POINT ( 'NONE',  ( 0.000000000000000000, 0.000000000000000000, 0.000000000000000000 ) ) ;
#12410 = CARTESIAN_POINT ( 'NONE',  ( 5.841785975170685319, -9.320713607846709436, -23.61690496628340341 ) ) ;
#12411 = CARTESIAN_POINT ( 'NONE',  ( 111.7113248654050892, 2.000000000000057288, 0.000000000000000000 ) ) ;
#12412 = CARTESIAN_POINT ( 'NONE',  ( 134.9273262448254798, -7.354674723977097983, 8.000000000000005329 ) ) ;
#12413 = CARTESIAN_POINT ( 'NONE',  ( 0.000000000000000000, 5.499999999999991118, -166.4999999999999716 ) ) ;
#12414 = CARTESIAN_POINT ( 'NONE',  ( -5.999999999999962697, 3.323446944526963260E-14, -161.3363248654052597 ) ) ;
#12415 = CARTESIAN_POINT ( 'NONE',  ( 0.000000000000000000, 5.499999999999991118, -150.0000000000000284 ) ) ;
#12416 = CARTESIAN_POINT ( 'NONE',  ( 104.4999999999998863, -2.499999999999919176, 0.000000000000000000 ) ) ;
#12417 = CARTESIAN_POINT ( 'NONE',  ( 6.350852961086080661, -9.614813431917819062E-14, -94.87500000000001421 ) ) ;
#12418 = CARTESIAN_POINT ( 'NONE',  ( 145.0386751345948539, -5.500000000000005329, 0.000000000000000000 ) ) ;
#12419 = CARTESIAN_POINT ( 'NONE',  ( -3.175426480542816510, 5.499999999999865885, -88.37500000000000000 ) ) ;
#12420 = CARTESIAN_POINT ( 'NONE',  ( 157.6086002691896795, -2.071067811865468400, -4.999999999999989342 ) ) ;
#12421 = CARTESIAN_POINT ( 'NONE',  ( -5.999999999999919176, 1.607695154586804565, -64.48066243270261566 ) ) ;
#12422 = DIRECTION ( 'NONE',  ( -0.000000000000000000, -0.000000000000000000, 1.000000000000000000 ) ) ;
#12423 = CARTESIAN_POINT ( 'NONE',  ( 9.687499999999998224, 2.649519052838419153, 1.097466725451499370 ) ) ;
#12424 = CARTESIAN_POINT ( 'NONE',  ( 110.6874999999997868, -1.035533905932689347, -2.499999999999844569 ) ) ;
#12425 = FACE_OUTER_BOUND ( 'NONE', #7258, .T. ) ;
#12426 = LINE ( 'NONE', #5453, #7603 ) ;
#12427 = VERTEX_POINT ( 'NONE', #7336 ) ;
#12428 = FACE_OUTER_BOUND ( 'NONE', #21178, .T. ) ;
#12429 = CARTESIAN_POINT ( 'NONE',  ( -5.999999999999971578, 1.607695154586715303, -80.40331216351302146 ) ) ;
#12430 = CARTESIAN_POINT ( 'NONE',  ( 120.1877832217620750, 0.7662911109077987781, -1.849990392679532247 ) ) ;
#12431 = EDGE_LOOP ( 'NONE', ( #10687, #14120, #8504, #30388 ) ) ;
#12432 = EDGE_LOOP ( 'NONE', ( #10551, #15536, #15918, #27667 ) ) ;
#12433 = B_SPLINE_CURVE_WITH_KNOTS ( 'NONE', 3,
 ( #10433, #5190, #17358, #26674, #19354, #22099, #17505, #1033, #5635, #9977, #21948, #23801 ),
 .UNSPECIFIED., .F., .F.,
 ( 4, 2, 2, 2, 2, 4 ),
 ( 0.000000000000000000, 0.0005736249320795650149, 0.001147249864159130030, 0.001720874796238695045, 0.002007687262278479504, 0.002294499728318263529 ),
 .UNSPECIFIED. ) ;
#12434 = CARTESIAN_POINT ( 'NONE',  ( -4.763139720814407951, 2.749999999999946709, -103.2500000000000142 ) ) ;
#12435 = CARTESIAN_POINT ( 'NONE',  ( 17.93750000000006395, -2.649519052838178457, -1.097466725451559322 ) ) ;
#12436 = ADVANCED_FACE ( 'NONE', ( #26358 ), #4720, .F. ) ;
#12437 = CARTESIAN_POINT ( 'NONE',  ( 3.608439182435180470, -6.249999999999997335, -119.5580127018922525 ) ) ;
#12438 = EDGE_LOOP ( 'NONE', ( #22138, #21035, #4413, #16001 ) ) ;
#12439 = CARTESIAN_POINT ( 'NONE',  ( 4.763139720814407951, -2.749999999999988454, -152.0000000000000284 ) ) ;
#12440 = CARTESIAN_POINT ( 'NONE',  ( 114.2113248654050750, -1.999999999999890754, 0.000000000000000000 ) ) ;
#12441 = CARTESIAN_POINT ( 'NONE',  ( 5.412658773652739619, 3.124999999999988898, -157.3169872981078470 ) ) ;
#12442 = CARTESIAN_POINT ( 'NONE',  ( 105.1249999999999005, 1.767766952966265404, 1.767766952966431937 ) ) ;
#12443 = CARTESIAN_POINT ( 'NONE',  ( 132.1726497308104058, -5.000000000000004441, 0.000000000000000000 ) ) ;
#12444 = CARTESIAN_POINT ( 'NONE',  ( -5.412658773652684552, -3.125000000000099920, -56.93301270189221697 ) ) ;
#12445 = ORIENTED_EDGE ( 'NONE', *, *, #17139, .T. ) ;
#12446 = CARTESIAN_POINT ( 'NONE',  ( 0.1513474785670624878, -15.31721424822544542, -8.468282902864297412 ) ) ;
#12447 =( GEOMETRIC_REPRESENTATION_CONTEXT ( 3 ) GLOBAL_UNCERTAINTY_ASSIGNED_CONTEXT ( ( #12229 ) ) GLOBAL_UNIT_ASSIGNED_CONTEXT ( ( #7162, #21608, #12265 ) ) REPRESENTATION_CONTEXT ( 'NONE', 'WORKASPACE' ) );
#12448 = CARTESIAN_POINT ( 'NONE',  ( -4.999999999999886313, -10.50000000000000888, -7.500000000000007105 ) ) ;
#12449 = CARTESIAN_POINT ( 'NONE',  ( 141.3675748654052313, -5.500000000000012434, 2.278174593052012309 ) ) ;
#12450 = CARTESIAN_POINT ( 'NONE',  ( 0.000000000000000000, 0.000000000000000000, 0.000000000000000000 ) ) ;
#12451 = CARTESIAN_POINT ( 'NONE',  ( 105.7502832217622597, -1.308140751793557266, 1.308140751793751555 ) ) ;
#12452 = CARTESIAN_POINT ( 'NONE',  ( 153.0863248654052313, 0.000000000000000000, 5.500000000000005329 ) ) ;
#12453 = CARTESIAN_POINT ( 'NONE',  ( 5.412658773652739619, 3.124999999999988898, -168.6830127018922383 ) ) ;
#12454 = LINE ( 'NONE', #14465, #6740 ) ;
#12455 = CARTESIAN_POINT ( 'NONE',  ( 23.75000000000013145, 1.665334536937734811E-13, -2.000000000000057288 ) ) ;
#12456 = CARTESIAN_POINT ( 'NONE',  ( -4.763139720814407951, 2.749999999999946709, -115.2500000000000142 ) ) ;
#12457 = CARTESIAN_POINT ( 'NONE',  ( 159.7574251345948824, -2.278174593051888408, 5.500000000000135891 ) ) ;
#12458 = CARTESIAN_POINT ( 'NONE',  ( -6.350852961085760029, -1.281975124255709124E-13, -112.1249999999999858 ) ) ;
#12459 =( LENGTH_UNIT ( ) NAMED_UNIT ( * ) SI_UNIT ( .MILLI., .METRE. ) );
#12460 = DIRECTION ( 'NONE',  ( -7.147005652999508048E-36, 5.642372883946980038E-36, 1.000000000000000000 ) ) ;
#12461 = CARTESIAN_POINT ( 'NONE',  ( 148.8824251345948824, 5.500000000000012434, 2.278174593052012309 ) ) ;
#12462 = ORIENTED_EDGE ( 'NONE', *, *, #16059, .F. ) ;
#12463 = CARTESIAN_POINT ( 'NONE',  ( 18.18750000000000000, -2.649519052838298805, -1.097466725451559322 ) ) ;
#12464 = CARTESIAN_POINT ( 'NONE',  ( 120.4999999999998437, -2.499999999999891198, 3.330669073875469621E-13 ) ) ;
#12465 = CARTESIAN_POINT ( 'NONE',  ( 0.000000000000000000, 10.00000000000000888, 3.000000000000002665 ) ) ;
#12466 = AXIS2_PLACEMENT_3D ( 'NONE', #5079, #11915, #331 ) ;
#12467 = CARTESIAN_POINT ( 'NONE',  ( 5.999999999999999112, 2.951592740943527306E-14, -153.0863248654052313 ) ) ;
#12468 = ORIENTED_EDGE ( 'NONE', *, *, #12853, .F. ) ;
#12469 = CARTESIAN_POINT ( 'NONE',  ( 111.3511751345947829, 2.000000000000061728, 0.8284271247462955401 ) ) ;
#12470 = ADVANCED_FACE ( 'NONE', ( #28058 ), #23923, .T. ) ;
#12471 = CARTESIAN_POINT ( 'NONE',  ( 17.03867513459494987, 1.665334536937734811E-13, -2.500000000000002220 ) ) ;
#12472 = ADVANCED_FACE ( 'NONE', ( #12285 ), #5308, .T. ) ;
#12473 = CARTESIAN_POINT ( 'NONE',  ( -5.999999999999963585, -1.487416814333745711E-14, -166.4136751345948539 ) ) ;
#12474 = EDGE_LOOP ( 'NONE', ( #15679, #8740, #6992, #1045 ) ) ;
#12475 = CARTESIAN_POINT ( 'NONE',  ( 25.00000000000013500, 2.000000000000279332, -5.551115123125782702E-14 ) ) ;
#12476 =( BOUNDED_CURVE ( )  B_SPLINE_CURVE ( 2, ( #3681, #13116, #22453, #30372, #15986, #9183, #1387, #4410, #27587 ),
 .UNSPECIFIED., .F., .T. ) 
 B_SPLINE_CURVE_WITH_KNOTS ( ( 3, 2, 2, 2, 3 ),
 ( 0.6194444444444444642, 0.6203703703703703498, 0.6222222222222222321, 0.6240740740740740033, 0.6250000000000000000 ),
 .UNSPECIFIED. ) 
 CURVE ( )  GEOMETRIC_REPRESENTATION_ITEM ( )  RATIONAL_B_SPLINE_CURVE ( ( 0.9330127018922194093, 0.9330127018922234061, 1.000000000000000000, 0.8660254037844388186, 1.000000000000000000, 0.8660254037844388186, 1.000000000000000000, 0.9330127018922194093, 0.9330127018922194093 ) ) 
 REPRESENTATION_ITEM ( '' )  );
#12477 = ORIENTED_EDGE ( 'NONE', *, *, #18669, .F. ) ;
#12478 = CARTESIAN_POINT ( 'NONE',  ( 132.3750000000000284, 0.000000000000000000, 6.000000000000005329 ) ) ;
#12479 = CARTESIAN_POINT ( 'NONE',  ( 133.3273502691896510, -5.000000000000004441, 0.000000000000000000 ) ) ;
#12480 = EDGE_CURVE ( 'NONE', #1192, #15961, #2985, .T. ) ;
#12481 =( BOUNDED_CURVE ( )  B_SPLINE_CURVE ( 2, ( #21410, #25855, #14231, #23567, #343, #21258, #2502, #198, #9583 ),
 .UNSPECIFIED., .F., .T. ) 
 B_SPLINE_CURVE_WITH_KNOTS ( ( 3, 2, 2, 2, 3 ),
 ( 0.8638888888888889284, 0.8648148148148148140, 0.8666666666666666963, 0.8685185185185184675, 0.8694444444444444642 ),
 .UNSPECIFIED. ) 
 CURVE ( )  GEOMETRIC_REPRESENTATION_ITEM ( )  RATIONAL_B_SPLINE_CURVE ( ( 0.9330127018922194093, 0.9330127018922234061, 1.000000000000000000, 0.8660254037844388186, 1.000000000000000000, 0.8660254037844388186, 1.000000000000000000, 0.9330127018922154125, 0.9330127018922194093 ) ) 
 REPRESENTATION_ITEM ( '' )  );
#12482 = EDGE_CURVE ( 'NONE', #891, #14585, #562, .T. ) ;
#12483 = ORIENTED_EDGE ( 'NONE', *, *, #11942, .T. ) ;
#12484 = CARTESIAN_POINT ( 'NONE',  ( 2.775557561562891351E-14, -6.250000000000061284, -133.8169872981078186 ) ) ;
#12485 = SURFACE_SIDE_STYLE ('',( #12039 ) ) ;
#12486 = CARTESIAN_POINT ( 'NONE',  ( 6.000000000000052403, 1.607695154586625819, -175.5193375672974412 ) ) ;
#12487 = DIRECTION ( 'NONE',  ( -7.147005652999508048E-36, 5.642372883946980038E-36, 1.000000000000000000 ) ) ;
#12488 = EDGE_LOOP ( 'NONE', ( #27422, #22960, #24997 ) ) ;
#12489 = CARTESIAN_POINT ( 'NONE',  ( 14.93750000000010303, 2.000000000000151879, -0.8284271247462955401 ) ) ;
#12490 = LINE ( 'NONE', #21828, #8313 ) ;
#12491 = CARTESIAN_POINT ( 'NONE',  ( -5.999999999999956479, -1.607695154586745057, -92.26933756729744118 ) ) ;
#12492 = SURFACE_SIDE_STYLE ('',( #1070 ) ) ;
#12493 = CARTESIAN_POINT ( 'NONE',  ( 135.1726497308104058, -5.000000000000004441, 0.000000000000000000 ) ) ;
#12494 = CARTESIAN_POINT ( 'NONE',  ( 12.21132486540527040, -2.499999999999946709, -2.220446049250313081E-13 ) ) ;
#12495 = CONICAL_SURFACE ( 'NONE', #25697, 577.3502691896271699, 0.5235987755982998149 ) ;
#12496 = CARTESIAN_POINT ( 'NONE',  ( 0.000000000000000000, -5.999999999999991118, -128.5386751345948255 ) ) ;
#12497 = CARTESIAN_POINT ( 'NONE',  ( 5.999999999999949374, 1.607695154586804565, -56.09668783648702828 ) ) ;
#12498 = CARTESIAN_POINT ( 'NONE',  ( -3.464101615137757051, -5.999999999999979572, -115.1636751345948255 ) ) ;
#12499 = CARTESIAN_POINT ( 'NONE',  ( -2.775557561562891351E-14, -5.500000000000115463, -140.2500000000000000 ) ) ;
#12500 =( LENGTH_UNIT ( ) NAMED_UNIT ( * ) SI_UNIT ( .MILLI., .METRE. ) );
#12501 = VERTEX_POINT ( 'NONE', #16743 ) ;
#12502 = CARTESIAN_POINT ( 'NONE',  ( -2.775557561562891351E-14, -5.500000000000115463, -50.25000000000001421 ) ) ;
#12503 = CARTESIAN_POINT ( 'NONE',  ( 6.000000000000026645, -1.607695154586707753, -132.7306624327025872 ) ) ;
#12504 = VERTEX_POINT ( 'NONE', #2710 ) ;
#12505 = CARTESIAN_POINT ( 'NONE',  ( 119.1872167782375271, -1.849990392679562001, -0.7662911109077087390 ) ) ;
#12506 = CARTESIAN_POINT ( 'NONE',  ( 136.8750000000000284, 0.000000000000000000, 6.000000000000005329 ) ) ;
#12507 = EDGE_CURVE ( 'NONE', #765, #12660, #9345, .T. ) ;
#12508 = CARTESIAN_POINT ( 'NONE',  ( 5.412658773652739619, 3.124999999999988898, -98.81698729810783277 ) ) ;
#12509 = SURFACE_SIDE_STYLE ('',( #8002 ) ) ;
#12510 = LINE ( 'NONE', #22302, #24371 ) ;
#12511 = CARTESIAN_POINT ( 'NONE',  ( 112.3124999999997726, -1.035533905932598975, 2.500000000000265121 ) ) ;
#12512 = CARTESIAN_POINT ( 'NONE',  ( 140.1146164139961456, -11.55730820707152695, 4.524920606409397195 ) ) ;
#12513 = VECTOR ( 'NONE', #3189, 1000.000000000000000 ) ;
#12514 = ADVANCED_FACE ( 'NONE', ( #9652 ), #28508, .T. ) ;
#12515 = CARTESIAN_POINT ( 'NONE',  ( 4.763139720814407951, -2.749999999999988454, -131.0000000000000000 ) ) ;
#12516 = EDGE_CURVE ( 'NONE', #137, #13496, #21180, .T. ) ;
#12517 = ORIENTED_EDGE ( 'NONE', *, *, #1712, .T. ) ;
#12518 = ORIENTED_EDGE ( 'NONE', *, *, #19056, .F. ) ;
#12519 = CARTESIAN_POINT ( 'NONE',  ( -5.196152422706573404, -3.000000000000002665, -83.21132486540521711 ) ) ;
#12520 = CARTESIAN_POINT ( 'NONE',  ( 3.175426480543072749, -5.500000000000105693, -54.62500000000003553 ) ) ;
#12521 = CARTESIAN_POINT ( 'NONE',  ( 137.0699251345947971, 2.278174593052352925, 5.499999999999671374 ) ) ;
#12522 = CARTESIAN_POINT ( 'NONE',  ( 5.196152422706629359, -2.999999999999988898, -51.21132486540525264 ) ) ;
#12523 = CARTESIAN_POINT ( 'NONE',  ( 2.687256737965279640, 10.66819377212462960, -30.36813770228161502 ) ) ;
#12524 = CARTESIAN_POINT ( 'NONE',  ( -5.412658773652739619, 3.124999999999975131, -73.68301270189225249 ) ) ;
#12525 = CARTESIAN_POINT ( 'NONE',  ( 0.000000000000000000, 0.000000000000000000, -14.99152654425661702 ) ) ;
#12526 = CARTESIAN_POINT ( 'NONE',  ( 1101.535898384862321, 1.665334536937736830E-13, 2.220446049250315605E-13 ) ) ;
#12527 = LINE ( 'NONE', #23722, #27986 ) ;
#12528 = CARTESIAN_POINT ( 'NONE',  ( 116.3127832217621034, 1.849990392679532247, -0.7662911109075883909 ) ) ;
#12529 = CARTESIAN_POINT ( 'NONE',  ( 6.350852961086080661, -9.614813431917819062E-14, -139.8750000000000568 ) ) ;
#12530 = CARTESIAN_POINT ( 'NONE',  ( 140.0346817368759673, -9.544509217149149904, 7.273987717135122821 ) ) ;
#12531 = DIRECTION ( 'NONE',  ( 1.000000000000000000, -0.000000000000000000, -0.000000000000000000 ) ) ;
#12532 = SURFACE_STYLE_USAGE ( .BOTH. , #14822 ) ;
#12533 = CARTESIAN_POINT ( 'NONE',  ( 4.763139720814407951, -2.749999999999988454, -72.50000000000001421 ) ) ;
#12534 = CARTESIAN_POINT ( 'NONE',  ( -4.763139720814407951, -2.750000000000016431, -59.50000000000000000 ) ) ;
#12535 = EDGE_LOOP ( 'NONE', ( #12107, #9846, #3014, #28664 ) ) ;
#12536 = CARTESIAN_POINT ( 'NONE',  ( 140.9211002691896510, -4.999999999999989342, -2.071067811865468400 ) ) ;
#12537 = CARTESIAN_POINT ( 'NONE',  ( 149.4375000000000284, -4.242640687119298093, -4.242640687119298093 ) ) ;
#12538 = CARTESIAN_POINT ( 'NONE',  ( 0.000000000000000000, 5.999999999999977796, -44.99152654425658682 ) ) ;
#12539 = CARTESIAN_POINT ( 'NONE',  ( 13.68750000000000178, -0.8284271247459350507, -2.000000000000091926 ) ) ;
#12540 = ADVANCED_FACE ( 'NONE', ( #14151 ), #23489, .T. ) ;
#12541 = FACE_OUTER_BOUND ( 'NONE', #29471, .T. ) ;
#12542 = ORIENTED_EDGE ( 'NONE', *, *, #23182, .T. ) ;
#12543 = CARTESIAN_POINT ( 'NONE',  ( 141.9375000000000284, -4.242640687119298093, -4.242640687119298093 ) ) ;
#12544 = AXIS2_PLACEMENT_3D ( 'NONE', #2280, #4864, #23633 ) ;
#12545 = EDGE_CURVE ( 'NONE', #21702, #18178, #23777, .T. ) ;
#12546 = DIRECTION ( 'NONE',  ( 0.000000000000000000, 0.000000000000000000, -1.000000000000000000 ) ) ;
#12547 = CARTESIAN_POINT ( 'NONE',  ( 4.763139720814407951, -2.749999999999988454, -176.0000000000000568 ) ) ;
#12548 = CARTESIAN_POINT ( 'NONE',  ( 18.25000000000009948, 1.110223024625156540E-13, 1.999999999999946265 ) ) ;
#12549 = ORIENTED_EDGE ( 'NONE', *, *, #27826, .F. ) ;
#12550 =( NAMED_UNIT ( * ) SI_UNIT ( $, .STERADIAN. ) SOLID_ANGLE_UNIT ( ) );
#12551 = CARTESIAN_POINT ( 'NONE',  ( -2.775557561562891351E-14, -5.500000000000115463, -81.74999999999998579 ) ) ;
#12552 = ORIENTED_EDGE ( 'NONE', *, *, #21365, .F. ) ;
#12553 = AXIS2_PLACEMENT_3D ( 'NONE', #14945, #19698, #29040 ) ;
#12554 = CARTESIAN_POINT ( 'NONE',  ( 136.0000000000000284, -9.165151389911695645, -8.000000000000007105 ) ) ;
#12555 =( NAMED_UNIT ( * ) SI_UNIT ( $, .STERADIAN. ) SOLID_ANGLE_UNIT ( ) );
#12556 = CARTESIAN_POINT ( 'NONE',  ( 3.675482141847883799, -10.37335300580274300, -20.24150316489820511 ) ) ;
#12557 = CARTESIAN_POINT ( 'NONE',  ( -3.464101615137757051, -5.999999999999979572, -59.08632486540519579 ) ) ;
#12558 =( BOUNDED_CURVE ( )  B_SPLINE_CURVE ( 2, ( #10760, #8254, #5794, #15209, #24852, #13228, #3341, #12767, #1189 ),
 .UNSPECIFIED., .F., .F. ) 
 B_SPLINE_CURVE_WITH_KNOTS ( ( 3, 2, 2, 2, 3 ),
 ( 0.1861111111111111160, 0.1870370370370370294, 0.1888888888888888840, 0.1907407407407407385, 0.1916666666666666519 ),
 .UNSPECIFIED. ) 
 CURVE ( )  GEOMETRIC_REPRESENTATION_ITEM ( )  RATIONAL_B_SPLINE_CURVE ( ( 0.9330127018922194093, 0.9330127018922204085, 1.000000000000000000, 0.8660254037844388186, 1.000000000000000000, 0.8660254037844388186, 1.000000000000000000, 0.9330127018922205195, 0.9330127018922196314 ) ) 
 REPRESENTATION_ITEM ( '' )  );
#12559 = CARTESIAN_POINT ( 'NONE',  ( -6.350852961085760029, -1.281975124255709124E-13, -163.1249999999999716 ) ) ;
#12560 = CARTESIAN_POINT ( 'NONE',  ( 143.7113248654052313, 5.500000000000005329, 0.000000000000000000 ) ) ;
#12561 = CARTESIAN_POINT ( 'NONE',  ( 4.763139720814407951, -2.749999999999988454, -144.5000000000000284 ) ) ;
#12562 = CARTESIAN_POINT ( 'NONE',  ( 116.9761751345948113, -0.8284271247460250898, -1.999999999999851674 ) ) ;
#12563 = CARTESIAN_POINT ( 'NONE',  ( 149.0550748654052029, -5.500000000000012434, -2.278174593052012309 ) ) ;
#12564 = AXIS2_PLACEMENT_3D ( 'NONE', #17939, #17629, #24657 ) ;
#12565 = CARTESIAN_POINT ( 'NONE',  ( -2.775557561562891351E-14, -5.500000000000115463, -96.75000000000000000 ) ) ;
#12566 = CARTESIAN_POINT ( 'NONE',  ( 0.000000000000000000, 0.000000000000000000, 0.000000000000000000 ) ) ;
#12567 = CYLINDRICAL_SURFACE ( 'NONE', #10356, 6.000000000000000888 ) ;
#12568 = CARTESIAN_POINT ( 'NONE',  ( 4.763139720814407951, 2.750000000000002665, -78.25000000000004263 ) ) ;
#12569 = DIRECTION ( 'NONE',  ( -1.000000000000000000, 0.000000000000000000, 0.000000000000000000 ) ) ;
#12570 = FACE_OUTER_BOUND ( 'NONE', #5015, .T. ) ;
#12571 = CARTESIAN_POINT ( 'NONE',  ( 108.5000000000000000, -2.500000000000002220, 2.220446049250313081E-13 ) ) ;
#12572 = CARTESIAN_POINT ( 'NONE',  ( 1.000000000000000888, -14.99923475244191451, -9.015151515151503148 ) ) ;
#12573 = ADVANCED_FACE ( 'NONE', ( #14574 ), #7186, .T. ) ;
#12574 = SURFACE_STYLE_USAGE ( .BOTH. , #7472 ) ;
#12575 = CARTESIAN_POINT ( 'NONE',  ( 113.2113248654051034, -1.999999999999918510, 1.110223024625156540E-13 ) ) ;
#12576 = EDGE_CURVE ( 'NONE', #6031, #16041, #16597, .T. ) ;
#12577 = ORIENTED_EDGE ( 'NONE', *, *, #4283, .F. ) ;
#12578 = VECTOR ( 'NONE', #2131, 1000.000000000000000 ) ;
#12579 = CARTESIAN_POINT ( 'NONE',  ( 160.4062500000000284, 6.000000000000005329, -2.485281374238555774 ) ) ;
#12580 = CARTESIAN_POINT ( 'NONE',  ( 161.0000000000000284, -12.64911064067353408, 3.000000000000002665 ) ) ;
#12581 = CARTESIAN_POINT ( 'NONE',  ( -5.196152422706601826, 2.999999999999975131, -80.46132486540524553 ) ) ;
#12582 = ORIENTED_EDGE ( 'NONE', *, *, #30050, .T. ) ;
#12583 = ORIENTED_EDGE ( 'NONE', *, *, #7532, .T. ) ;
#12584 = ORIENTED_EDGE ( 'NONE', *, *, #16311, .T. ) ;
#12585 = AXIS2_PLACEMENT_3D ( 'NONE', #15279, #1879, #20637 ) ;
#12586 = CARTESIAN_POINT ( 'NONE',  ( 3.175426480543072749, 5.499999999999865885, -108.1250000000000284 ) ) ;
#12587 = CARTESIAN_POINT ( 'NONE',  ( -7.216878364870328078, 0.000000000000000000, -124.5580127018922241 ) ) ;
#12588 = VERTEX_POINT ( 'NONE', #28359 ) ;
#12589 = CARTESIAN_POINT ( 'NONE',  ( -5.196152422706573404, -3.000000000000002665, -68.78867513459485394 ) ) ;
#12590 = CARTESIAN_POINT ( 'NONE',  ( 3.608439182435180470, 6.249999999999982236, -163.1919872981078470 ) ) ;
#12591 = CARTESIAN_POINT ( 'NONE',  ( 10.00000000000002309, 8.326672684688674053E-14, 1.110223024625156540E-13 ) ) ;
#12592 = DIRECTION ( 'NONE',  ( 0.000000000000000000, 0.000000000000000000, -1.000000000000000000 ) ) ;
#12593 = CARTESIAN_POINT ( 'NONE',  ( 3.608439182435180470, -6.249999999999997335, -56.55801270189220986 ) ) ;
#12594 = ORIENTED_EDGE ( 'NONE', *, *, #29730, .F. ) ;
#12595 = CARTESIAN_POINT ( 'NONE',  ( -4.380587382795368967, 10.09118633559235612, -20.89546095134608805 ) ) ;
#12596 = CARTESIAN_POINT ( 'NONE',  ( 141.7425748654051745, -2.278174593052322283, -5.499999999999701572 ) ) ;
#12597 = CARTESIAN_POINT ( 'NONE',  ( 3.175426480543072749, 5.499999999999865885, -171.1250000000000000 ) ) ;
#12598 = CARTESIAN_POINT ( 'NONE',  ( 120.2499999999998721, -2.775557561562891351E-14, 2.500000000000168754 ) ) ;
#12599 =( GEOMETRIC_REPRESENTATION_CONTEXT ( 3 ) GLOBAL_UNCERTAINTY_ASSIGNED_CONTEXT ( ( #21337 ) ) GLOBAL_UNIT_ASSIGNED_CONTEXT ( ( #21194, #2584, #7353 ) ) REPRESENTATION_CONTEXT ( 'NONE', 'WORKASPACE' ) );
#12600 = CARTESIAN_POINT ( 'NONE',  ( 0.000000000000000000, 5.999999999999977796, -100.2113248654052313 ) ) ;
#12601 = CARTESIAN_POINT ( 'NONE',  ( -3.608439182435052128, -6.250000000000110134, -170.8080127018922383 ) ) ;
#12602 = CARTESIAN_POINT ( 'NONE',  ( 113.7261751345946124, -1.999999999999941602, 0.8284271247462955401 ) ) ;
#12603 = CARTESIAN_POINT ( 'NONE',  ( 23.68750000000012790, -0.8284271247461153509, -1.999999999999911626 ) ) ;
#12604 = CARTESIAN_POINT ( 'NONE',  ( 4.763139720814407951, 2.750000000000002665, -117.2500000000000142 ) ) ;
#12605 = CARTESIAN_POINT ( 'NONE',  ( -2.910268709469104432E-14, -11.00000000000000000, -14.99152654425661702 ) ) ;
#12606 = AXIS2_PLACEMENT_3D ( 'NONE', #11473, #20970, #6968 ) ;
#12607 = CARTESIAN_POINT ( 'NONE',  ( -4.763139720814407951, -2.750000000000016431, -103.0000000000000426 ) ) ;
#12608 = CARTESIAN_POINT ( 'NONE',  ( -5.999999999999944933, 1.607695154586759934, -142.4806624327026441 ) ) ;
#12609 = CARTESIAN_POINT ( 'NONE',  ( 148.6011751345948539, 3.889087296526011706, -3.889087296526011706 ) ) ;
#12610 = EDGE_LOOP ( 'NONE', ( #7965, #9656, #28962, #27295 ) ) ;
#12611 = AXIS2_PLACEMENT_3D ( 'NONE', #19168, #9640, #14713 ) ;
#12612 = CARTESIAN_POINT ( 'NONE',  ( 120.3750000000000284, -1.767766952966376426, 1.767766952966320915 ) ) ;
#12613 = DIRECTION ( 'NONE',  ( 1.000000000000000000, 0.000000000000000000, 0.000000000000000000 ) ) ;
#12614 = EDGE_CURVE ( 'NONE', #15017, #6232, #2572, .T. ) ;
#12615 = ORIENTED_EDGE ( 'NONE', *, *, #20191, .T. ) ;
#12616 = CARTESIAN_POINT ( 'NONE',  ( 3.464101615137757051, -5.999999999999979572, -126.9136751345948113 ) ) ;
#12617 = VECTOR ( 'NONE', #6785, 1000.000000000000000 ) ;
#12618 = CARTESIAN_POINT ( 'NONE',  ( 5.412658773652712085, -3.125000000000086153, -84.06698729810780435 ) ) ;
#12619 = ORIENTED_EDGE ( 'NONE', *, *, #10474, .T. ) ;
#12620 = CARTESIAN_POINT ( 'NONE',  ( 24.71589091039370700, 1.670749105717314498, -1.562495652617925446 ) ) ;
#12621 = ORIENTED_EDGE ( 'NONE', *, *, #7956, .T. ) ;
#12622 = CARTESIAN_POINT ( 'NONE',  ( 161.9062500000000568, 6.000000000000005329, -2.485281374238555774 ) ) ;
#12623 = CARTESIAN_POINT ( 'NONE',  ( 5.412658773652712085, -3.125000000000086153, -130.5669872981078470 ) ) ;
#12624 = DIRECTION ( 'NONE',  ( 0.000000000000000000, 0.000000000000000000, 1.000000000000000000 ) ) ;
#12625 = CARTESIAN_POINT ( 'NONE',  ( -9.999999999999779732, -89.00000000000001421, -4.000000000000003553 ) ) ;
#12626 = FACE_OUTER_BOUND ( 'NONE', #19717, .T. ) ;
#12627 = VERTEX_POINT ( 'NONE', #13039 ) ;
#12628 = CARTESIAN_POINT ( 'NONE',  ( 149.3511751345948255, -3.889087296526011706, 3.889087296526011706 ) ) ;
#12629 = CARTESIAN_POINT ( 'NONE',  ( 3.464101615137852974, 5.999999999999884537, -56.83632486540519579 ) ) ;
#12630 = CARTESIAN_POINT ( 'NONE',  ( 139.6726497308104342, -5.000000000000004441, 0.000000000000000000 ) ) ;
#12631 = DIRECTION ( 'NONE',  ( -1.000000000000000000, -1.665334536937731113E-16, 1.526556658859586792E-16 ) ) ;
#12632 = CARTESIAN_POINT ( 'NONE',  ( 13.91367513459485039, -1.767766952966209892, -1.767766952966487448 ) ) ;
#12633 = AXIS2_PLACEMENT_3D ( 'NONE', #26445, #25859, #5399 ) ;
#12634 = EDGE_CURVE ( 'NONE', #16367, #16120, #4078, .T. ) ;
#12635 = CARTESIAN_POINT ( 'NONE',  ( -0.5000000000000004441, -14.50000000000001243, 7.500000000000007105 ) ) ;
#12636 = CARTESIAN_POINT ( 'NONE',  ( 106.0624999999998295, 2.500000000000115019, 1.035533905933049725 ) ) ;
#12637 = CARTESIAN_POINT ( 'NONE',  ( 5.999999999999974243, 1.607695154586759934, -128.0966878364870638 ) ) ;
#12638 = CARTESIAN_POINT ( 'NONE',  ( 3.175426480543072749, 5.499999999999865885, -136.6250000000000568 ) ) ;
#12639 = CARTESIAN_POINT ( 'NONE',  ( 135.0000000000000284, 0.000000000000000000, 0.000000000000000000 ) ) ;
#12640 = CARTESIAN_POINT ( 'NONE',  ( 153.6636751345948255, 0.000000000000000000, 5.500000000000005329 ) ) ;
#12641 = PRESENTATION_LAYER_ASSIGNMENT (  '', '', ( #12176 ) ) ;
#12642 = VERTEX_POINT ( 'NONE', #7765 ) ;
#12643 = CARTESIAN_POINT ( 'NONE',  ( 13.39882486540532724, -1.035533905932629173, -2.499999999999904521 ) ) ;
#12644 = CARTESIAN_POINT ( 'NONE',  ( 4.763139720814407951, 2.750000000000002665, -49.75000000000001421 ) ) ;
#12645 = DIRECTION ( 'NONE',  ( 1.000000000000000000, 1.665334536937736783E-16, 2.220446049250315546E-16 ) ) ;
#12646 = DIRECTION ( 'NONE',  ( -1.000000000000000000, -0.000000000000000000, -0.000000000000000000 ) ) ;
#12647 =( BOUNDED_CURVE ( )  B_SPLINE_CURVE ( 2, ( #18187, #27506, #25205, #22933, #4328, #1873, #11276, #20630, #13746 ),
 .UNSPECIFIED., .F., .F. ) 
 B_SPLINE_CURVE_WITH_KNOTS ( ( 3, 2, 2, 2, 3 ),
 ( 0.1916666666666666519, 0.1925925925925925930, 0.1944444444444444475, 0.1962962962962963021, 0.1972222222222222432 ),
 .UNSPECIFIED. ) 
 CURVE ( )  GEOMETRIC_REPRESENTATION_ITEM ( )  RATIONAL_B_SPLINE_CURVE ( ( 0.9330127018922196314, 0.9330127018922185211, 1.000000000000000000, 0.8660254037844388186, 1.000000000000000000, 0.8660254037844388186, 1.000000000000000000, 0.9330127018922184101, 0.9330127018922194093 ) ) 
 REPRESENTATION_ITEM ( '' )  );
#12648 = ADVANCED_FACE ( 'NONE', ( #5912 ), #719, .T. ) ;
#12649 = ORIENTED_EDGE ( 'NONE', *, *, #21742, .F. ) ;
#12650 = CARTESIAN_POINT ( 'NONE',  ( 113.0622167782374561, -1.849990392679532247, 0.7662911109078888172 ) ) ;
#12651 = CARTESIAN_POINT ( 'NONE',  ( -5.999999999999962697, 3.323446944526963891E-14, -158.9136751345948255 ) ) ;
#12652 = CARTESIAN_POINT ( 'NONE',  ( 2.775557561562891351E-14, -6.250000000000061284, -96.31698729810783277 ) ) ;
#12653 = DIRECTION ( 'NONE',  ( 1.000000000000000000, -5.551115123125773458E-17, -1.260129944081490338E-35 ) ) ;
#12654 =( BOUNDED_CURVE ( )  B_SPLINE_CURVE ( 2, ( #16225, #28285, #14222, #6953, #18660, #7264, #25539, #20953, #2207 ),
 .UNSPECIFIED., .F., .T. ) 
 B_SPLINE_CURVE_WITH_KNOTS ( ( 3, 2, 2, 2, 3 ),
 ( 0.3374999999999998557, 0.3437499999999996114, 0.3499999999999993117, 0.3562499999999990674, 0.3624999999999989342 ),
 .UNSPECIFIED. ) 
 CURVE ( )  GEOMETRIC_REPRESENTATION_ITEM ( )  RATIONAL_B_SPLINE_CURVE ( ( 1.000000000000001998, 0.9238795325112847401, 1.000000000000000000, 0.9238795325112867385, 1.000000000000000000, 0.9238795325112867385, 1.000000000000000000, 0.9238795325113002832, 0.9999999999999864553 ) ) 
 REPRESENTATION_ITEM ( '' )  );
#12655 = CARTESIAN_POINT ( 'NONE',  ( 124.9999999999999432, -65.50000000000000000, -8.000000000000007105 ) ) ;
#12656 = CARTESIAN_POINT ( 'NONE',  ( 112.6874999999997726, -1.035533905932659149, -2.499999999999604317 ) ) ;
#12657 = AXIS2_PLACEMENT_3D ( 'NONE', #5737, #22044, #10853 ) ;
#12658 = CARTESIAN_POINT ( 'NONE',  ( 140.0769230769231228, -11.53846153846154898, 4.615384615384614087 ) ) ;
#12659 = AXIS2_PLACEMENT_3D ( 'NONE', #9418, #29990, #4493 ) ;
#12660 = VERTEX_POINT ( 'NONE', #19911 ) ;
#12661 = CARTESIAN_POINT ( 'NONE',  ( 25.37500000000009237, 2.649519052838500421, -5.551115123125782702E-14 ) ) ;
#12662 = ORIENTED_EDGE ( 'NONE', *, *, #8184, .F. ) ;
#12663 = CARTESIAN_POINT ( 'NONE',  ( 0.000000000000000000, -5.999999999999991118, -138.4613248654051745 ) ) ;
#12664 = CARTESIAN_POINT ( 'NONE',  ( -6.350852961085760029, -1.281975124255709124E-13, -61.12500000000000711 ) ) ;
#12665 = CARTESIAN_POINT ( 'NONE',  ( 5.999999999999949374, 1.607695154586804565, -69.59668783648703538 ) ) ;
#12666 = CARTESIAN_POINT ( 'NONE',  ( 14.96132486540535567, 5.551115123125782702E-14, 2.500000000000002220 ) ) ;
#12667 = CARTESIAN_POINT ( 'NONE',  ( -5.999999999999971578, 1.607695154586715303, -67.48066243270260145 ) ) ;
#12668 = CARTESIAN_POINT ( 'NONE',  ( -7.216878364870328078, 0.000000000000000000, -78.05801270189225249 ) ) ;
#12669 = CARTESIAN_POINT ( 'NONE',  ( 116.2113248654050750, -2.000000000000029310, 0.000000000000000000 ) ) ;
#12670 = CARTESIAN_POINT ( 'NONE',  ( 158.5163997308104342, 4.999999999999989342, 2.071067811865468400 ) ) ;
#12671 = VECTOR ( 'NONE', #27328, 1000.000000000000000 ) ;
#12672 = DIRECTION ( 'NONE',  ( 0.7071067811865477948, 4.734329415645503570E-17, -0.7071067811865472397 ) ) ;
#12673 = EDGE_CURVE ( 'NONE', #23965, #11212, #26072, .T. ) ;
#12674 = CARTESIAN_POINT ( 'NONE',  ( 15.00000000000000000, 2.143131898507868643E-15, -17.50000000000000355 ) ) ;
#12675 = FILL_AREA_STYLE ('',( #29053 ) ) ;
#12676 = CARTESIAN_POINT ( 'NONE',  ( 135.5000000000000000, -9.047800747817552391, 8.000000000000007105 ) ) ;
#12677 = CARTESIAN_POINT ( 'NONE',  ( 3.175426480543072749, 5.499999999999865885, -142.6250000000000000 ) ) ;
#12678 = CARTESIAN_POINT ( 'NONE',  ( 6.000000000000000888, 1.743066579297358182E-13, -87.66367513459482552 ) ) ;
#12679 = CARTESIAN_POINT ( 'NONE',  ( 2.775557561562891351E-14, 6.250000000000033751, -147.4330127018922383 ) ) ;
#12680 = CARTESIAN_POINT ( 'NONE',  ( 0.000000000000000000, 0.000000000000000000, 0.000000000000000000 ) ) ;
#12681 = DIRECTION ( 'NONE',  ( 1.000000000000000000, 0.000000000000000000, 0.000000000000000000 ) ) ;
#12683 = CARTESIAN_POINT ( 'NONE',  ( 6.350852961086080661, -9.614813431917819062E-14, -72.37500000000000000 ) ) ;
#12682 =( GEOMETRIC_REPRESENTATION_CONTEXT ( 3 ) GLOBAL_UNCERTAINTY_ASSIGNED_CONTEXT ( ( #16736 ) ) GLOBAL_UNIT_ASSIGNED_CONTEXT ( ( #21866, #21570, #25865 ) ) REPRESENTATION_CONTEXT ( 'NONE', 'WORKASPACE' ) );
#12684 = CIRCLE ( 'NONE', #4296, 2.000000000000012879 ) ;
#12685 = EDGE_CURVE ( 'NONE', #8576, #26834, #30381, .T. ) ;
#12686 = CARTESIAN_POINT ( 'NONE',  ( -4.763139720814407951, 2.749999999999946709, -58.25000000000002132 ) ) ;
#12687 = VERTEX_POINT ( 'NONE', #3154 ) ;
#12688 = CARTESIAN_POINT ( 'NONE',  ( 136.8898502691896510, 3.535533905932725318, -3.535533905932725318 ) ) ;
#12689 = CARTESIAN_POINT ( 'NONE',  ( 154.2187500000000568, 2.485281374238556218, -6.000000000000005329 ) ) ;
#12690 = CARTESIAN_POINT ( 'NONE',  ( 5.999999999999949374, 1.607695154586804565, -98.09668783648704959 ) ) ;
#12691 = CARTESIAN_POINT ( 'NONE',  ( 15.49999999999998579, -1.999999999999835243, 0.000000000000000000 ) ) ;
#12692 = CARTESIAN_POINT ( 'NONE',  ( 114.7113248654050750, 2.000000000000057288, 0.000000000000000000 ) ) ;
#12693 = CARTESIAN_POINT ( 'NONE',  ( 114.1247167782374987, -1.849990392679440321, 0.000000000000000000 ) ) ;
#12694 = ORIENTED_EDGE ( 'NONE', *, *, #2523, .T. ) ;
#12695 = CARTESIAN_POINT ( 'NONE',  ( 141.3750000000000284, 0.000000000000000000, 6.000000000000005329 ) ) ;
#12696 = CARTESIAN_POINT ( 'NONE',  ( 142.9613248654052597, -5.500000000000005329, 0.000000000000000000 ) ) ;
#12697 = AXIS2_PLACEMENT_3D ( 'NONE', #1823, #24863, #27606 ) ;
#12698 = DIRECTION ( 'NONE',  ( 1.000000000000000000, -0.000000000000000000, -0.000000000000000000 ) ) ;
#12699 = CARTESIAN_POINT ( 'NONE',  ( 0.000000000000000000, 5.499999999999991118, -177.0000000000000568 ) ) ;
#12700 = CARTESIAN_POINT ( 'NONE',  ( 16.43750000000008527, -1.999999999999851674, 0.8284271247461753029 ) ) ;
#12701 = CARTESIAN_POINT ( 'NONE',  ( 3.608439182435180470, -6.249999999999997335, -147.1919872981078470 ) ) ;
#12702 = VERTEX_POINT ( 'NONE', #19759 ) ;
#12703 = CARTESIAN_POINT ( 'NONE',  ( 3.175426480543072749, 5.499999999999865885, -82.62500000000004263 ) ) ;
#12704 = CARTESIAN_POINT ( 'NONE',  ( 3.608439182435180470, -6.249999999999997335, -92.55801270189225249 ) ) ;
#12705 = DIRECTION ( 'NONE',  ( -8.326672684688675286E-17, -2.081668171172168821E-17, 1.000000000000000000 ) ) ;
#12706 = EDGE_CURVE ( 'NONE', #22119, #12588, #17860, .T. ) ;
#12707 = SURFACE_STYLE_FILL_AREA ( #14988 ) ;
#12708 = DIRECTION ( 'NONE',  ( -1.000000000000000000, -1.734723475976843579E-16, 0.000000000000000000 ) ) ;
#12709 = CARTESIAN_POINT ( 'NONE',  ( -3.464101615137757051, -5.999999999999979572, -91.16367513459485394 ) ) ;
#12710 = LINE ( 'NONE', #22046, #18180 ) ;
#12711 = CARTESIAN_POINT ( 'NONE',  ( -4.763139720814407951, -2.750000000000016431, -161.5000000000000284 ) ) ;
#12712 = CARTESIAN_POINT ( 'NONE',  ( 6.000000000000000888, -3.330669073875464691E-16, -7.560779664488942560E-35 ) ) ;
#12713 = CARTESIAN_POINT ( 'NONE',  ( 6.350852961086080661, -9.614813431917819062E-14, -145.8750000000000284 ) ) ;
#12714 = FACE_OUTER_BOUND ( 'NONE', #23380, .T. ) ;
#12715 = CARTESIAN_POINT ( 'NONE',  ( 5.196152422706629359, -2.999999999999988898, -103.7113248654052455 ) ) ;
#12716 = CARTESIAN_POINT ( 'NONE',  ( -4.763139720814407951, -2.750000000000016431, -95.50000000000002842 ) ) ;
#12717 = CARTESIAN_POINT ( 'NONE',  ( 142.3050748654052597, 5.500000000000012434, 2.278174593052012309 ) ) ;
#12718 = FILL_AREA_STYLE_COLOUR ( '', #29962 ) ;
#12719 = EDGE_CURVE ( 'NONE', #11022, #24590, #934, .T. ) ;
#12720 = CARTESIAN_POINT ( 'NONE',  ( 4.763139720814407951, 2.750000000000002665, -82.74999999999998579 ) ) ;
#12721 = CARTESIAN_POINT ( 'NONE',  ( 135.4613248654052313, -5.500000000000005329, 0.000000000000000000 ) ) ;
#12722 = CARTESIAN_POINT ( 'NONE',  ( 151.6086002691896795, -2.071067811865468400, -4.999999999999989342 ) ) ;
#12723 = CARTESIAN_POINT ( 'NONE',  ( 139.7195358716536475, -9.255744405766421323, -7.950703011861615543 ) ) ;
#12724 = CARTESIAN_POINT ( 'NONE',  ( -5.999999999999919176, 1.607695154586804565, -155.4033121635129930 ) ) ;
#12725 = CYLINDRICAL_SURFACE ( 'NONE', #5045, 6.000000000000000888 ) ;
#12726 = CARTESIAN_POINT ( 'NONE',  ( 3.464101615137852974, 5.999999999999884537, -72.41367513459482552 ) ) ;
#12727 = CARTESIAN_POINT ( 'NONE',  ( 6.000000000000000888, -1.859271017917181981E-14, -63.66367513459483973 ) ) ;
#12728 = ORIENTED_EDGE ( 'NONE', *, *, #17846, .F. ) ;
#12729 = CARTESIAN_POINT ( 'NONE',  ( 5.196152422706629359, 3.000000000000002665, -91.46132486540525974 ) ) ;
#12730 = CARTESIAN_POINT ( 'NONE',  ( -0.04481861813794070504, -15.28417525976993652, 7.195112359326359730 ) ) ;
#12731 = CARTESIAN_POINT ( 'NONE',  ( -3.464101615137725076, 5.999999999999979572, -82.66367513459479710 ) ) ;
#12732 = CARTESIAN_POINT ( 'NONE',  ( 104.7497167782376408, 1.308140751793640533, 1.308140751793640533 ) ) ;
#12733 = CARTESIAN_POINT ( 'NONE',  ( -3.464101615137757051, -5.999999999999979572, -116.0863248654052171 ) ) ;
#12734 = VERTEX_POINT ( 'NONE', #12884 ) ;
#12735 = ORIENTED_EDGE ( 'NONE', *, *, #1467, .F. ) ;
#12736 = CARTESIAN_POINT ( 'NONE',  ( 3.175426480543072749, 5.499999999999865885, -105.1250000000000284 ) ) ;
#12737 =( BOUNDED_CURVE ( )  B_SPLINE_CURVE ( 2, ( #10346, #19707, #29052, #10197, #3552, #24447, #661, #22009, #17577 ),
 .UNSPECIFIED., .F., .T. ) 
 B_SPLINE_CURVE_WITH_KNOTS ( ( 3, 2, 2, 2, 3 ),
 ( 0.7527777777777777679, 0.7537037037037036535, 0.7555555555555555358, 0.7574074074074074181, 0.7583333333333333037 ),
 .UNSPECIFIED. ) 
 CURVE ( )  GEOMETRIC_REPRESENTATION_ITEM ( )  RATIONAL_B_SPLINE_CURVE ( ( 0.9330127018922194093, 0.9330127018922194093, 1.000000000000000000, 0.8660254037844388186, 1.000000000000000000, 0.8660254037844388186, 1.000000000000000000, 0.9330127018922234061, 0.9330127018922194093 ) ) 
 REPRESENTATION_ITEM ( '' )  );
#12738 = CARTESIAN_POINT ( 'NONE',  ( -3.608439182435052128, -6.250000000000110134, -118.3080127018922383 ) ) ;
#12739 = VERTEX_POINT ( 'NONE', #22221 ) ;
#12740 = CARTESIAN_POINT ( 'NONE',  ( 7.216878364870455975, -6.409875621278545621E-14, -163.4419872981078186 ) ) ;
#12741 = CARTESIAN_POINT ( 'NONE',  ( 105.5624999999997726, -2.499999999999874767, -1.035533905932568777 ) ) ;
#12742 = CARTESIAN_POINT ( 'NONE',  ( 21.28867513459486815, 2.500000000000002220, -1.665334536937734811E-13 ) ) ;
#12743 = EDGE_CURVE ( 'NONE', #28619, #11692, #17944, .T. ) ;
#12744 = CARTESIAN_POINT ( 'NONE',  ( 3.608439182435180470, 6.249999999999982236, -59.05801270189222407 ) ) ;
#12745 =( GEOMETRIC_REPRESENTATION_CONTEXT ( 3 ) GLOBAL_UNCERTAINTY_ASSIGNED_CONTEXT ( ( #9643 ) ) GLOBAL_UNIT_ASSIGNED_CONTEXT ( ( #14009, #14163, #20885 ) ) REPRESENTATION_CONTEXT ( 'NONE', 'WORKASPACE' ) );
#12746 = ORIENTED_EDGE ( 'NONE', *, *, #13140, .T. ) ;
#12747 = CARTESIAN_POINT ( 'NONE',  ( -0.06480180424034547026, -14.68233348625668988, -8.233331871529086854 ) ) ;
#12748 = EDGE_CURVE ( 'NONE', #18178, #29147, #9400, .T. ) ;
#12749 = CARTESIAN_POINT ( 'NONE',  ( -5.792970643771982786, 9.351264793308498469, -23.42496030963406284 ) ) ;
#12750 = CYLINDRICAL_SURFACE ( 'NONE', #5941, 6.000000000000000888 ) ;
#12751 = CARTESIAN_POINT ( 'NONE',  ( -4.763139720814407951, -2.750000000000016431, -169.0000000000000284 ) ) ;
#12752 = CARTESIAN_POINT ( 'NONE',  ( 118.7499999999997868, -1.665334536937734811E-13, -2.500000000000057732 ) ) ;
#12753 = CARTESIAN_POINT ( 'NONE',  ( -3.464101615137757051, -5.999999999999979572, -113.0863248654051745 ) ) ;
#12754 = CARTESIAN_POINT ( 'NONE',  ( -3.608439182435115633, 6.249999999999965361, -166.8080127018922951 ) ) ;
#12755 = CYLINDRICAL_SURFACE ( 'NONE', #16612, 6.000000000000000888 ) ;
#12756 = CARTESIAN_POINT ( 'NONE',  ( 24.87500000000009237, 1.414213562373312083, -1.414213562373145550 ) ) ;
#12757 = CARTESIAN_POINT ( 'NONE',  ( 4.763139720814407951, -2.749999999999988454, -112.9999999999999858 ) ) ;
#12758 = CARTESIAN_POINT ( 'NONE',  ( 4.763139720814407951, 2.750000000000002665, -106.7500000000000142 ) ) ;
#12759 = DIRECTION ( 'NONE',  ( 1.000000000000000000, -0.000000000000000000, -0.000000000000000000 ) ) ;
#12760 = CARTESIAN_POINT ( 'NONE',  ( 15.96132486540519047, 1.665334536937734811E-13, 2.500000000000057732 ) ) ;
#12761 = FACE_OUTER_BOUND ( 'NONE', #4392, .T. ) ;
#12762 = ORIENTED_EDGE ( 'NONE', *, *, #16971, .F. ) ;
#12763 = CARTESIAN_POINT ( 'NONE',  ( 14.81250000000001599, 1.097466725451679892, 2.649519052838298805 ) ) ;
#12764 = LINE ( 'NONE', #1183, #18244 ) ;
#12765 = LINE ( 'NONE', #4060, #18891 ) ;
#12766 = ORIENTED_EDGE ( 'NONE', *, *, #29373, .F. ) ;
#12767 = CARTESIAN_POINT ( 'NONE',  ( -5.999999999999957367, 1.607695154586737507, -155.9806624327026157 ) ) ;
#12768 = CARTESIAN_POINT ( 'NONE',  ( 3.608439182435180470, -6.249999999999997335, -84.19198729810781856 ) ) ;
#12769 = VECTOR ( 'NONE', #6929, 1000.000000000000000 ) ;
#12770 = DIRECTION ( 'NONE',  ( -7.147005652999508048E-36, 5.642372883946980038E-36, 1.000000000000000000 ) ) ;
#12771 = ORIENTED_EDGE ( 'NONE', *, *, #16966, .T. ) ;
#12772 = DIRECTION ( 'NONE',  ( 1.000000000000000000, -5.551115123125773458E-17, -1.260129944081490338E-35 ) ) ;
#12773 = ORIENTED_EDGE ( 'NONE', *, *, #17425, .T. ) ;
#12774 = ORIENTED_EDGE ( 'NONE', *, *, #25430, .F. ) ;
#12775 = CARTESIAN_POINT ( 'NONE',  ( 135.7648502691896510, 3.535533905932725318, 3.535533905932752852 ) ) ;
#12776 = ORIENTED_EDGE ( 'NONE', *, *, #13847, .F. ) ;
#12777 = CARTESIAN_POINT ( 'NONE',  ( -3.608439182435052128, -6.250000000000110134, -132.4419872981078470 ) ) ;
#12778 = CARTESIAN_POINT ( 'NONE',  ( 5.000000000000018652, 8.326672684688674053E-14, 1.110223024625156540E-13 ) ) ;
#12779 = CARTESIAN_POINT ( 'NONE',  ( 5.196152422706629359, 3.000000000000002665, -50.03867513459481131 ) ) ;
#12780 = VERTEX_POINT ( 'NONE', #21515 ) ;
#12781 = CARTESIAN_POINT ( 'NONE',  ( 14.06250000000011546, 2.000000000000151879, 0.8284271247461753029 ) ) ;
#12782 = CARTESIAN_POINT ( 'NONE',  ( 5.196152422706629359, 3.000000000000002665, -135.5386751345948255 ) ) ;
#12783 = CARTESIAN_POINT ( 'NONE',  ( 140.0000000000000284, -11.45643923738959202, -5.000000000000004441 ) ) ;
#12784 = ADVANCED_FACE ( 'NONE', ( #297 ), #14752, .F. ) ;
#12785 = LINE ( 'NONE', #7679, #29897 ) ;
#12786 = CARTESIAN_POINT ( 'NONE',  ( 6.000000000000000888, -1.859271017917181981E-14, -93.08632486540523132 ) ) ;
#12787 = CARTESIAN_POINT ( 'NONE',  ( -0.01452156813450973180, -14.38967195594448611, -8.359059054233915376 ) ) ;
#12788 = CARTESIAN_POINT ( 'NONE',  ( 7.216878364870455975, -6.409875621278545621E-14, -67.44198729810779014 ) ) ;
#12789 = CARTESIAN_POINT ( 'NONE',  ( 2.775557561562891351E-14, -6.250000000000061284, -51.31698729810785409 ) ) ;
#12790 =( NAMED_UNIT ( * ) SI_UNIT ( $, .STERADIAN. ) SOLID_ANGLE_UNIT ( ) );
#12791 = CARTESIAN_POINT ( 'NONE',  ( 3.464101615137757051, -5.999999999999979572, -128.4136751345948255 ) ) ;
#12792 = LINE ( 'NONE', #3672, #19517 ) ;
#12793 = CARTESIAN_POINT ( 'NONE',  ( 107.6488248654049897, 2.000000000000061728, -0.8284271247460553989 ) ) ;
#12794 = MECHANICAL_DESIGN_GEOMETRIC_PRESENTATION_REPRESENTATION (  '', ( #27467 ), #4418 ) ;
#12795 = CARTESIAN_POINT ( 'NONE',  ( 6.350852961086080661, -9.614813431917819062E-14, -132.3750000000000284 ) ) ;
#12796 = DIRECTION ( 'NONE',  ( 0.000000000000000000, 0.000000000000000000, -1.000000000000000000 ) ) ;
#12797 = CARTESIAN_POINT ( 'NONE',  ( 154.4136751345948539, 0.000000000000000000, -5.500000000000005329 ) ) ;
#12798 = ORIENTED_EDGE ( 'NONE', *, *, #10802, .T. ) ;
#12799 = CARTESIAN_POINT ( 'NONE',  ( 3.464101615137852974, 5.999999999999884537, -119.8363248654051603 ) ) ;
#12800 = LINE ( 'NONE', #17552, #28969 ) ;
#12801 = DIRECTION ( 'NONE',  ( -0.000000000000000000, -0.000000000000000000, -1.000000000000000000 ) ) ;
#12802 = EDGE_LOOP ( 'NONE', ( #19371, #21492, #11367, #24506 ) ) ;
#12803 = CARTESIAN_POINT ( 'NONE',  ( 114.6872167782375982, 1.849990392679621953, 0.7662911109080090544 ) ) ;
#12804 = DIRECTION ( 'NONE',  ( 0.000000000000000000, 0.000000000000000000, -1.000000000000000000 ) ) ;
#12805 = CARTESIAN_POINT ( 'NONE',  ( 11.12500000000010658, 1.414213562373201061, 1.414213562373034527 ) ) ;
#12806 = CARTESIAN_POINT ( 'NONE',  ( 5.412658773652712085, -3.125000000000086153, -97.56698729810780435 ) ) ;
#12807 = CARTESIAN_POINT ( 'NONE',  ( 6.000000000000000888, -1.859271017917181981E-14, -173.1636751345948539 ) ) ;
#12808 = DIRECTION ( 'NONE',  ( 1.000000000000000000, -0.000000000000000000, -0.000000000000000000 ) ) ;
#12809 = CARTESIAN_POINT ( 'NONE',  ( 115.5624999999998863, -2.499999999999934719, -1.035533905932568999 ) ) ;
#12810 = PRESENTATION_STYLE_ASSIGNMENT (( #21997 ) ) ;
#12811 = FACE_OUTER_BOUND ( 'NONE', #17230, .T. ) ;
#12812 = EDGE_CURVE ( 'NONE', #26042, #2934, #9684, .T. ) ;
#12813 = VECTOR ( 'NONE', #19152, 1000.000000000000000 ) ;
#12814 = CARTESIAN_POINT ( 'NONE',  ( 9.687499999999998224, -0.8284271247461152399, -1.999999999999971800 ) ) ;
#12815 = CARTESIAN_POINT ( 'NONE',  ( 160.7356042043084585, -11.41176159196295004, 3.718407753375058800 ) ) ;
#12816 = CARTESIAN_POINT ( 'NONE',  ( 0.000000000000000000, 5.499999999999991118, -49.49999999999998579 ) ) ;
#12817 = DIRECTION ( 'NONE',  ( 1.000000000000000000, 0.000000000000000000, 0.000000000000000000 ) ) ;
#12818 = CARTESIAN_POINT ( 'NONE',  ( -5.196152422706573404, -3.000000000000002665, -62.78867513459485394 ) ) ;
#12819 = CARTESIAN_POINT ( 'NONE',  ( 2.775557561562891351E-14, -6.250000000000061284, -73.18301270189225249 ) ) ;
#12820 = EDGE_CURVE ( 'NONE', #9948, #9152, #4754, .T. ) ;
#12821 = CARTESIAN_POINT ( 'NONE',  ( -3.464101615137757051, -5.999999999999979572, -173.0863248654051745 ) ) ;
#12822 = CARTESIAN_POINT ( 'NONE',  ( 151.0163997308104058, 4.999999999999989342, 2.071067811865468400 ) ) ;
#12823 = CARTESIAN_POINT ( 'NONE',  ( 0.000000000000000000, 0.000000000000000000, 0.000000000000000000 ) ) ;
#12824 =( NAMED_UNIT ( * ) SI_UNIT ( $, .STERADIAN. ) SOLID_ANGLE_UNIT ( ) );
#12825 =( BOUNDED_CURVE ( )  B_SPLINE_CURVE ( 2, ( #9980, #15043, #28985, #21512, #26391, #17208, #26536, #12315, #23805 ),
 .UNSPECIFIED., .F., .T. ) 
 B_SPLINE_CURVE_WITH_KNOTS ( ( 3, 2, 2, 2, 3 ),
 ( 0.3694444444444444087, 0.3703703703703703498, 0.3722222222222222321, 0.3740740740740740589, 0.3750000000000000000 ),
 .UNSPECIFIED. ) 
 CURVE ( )  GEOMETRIC_REPRESENTATION_ITEM ( )  RATIONAL_B_SPLINE_CURVE ( ( 0.9330127018922194093, 0.9330127018922174109, 1.000000000000000000, 0.8660254037844388186, 1.000000000000000000, 0.8660254037844388186, 1.000000000000000000, 0.9330127018922194093, 0.9330127018922194093 ) ) 
 REPRESENTATION_ITEM ( '' )  );
#12826 = CARTESIAN_POINT ( 'NONE',  ( 3.175426480543072749, -5.500000000000105693, -131.1250000000000284 ) ) ;
#12827 = CARTESIAN_POINT ( 'NONE',  ( 24.50000000000010658, 5.586935463532396279E-14, -2.500000000000054623 ) ) ;
#12828 = LINE ( 'NONE', #19713, #22870 ) ;
#12829 =( GEOMETRIC_REPRESENTATION_CONTEXT ( 3 ) GLOBAL_UNCERTAINTY_ASSIGNED_CONTEXT ( ( #16770 ) ) GLOBAL_UNIT_ASSIGNED_CONTEXT ( ( #4619, #172, #15898 ) ) REPRESENTATION_CONTEXT ( 'NONE', 'WORKASPACE' ) );
#12830 = CARTESIAN_POINT ( 'NONE',  ( -3.175426480542816066, -5.500000000000057732, -60.87500000000000000 ) ) ;
#12831 = CARTESIAN_POINT ( 'NONE',  ( 0.000000000000000000, 5.499999999999991118, -57.00000000000004974 ) ) ;
#12832 =( BOUNDED_CURVE ( )  B_SPLINE_CURVE ( 2, ( #16815, #640, #7547, #5386, #10023, #26719, #21845, #15093, #19548 ),
 .UNSPECIFIED., .F., .T. ) 
 B_SPLINE_CURVE_WITH_KNOTS ( ( 3, 2, 2, 2, 3 ),
 ( 0.7941176470588234837, 0.8014705882352941568, 0.8088235294117647189, 0.8161764705882352811, 0.8235294117647058432 ),
 .UNSPECIFIED. ) 
 CURVE ( )  GEOMETRIC_REPRESENTATION_ITEM ( )  RATIONAL_B_SPLINE_CURVE ( ( 1.000000000000000000, 0.9238795325112867385, 1.000000000000000000, 0.9238795325112867385, 1.000000000000000000, 0.9238795325112867385, 1.000000000000000000, 0.9238795325112867385, 1.000000000000000000 ) ) 
 REPRESENTATION_ITEM ( '' )  );
#12833 = AXIS2_PLACEMENT_3D ( 'NONE', #108, #9489, #4706 ) ;
#12834 = CARTESIAN_POINT ( 'NONE',  ( -6.000000000000000888, 1.067854986875958443E-15, 7.560779664488942560E-35 ) ) ;
#12835 = ORIENTED_EDGE ( 'NONE', *, *, #3402, .T. ) ;
#12836 = CARTESIAN_POINT ( 'NONE',  ( 153.8437500000000284, -6.000000000000005329, -2.485281374238556218 ) ) ;
#12837 = FACE_OUTER_BOUND ( 'NONE', #1228, .T. ) ;
#12838 = CARTESIAN_POINT ( 'NONE',  ( 15.00000000000012434, 2.000000000000112799, 0.000000000000000000 ) ) ;
#12839 = CARTESIAN_POINT ( 'NONE',  ( 112.2497167782374561, -1.308140751793585022, -1.308140751793640533 ) ) ;
#12840 = VERTEX_POINT ( 'NONE', #30408 ) ;
#12841 = CARTESIAN_POINT ( 'NONE',  ( 142.2187500000000284, 2.485281374238555774, -6.000000000000005329 ) ) ;
#12842 = CARTESIAN_POINT ( 'NONE',  ( 161.3705918646423925, -5.766246672886522262, -1.146283980155012205 ) ) ;
#12843 = ADVANCED_FACE ( 'NONE', ( #7064 ), #5343, .T. ) ;
#12844 = VERTEX_POINT ( 'NONE', #18769 ) ;
#12845 = EDGE_CURVE ( 'NONE', #18063, #11022, #2315, .T. ) ;
#12846 = CARTESIAN_POINT ( 'NONE',  ( 4.763139720814407951, -2.749999999999988454, -146.0000000000000284 ) ) ;
#12847 = CARTESIAN_POINT ( 'NONE',  ( 16.31250000000011369, -0.8284271247460553989, 1.999999999999971800 ) ) ;
#12848 = ORIENTED_EDGE ( 'NONE', *, *, #27785, .F. ) ;
#12849 = CARTESIAN_POINT ( 'NONE',  ( -5.412658773652739619, 3.124999999999975131, -144.8169872981078186 ) ) ;
#12850 = CARTESIAN_POINT ( 'NONE',  ( -3.175426480542816510, -5.500000000000057732, -78.87500000000002842 ) ) ;
#12851 = VECTOR ( 'NONE', #21720, 1000.000000000000000 ) ;
#12852 = CARTESIAN_POINT ( 'NONE',  ( 14.56250000000007994, 1.097466725451619718, 2.649519052838298805 ) ) ;
#12853 = EDGE_CURVE ( 'NONE', #12642, #13611, #5948, .T. ) ;
#12854 = CARTESIAN_POINT ( 'NONE',  ( -3.608439182435052128, -6.250000000000110134, -92.80801270189226670 ) ) ;
#12855 = EDGE_CURVE ( 'NONE', #5798, #17671, #25142, .T. ) ;
#12856 = CIRCLE ( 'NONE', #1040, 2.000000000000000000 ) ;
#12857 = CARTESIAN_POINT ( 'NONE',  ( 3.464101615137852974, 5.999999999999884537, -175.9136751345948539 ) ) ;
#12858 = DIRECTION ( 'NONE',  ( -1.000000000000000000, -1.665334536937736783E-16, -2.220446049250315546E-16 ) ) ;
#12859 = DIRECTION ( 'NONE',  ( 1.734723475976842100E-16, -1.000000000000000000, 0.000000000000000000 ) ) ;
#12860 = CARTESIAN_POINT ( 'NONE',  ( -5.999999999999963585, 8.134310703387671600E-14, -115.4136751345948397 ) ) ;
#12861 = CARTESIAN_POINT ( 'NONE',  ( 134.4977709871204468, -7.448582144743035371, 8.000000000000007105 ) ) ;
#12862 = FILL_AREA_STYLE_COLOUR ( '', #10957 ) ;
#12863 = CARTESIAN_POINT ( 'NONE',  ( -4.763139720814407951, 2.749999999999946709, -154.2500000000000000 ) ) ;
#12864 = CARTESIAN_POINT ( 'NONE',  ( 118.2113248654050466, -1.999999999999946265, 2.220446049250313081E-13 ) ) ;
#12865 = VECTOR ( 'NONE', #29798, 1000.000000000000000 ) ;
#12866 = CARTESIAN_POINT ( 'NONE',  ( -4.763139720814407951, -2.750000000000016431, -143.5000000000000284 ) ) ;
#12867 = CARTESIAN_POINT ( 'NONE',  ( 4.763139720814407951, 2.750000000000002665, -96.25000000000000000 ) ) ;
#12868 = FACE_OUTER_BOUND ( 'NONE', #4908, .T. ) ;
#12869 = CARTESIAN_POINT ( 'NONE',  ( 6.000000000000000888, -3.330669073875464691E-16, -7.560779664488942560E-35 ) ) ;
#12870 = CARTESIAN_POINT ( 'NONE',  ( 4.763139720814407951, 2.750000000000002665, -79.74999999999998579 ) ) ;
#12871 = CIRCLE ( 'NONE', #1054, 16.50000000000000355 ) ;
#12872 = CARTESIAN_POINT ( 'NONE',  ( 153.1086002691896510, -2.071067811865468400, -4.999999999999989342 ) ) ;
#12873 = CARTESIAN_POINT ( 'NONE',  ( -5.196152422706601826, 2.999999999999975131, -164.4613248654052029 ) ) ;
#12874 = CARTESIAN_POINT ( 'NONE',  ( 151.4136751345948539, 0.000000000000000000, -5.500000000000005329 ) ) ;
#12875 = CARTESIAN_POINT ( 'NONE',  ( 135.6636751345948255, 0.000000000000000000, 5.500000000000005329 ) ) ;
#12876 = CARTESIAN_POINT ( 'NONE',  ( 21.56250000000015987, -1.999999999999911626, -0.8284271247462354770 ) ) ;
#12877 = CARTESIAN_POINT ( 'NONE',  ( 10.46132486540518514, 5.551115123125782702E-14, -2.499999999999946709 ) ) ;
#12878 = AXIS2_PLACEMENT_3D ( 'NONE', #14313, #17200, #23793 ) ;
#12879 = DIRECTION ( 'NONE',  ( 1.000000000000000000, -0.000000000000000000, -0.000000000000000000 ) ) ;
#12880 = FACE_OUTER_BOUND ( 'NONE', #5076, .T. ) ;
#12881 = VERTEX_POINT ( 'NONE', #25949 ) ;
#12882 = CARTESIAN_POINT ( 'NONE',  ( 160.9687500000000000, -2.485281374238585972, 6.000000000000005329 ) ) ;
#12883 = CARTESIAN_POINT ( 'NONE',  ( 5.196152422706629359, 3.000000000000002665, -73.46132486540524553 ) ) ;
#12884 = CARTESIAN_POINT ( 'NONE',  ( -5.999999999999963585, 8.134310703387671600E-14, -119.9136751345948397 ) ) ;
#12885 = CARTESIAN_POINT ( 'NONE',  ( 104.2497167782374845, -1.308140751793640533, -1.308140751793640533 ) ) ;
#12886 = EDGE_CURVE ( 'NONE', #4790, #27647, #2897, .T. ) ;
#12887 = CYLINDRICAL_SURFACE ( 'NONE', #10582, 6.000000000000000888 ) ;
#12888 = ORIENTED_EDGE ( 'NONE', *, *, #12313, .T. ) ;
#12889 = AXIS2_PLACEMENT_3D ( 'NONE', #21584, #24310, #24173 ) ;
#12890 = ORIENTED_EDGE ( 'NONE', *, *, #20670, .F. ) ;
#12891 = CARTESIAN_POINT ( 'NONE',  ( 4.763139720814407951, -2.749999999999988454, -104.0000000000000426 ) ) ;
#12892 = CARTESIAN_POINT ( 'NONE',  ( 3.464101615137757051, -5.999999999999979572, -89.41367513459483973 ) ) ;
#12893 = ADVANCED_FACE ( 'NONE', ( #9533 ), #22952, .T. ) ;
#12894 = EDGE_CURVE ( 'NONE', #11685, #11657, #26099, .T. ) ;
#12895 = ORIENTED_EDGE ( 'NONE', *, *, #23697, .T. ) ;
#12896 = CARTESIAN_POINT ( 'NONE',  ( 3.464101615137852974, 5.999999999999884537, -140.8363248654051745 ) ) ;
#12897 = CARTESIAN_POINT ( 'NONE',  ( 104.9374999999997726, 2.500000000000114575, -1.035533905932448873 ) ) ;
#12898 = CARTESIAN_POINT ( 'NONE',  ( 0.000000000000000000, 5.999999999999977796, -63.28867513459479710 ) ) ;
#12899 = CARTESIAN_POINT ( 'NONE',  ( 5.412658773652712085, -3.125000000000086153, -54.93301270189221697 ) ) ;
#12900 = ORIENTED_EDGE ( 'NONE', *, *, #22570, .F. ) ;
#12901 = CARTESIAN_POINT ( 'NONE',  ( -5.999999999999944933, 1.607695154586759934, -116.9806624327026299 ) ) ;
#12902 = FACE_OUTER_BOUND ( 'NONE', #9463, .T. ) ;
#12903 = CARTESIAN_POINT ( 'NONE',  ( -6.000000000000007105, -1.607695154586655129, -62.26933756729742697 ) ) ;
#12904 = CARTESIAN_POINT ( 'NONE',  ( 0.8619745489090037127, -15.74670610583283903, -7.642883928913010827 ) ) ;
#12905 = CARTESIAN_POINT ( 'NONE',  ( -2.775557561562891351E-14, -5.500000000000115463, -167.2500000000000000 ) ) ;
#12906 = CARTESIAN_POINT ( 'NONE',  ( 120.1249999999998295, 1.767766952966348670, 1.767766952966431937 ) ) ;
#12907 = CARTESIAN_POINT ( 'NONE',  ( -5.412658773652684552, -3.125000000000099920, -169.4330127018922667 ) ) ;
#12908 = LINE ( 'NONE', #1030, #9202 ) ;
#12909 = CARTESIAN_POINT ( 'NONE',  ( -2.775557561562891351E-14, -5.500000000000115463, -116.2500000000000142 ) ) ;
#12910 = DIRECTION ( 'NONE',  ( -7.147005652999508048E-36, 5.642372883946980038E-36, 1.000000000000000000 ) ) ;
#12911 = CARTESIAN_POINT ( 'NONE',  ( -6.350852961085760029, -1.281975124255709124E-13, -106.1250000000000142 ) ) ;
#12912 = SURFACE_SIDE_STYLE ('',( #1036 ) ) ;
#12913 = CARTESIAN_POINT ( 'NONE',  ( 6.000000000000000888, 1.743066579297358182E-13, -87.08632486540520290 ) ) ;
#12914 = CARTESIAN_POINT ( 'NONE',  ( -5.999999999999963585, -1.487416814333745711E-14, -117.8363248654052313 ) ) ;
#12915 = VERTEX_POINT ( 'NONE', #14473 ) ;
#12916 = CARTESIAN_POINT ( 'NONE',  ( 13.87500000000008171, 1.665334536937734811E-13, 2.649519052838167354 ) ) ;
#12917 = DIRECTION ( 'NONE',  ( 1.000000000000000000, 0.000000000000000000, 0.000000000000000000 ) ) ;
#12918 = CARTESIAN_POINT ( 'NONE',  ( 135.0000000000000284, -6.982120021884474781, -8.500000000000007105 ) ) ;
#12919 = EDGE_LOOP ( 'NONE', ( #17289, #29628, #27932, #22868 ) ) ;
#12920 = CARTESIAN_POINT ( 'NONE',  ( -2.775557561562891351E-14, -5.500000000000115463, -159.7500000000000568 ) ) ;
#12921 = CARTESIAN_POINT ( 'NONE',  ( 109.8747167782376124, -2.775557561562891351E-14, 1.849990392679523588 ) ) ;
#12922 = CARTESIAN_POINT ( 'NONE',  ( 5.412658773652739619, 3.124999999999988898, -77.81698729810781856 ) ) ;
#12923 = EDGE_CURVE ( 'NONE', #22416, #10004, #17764, .T. ) ;
#12924 = CARTESIAN_POINT ( 'NONE',  ( -5.999999999999963585, 8.134310703387671600E-14, -129.8363248654052313 ) ) ;
#12925 = ORIENTED_EDGE ( 'NONE', *, *, #27026, .T. ) ;
#12926 = DIRECTION ( 'NONE',  ( -7.147005652999508048E-36, 5.642372883946980038E-36, 1.000000000000000000 ) ) ;
#12927 =( BOUNDED_CURVE ( )  B_SPLINE_CURVE ( 2, ( #4447, #30100, #18915, #16623, #2158, #7363, #27930, #18458, #4889 ),
 .UNSPECIFIED., .F., .F. ) 
 B_SPLINE_CURVE_WITH_KNOTS ( ( 3, 2, 2, 2, 3 ),
 ( 0.9472222222222221877, 0.9481481481481481843, 0.9499999999999999556, 0.9518518518518518379, 0.9527777777777778345 ),
 .UNSPECIFIED. ) 
 CURVE ( )  GEOMETRIC_REPRESENTATION_ITEM ( )  RATIONAL_B_SPLINE_CURVE ( ( 0.9330127018922194093, 0.9330127018922154125, 1.000000000000000000, 0.8660254037844388186, 1.000000000000000000, 0.8660254037844388186, 1.000000000000000000, 0.9330127018922154125, 0.9330127018922194093 ) ) 
 REPRESENTATION_ITEM ( '' )  );
#12928 = ORIENTED_EDGE ( 'NONE', *, *, #16238, .F. ) ;
#12929 = VERTEX_POINT ( 'NONE', #5197 ) ;
#12930 = CARTESIAN_POINT ( 'NONE',  ( 156.0000000000000284, 6.000000000000005329, 0.000000000000000000 ) ) ;
#12931 = EDGE_CURVE ( 'NONE', #16922, #5496, #12764, .T. ) ;
#12932 =( GEOMETRIC_REPRESENTATION_CONTEXT ( 3 ) GLOBAL_UNCERTAINTY_ASSIGNED_CONTEXT ( ( #28447 ) ) GLOBAL_UNIT_ASSIGNED_CONTEXT ( ( #19456, #10703, #22048 ) ) REPRESENTATION_CONTEXT ( 'NONE', 'WORKASPACE' ) );
#12933 = CARTESIAN_POINT ( 'NONE',  ( 5.412658773652712085, -3.125000000000086153, -138.9330127018922383 ) ) ;
#12934 = VERTEX_POINT ( 'NONE', #19649 ) ;
#12935 = CARTESIAN_POINT ( 'NONE',  ( 7.216878364870455975, -6.409875621278545621E-14, -124.4419872981078328 ) ) ;
#12936 = CARTESIAN_POINT ( 'NONE',  ( 6.350852961086080661, -9.614813431917819062E-14, -171.3750000000000000 ) ) ;
#12937 = CARTESIAN_POINT ( 'NONE',  ( -5.196152422706573404, -3.000000000000002665, -167.7886751345948255 ) ) ;
#12938 = CARTESIAN_POINT ( 'NONE',  ( 20.14882486540532014, -2.499999999999964473, 1.035533905932749299 ) ) ;
#12939 = ORIENTED_EDGE ( 'NONE', *, *, #28996, .T. ) ;
#12940 = CARTESIAN_POINT ( 'NONE',  ( 15.00000000000012434, 2.000000000000112799, 0.000000000000000000 ) ) ;
#12941 = DIRECTION ( 'NONE',  ( -1.000000000000000000, -1.665334536937736783E-16, -2.220446049250315546E-16 ) ) ;
#12942 = DIRECTION ( 'NONE',  ( -7.147005652999508048E-36, 5.642372883946980038E-36, 1.000000000000000000 ) ) ;
#12943 = CARTESIAN_POINT ( 'NONE',  ( 159.7528503973856857, -11.43509073697069311, -3.684568878343219112 ) ) ;
#12944 = LINE ( 'NONE', #15400, #25585 ) ;
#12945 = CARTESIAN_POINT ( 'NONE',  ( 0.07065350754911334241, -15.06982159471415805, -8.897710498417703562 ) ) ;
#12946 = CARTESIAN_POINT ( 'NONE',  ( 2.775557561562891351E-14, -6.250000000000061284, -69.31698729810781856 ) ) ;
#12947 = CARTESIAN_POINT ( 'NONE',  ( -7.216878364870328078, 0.000000000000000000, -57.69198729810781856 ) ) ;
#12948 = LINE ( 'NONE', #6596, #3398 ) ;
#12949 = CARTESIAN_POINT ( 'NONE',  ( 135.0000000000001421, 3.980162674786793975, 4.050973044690350910 ) ) ;
#12950 = CARTESIAN_POINT ( 'NONE',  ( 119.9999999999997868, 2.090674230935563926, -1.116850201269817600 ) ) ;
#12951 = DIRECTION ( 'NONE',  ( 1.000000000000000000, 1.734723475976824844E-16, -0.000000000000000000 ) ) ;
#12952 = CARTESIAN_POINT ( 'NONE',  ( -3.175426480542816510, -5.500000000000057732, -129.8750000000000284 ) ) ;
#12953 = COLOUR_RGB ( '', 0.66274510, 0.83137255, 0.94901961) ;
#12954 = ORIENTED_EDGE ( 'NONE', *, *, #18715, .T. ) ;
#12955 = CARTESIAN_POINT ( 'NONE',  ( -6.000000000000000888, 1.067854986875958443E-15, 7.560779664488942560E-35 ) ) ;
#12956 = CARTESIAN_POINT ( 'NONE',  ( 136.0000000000000284, -8.798545334315205579, 8.160000000000000142 ) ) ;
#12957 = CARTESIAN_POINT ( 'NONE',  ( 6.000000000000000888, 1.743066579297358182E-13, -97.58632486540524553 ) ) ;
#12958 = CARTESIAN_POINT ( 'NONE',  ( 6.000000000000052403, -1.607695154586662678, -99.73066243270258724 ) ) ;
#12959 = AXIS2_PLACEMENT_3D ( 'NONE', #20384, #3745, #27241 ) ;
#12960 = ORIENTED_EDGE ( 'NONE', *, *, #9360, .F. ) ;
#12961 = CARTESIAN_POINT ( 'NONE',  ( 111.8747167782376408, 0.000000000000000000, 1.849990392679523588 ) ) ;
#12962 = CARTESIAN_POINT ( 'NONE',  ( 3.464101615137852974, 5.999999999999884537, -71.83632486540520290 ) ) ;
#12963 = CARTESIAN_POINT ( 'NONE',  ( 5.412658773652712085, -3.125000000000086153, -93.06698729810780435 ) ) ;
#12964 = ADVANCED_FACE ( 'NONE', ( #17662 ), #26985, .T. ) ;
#12965 = EDGE_CURVE ( 'NONE', #14623, #1710, #12378, .T. ) ;
#12966 = CYLINDRICAL_SURFACE ( 'NONE', #16581, 17.50000000000004619 ) ;
#12967 = CARTESIAN_POINT ( 'NONE',  ( 115.9999999999998153, 2.500000000000002220, 2.220446049250313081E-13 ) ) ;
#12968 = CARTESIAN_POINT ( 'NONE',  ( 140.5828481527998974, -11.16569630559838444, 4.440052304731517019 ) ) ;
#12969 = ORIENTED_EDGE ( 'NONE', *, *, #23559, .F. ) ;
#12970 = CARTESIAN_POINT ( 'NONE',  ( 9.562500000000090594, -1.999999999999851674, -0.8284271247462354770 ) ) ;
#12971 = AXIS2_PLACEMENT_3D ( 'NONE', #26978, #27137, #1176 ) ;
#12972 = CONICAL_SURFACE ( 'NONE', #27650, 5.500000000000000000, 0.7853981633974369547 ) ;
#12973 = CARTESIAN_POINT ( 'NONE',  ( 160.5832898866354981, -11.34230189387781884, 3.922211216774294851 ) ) ;
#12974 = CARTESIAN_POINT ( 'NONE',  ( 6.350852961086080661, -9.614813431917819062E-14, -48.37500000000000711 ) ) ;
#12975 = CARTESIAN_POINT ( 'NONE',  ( 136.4136751345948539, 0.000000000000000000, -5.500000000000005329 ) ) ;
#12976 = CARTESIAN_POINT ( 'NONE',  ( 3.464101615137757051, -5.999999999999979572, -51.33632486540523843 ) ) ;
#12977 = CARTESIAN_POINT ( 'NONE',  ( 5.196152422706629359, -2.999999999999988898, -79.71132486540521711 ) ) ;
#12978 = CARTESIAN_POINT ( 'NONE',  ( -3.608439182435115633, 6.249999999999965361, -75.30801270189223828 ) ) ;
#12979 = CYLINDRICAL_SURFACE ( 'NONE', #28550, 6.000000000000000888 ) ;
#12980 = CARTESIAN_POINT ( 'NONE',  ( 150.2663997308104058, -4.999999999999989342, -2.071067811865468400 ) ) ;
#12981 = LINE ( 'NONE', #22316, #13888 ) ;
#12982 = DIRECTION ( 'NONE',  ( 0.000000000000000000, 0.000000000000000000, 1.000000000000000000 ) ) ;
#12983 = DIRECTION ( 'NONE',  ( 0.000000000000000000, 0.000000000000000000, -1.000000000000000000 ) ) ;
#12984 = SURFACE_STYLE_FILL_AREA ( #12675 ) ;
#12985 = CARTESIAN_POINT ( 'NONE',  ( -4.763139720814407951, 2.749999999999946709, -133.2500000000000284 ) ) ;
#12986 = FACE_OUTER_BOUND ( 'NONE', #6883, .T. ) ;
#12987 = CARTESIAN_POINT ( 'NONE',  ( -5.412658773652739619, 3.124999999999975131, -147.1830127018922667 ) ) ;
#12988 = FACE_OUTER_BOUND ( 'NONE', #20795, .T. ) ;
#12989 = EDGE_LOOP ( 'NONE', ( #11808, #23044, #4005, #25419 ) ) ;
#12990 = CARTESIAN_POINT ( 'NONE',  ( 4.763139720814407951, 2.750000000000002665, -61.75000000000002842 ) ) ;
#12991 = CARTESIAN_POINT ( 'NONE',  ( 0.000000000000000000, 5.499999999999991118, -58.50000000000000000 ) ) ;
#12992 = CARTESIAN_POINT ( 'NONE',  ( -3.464101615137725076, 5.999999999999979572, -170.5863248654052029 ) ) ;
#12993 = ORIENTED_EDGE ( 'NONE', *, *, #12094, .F. ) ;
#12994 = CARTESIAN_POINT ( 'NONE',  ( 148.1250000000000284, 0.000000000000000000, -6.000000000000005329 ) ) ;
#12995 = CARTESIAN_POINT ( 'NONE',  ( 0.000000000000000000, -5.999999999999991118, -118.0386751345948113 ) ) ;
#12996 = DIRECTION ( 'NONE',  ( -7.147005652999508048E-36, 5.642372883946980038E-36, 1.000000000000000000 ) ) ;
#12997 = CARTESIAN_POINT ( 'NONE',  ( 111.0622167782374845, -1.849990392679501827, 0.7662911109078888172 ) ) ;
#12998 = ADVANCED_FACE ( 'NONE', ( #24695 ), #8249, .T. ) ;
#12999 = EDGE_LOOP ( 'NONE', ( #19099, #25929, #19409, #26318 ) ) ;
#13000 = CARTESIAN_POINT ( 'NONE',  ( 147.0937500000000284, 6.000000000000005329, 2.485281374238585972 ) ) ;
#13001 = ORIENTED_EDGE ( 'NONE', *, *, #4031, .T. ) ;
#13002 = CARTESIAN_POINT ( 'NONE',  ( -2.775557561562891351E-14, -5.500000000000115463, -147.7500000000000568 ) ) ;
#13003 = CARTESIAN_POINT ( 'NONE',  ( -3.608439182435052128, -6.250000000000110134, -49.94198729810783988 ) ) ;
#13004 = CARTESIAN_POINT ( 'NONE',  ( 18.06250000000005684, 2.000000000000151879, 0.8284271247461153509 ) ) ;
#13005 = ORIENTED_EDGE ( 'NONE', *, *, #14400, .T. ) ;
#13006 = CARTESIAN_POINT ( 'NONE',  ( 2.775557561562891351E-14, -6.250000000000061284, -147.3169872981078186 ) ) ;
#13007 = CARTESIAN_POINT ( 'NONE',  ( -3.175426480542816510, 5.499999999999865885, -74.87500000000000000 ) ) ;
#13008 = CARTESIAN_POINT ( 'NONE',  ( 13.06250000000009948, -1.097466725451499370, -2.649519052838419153 ) ) ;
#13009 =( BOUNDED_SURFACE ( )  B_SPLINE_SURFACE ( 3, 2, ( 
 ( #10904, #10589, #17659 ),
 ( #19940, #29134, #1492 ),
 ( #13072, #22406, #29289 ),
 ( #8246, #26982, #5947 ),
 ( #1341, #15370, #10754 ),
 ( #8415, #17821, #3792 ),
 ( #7021, #6721, #18877 ),
 ( #4565, #23482, #2120 ),
 ( #4710, #25281, #13991 ),
 ( #28049, #21019, #2420 ) ),
 .UNSPECIFIED., .F., .F., .T. ) 
 B_SPLINE_SURFACE_WITH_KNOTS ( ( 4, 2, 2, 2, 4 ),
 ( 3, 3 ),
 ( 0.0003766318053149186927, 0.0009617798311713785311, 0.001546927857027838261, 0.002132075882884297991, 0.002717223908740757938 ),
 ( 0.000000000000000000, 1.000000000000000000 ),
 .UNSPECIFIED. ) 
 GEOMETRIC_REPRESENTATION_ITEM ( )  RATIONAL_B_SPLINE_SURFACE ( (
 ( 1.000000000000000000, 0.7071067811871951658, 1.000000000000000000),
 ( 1.000000000000000000, 0.7334558377629624148, 1.000000000000000000),
 ( 1.000000000000000000, 0.7720829478853132866, 1.000000000000000000),
 ( 1.000000000000000000, 0.8526052345356729401, 1.000000000000000000),
 ( 1.000000000000000000, 0.8923351120859769336, 1.000000000000000000),
 ( 1.000000000000000000, 0.9508075038259667933, 1.000000000000000000),
 ( 1.000000000000000000, 0.9705468812199546935, 1.000000000000000000),
 ( 1.000000000000000000, 0.9949883423647858383, 1.000000000000000000),
 ( 1.000000000000000000, 0.9999576422882877624, 1.000000000000000000),
 ( 1.000000000000000000, 1.000000000000000000, 1.000000000000000000) ) ) 
 REPRESENTATION_ITEM ( '' )  SURFACE ( )  );
#13010 = CARTESIAN_POINT ( 'NONE',  ( -3.608439182435115633, 6.249999999999965361, -97.80801270189222407 ) ) ;
#13011 = CARTESIAN_POINT ( 'NONE',  ( 2.676951800742168933E-14, -11.00000000000000000, -19.00000000000002132 ) ) ;
#13012 = CARTESIAN_POINT ( 'NONE',  ( 106.5863248654051034, 1.414213562373145550, -1.414213562373145550 ) ) ;
#13013 = CARTESIAN_POINT ( 'NONE',  ( -5.999999999999963585, 1.780251999655701777E-13, -86.91367513459485394 ) ) ;
#13014 = AXIS2_PLACEMENT_3D ( 'NONE', #13021, #22975, #6518 ) ;
#13015 = LINE ( 'NONE', #15937, #5847 ) ;
#13016 = SURFACE_STYLE_FILL_AREA ( #26774 ) ;
#13017 =( BOUNDED_CURVE ( )  B_SPLINE_CURVE ( 2, ( #10818, #27051, #5550, #6017, #3241, #21863, #944, #24443, #12669 ),
 .UNSPECIFIED., .F., .T. ) 
 B_SPLINE_CURVE_WITH_KNOTS ( ( 3, 2, 2, 2, 3 ),
 ( 0.2352941176470588203, 0.2426470588235294101, 0.2500000000000000000, 0.2573529411764705621, 0.2647058823529411797 ),
 .UNSPECIFIED. ) 
 CURVE ( )  GEOMETRIC_REPRESENTATION_ITEM ( )  RATIONAL_B_SPLINE_CURVE ( ( 1.000000000000000000, 0.9238795325112867385, 1.000000000000000000, 0.9238795325112867385, 1.000000000000000000, 0.9238795325112867385, 1.000000000000000000, 0.9238795325112867385, 1.000000000000000000 ) ) 
 REPRESENTATION_ITEM ( '' )  );
#13018 = CARTESIAN_POINT ( 'NONE',  ( 4.763139720814407951, -2.749999999999988454, -153.5000000000000284 ) ) ;
#13019 = CARTESIAN_POINT ( 'NONE',  ( 117.7113248654050466, 2.000000000000085265, 0.000000000000000000 ) ) ;
#13020 = CARTESIAN_POINT ( 'NONE',  ( 4.763139720814407951, 2.750000000000002665, -148.7500000000000568 ) ) ;
#13021 = CARTESIAN_POINT ( 'NONE',  ( 2.775557561562891351E-14, 5.874999999999977796, -46.71650635094615467 ) ) ;
#13022 = EDGE_CURVE ( 'NONE', #6076, #11685, #23318, .T. ) ;
#13023 = CARTESIAN_POINT ( 'NONE',  ( -2.775557561562891351E-14, -5.500000000000115463, -83.25000000000004263 ) ) ;
#13024 =( LENGTH_UNIT ( ) NAMED_UNIT ( * ) SI_UNIT ( .MILLI., .METRE. ) );
#13025 = CARTESIAN_POINT ( 'NONE',  ( -4.763139720814407951, -2.750000000000016431, -85.00000000000001421 ) ) ;
#13026 = CARTESIAN_POINT ( 'NONE',  ( 155.3363248654052313, 0.000000000000000000, -5.500000000000005329 ) ) ;
#13027 = CARTESIAN_POINT ( 'NONE',  ( 153.9523502691896510, 0.000000000000000000, 5.000000000000004441 ) ) ;
#13028 = CARTESIAN_POINT ( 'NONE',  ( -0.5000000000000004441, -10.50000000000000888, -7.500000000000007105 ) ) ;
#13029 = CARTESIAN_POINT ( 'NONE',  ( 152.0699251345948255, 2.278174593052229469, 5.499999999999796607 ) ) ;
#13030 = CARTESIAN_POINT ( 'NONE',  ( 144.6488248654052029, -3.889087296526011706, -3.889087296526011706 ) ) ;
#13031 = AXIS2_PLACEMENT_3D ( 'NONE', #22053, #1138, #3288 ) ;
#13032 = CARTESIAN_POINT ( 'NONE',  ( -5.999999999999904965, -1.607695154586834541, -165.7693375672973559 ) ) ;
#13033 = CARTESIAN_POINT ( 'NONE',  ( 120.3747167782374277, 0.000000000000000000, -1.849990392679301543 ) ) ;
#13034 = CARTESIAN_POINT ( 'NONE',  ( -5.999999999999963585, 1.780251999655701777E-13, -77.91367513459482552 ) ) ;
#13035 = ADVANCED_FACE ( 'NONE', ( #29137 ), #29375, .T. ) ;
#13036 = VERTEX_POINT ( 'NONE', #5553 ) ;
#13037 = PLANE ( 'NONE',  #3269 ) ;
#13038 = DIRECTION ( 'NONE',  ( 0.000000000000000000, 0.000000000000000000, -1.000000000000000000 ) ) ;
#13039 = CARTESIAN_POINT ( 'NONE',  ( -5.999999999999963585, 1.780251999655701777E-13, -53.91367513459482552 ) ) ;
#13040 = CARTESIAN_POINT ( 'NONE',  ( 116.8752832217622313, -1.849990392679579099, 0.000000000000000000 ) ) ;
#13041 = DIRECTION ( 'NONE',  ( -3.845925372767118265E-16, 1.000000000000000000, 8.881784197001258240E-16 ) ) ;
#13042 = ORIENTED_EDGE ( 'NONE', *, *, #27603, .F. ) ;
#13043 = AXIS2_PLACEMENT_3D ( 'NONE', #3844, #25042, #1554 ) ;
#13044 = UNCERTAINTY_MEASURE_WITH_UNIT (LENGTH_MEASURE( 1.000000000000000082E-05 ), #10235, 'distance_accuracy_value', 'NONE');
#13045 = ORIENTED_EDGE ( 'NONE', *, *, #13697, .T. ) ;
#13046 = CARTESIAN_POINT ( 'NONE',  ( -4.763139720814407951, 2.749999999999946709, -100.2500000000000000 ) ) ;
#13047 = CARTESIAN_POINT ( 'NONE',  ( 16.56249999999998934, 1.097466725451619718, 2.649519052838419153 ) ) ;
#13048 = FACE_OUTER_BOUND ( 'NONE', #21547, .T. ) ;
#13049 = CARTESIAN_POINT ( 'NONE',  ( 2.775557561562891351E-14, -6.250000000000061284, -115.1830127018922383 ) ) ;
#13050 = EDGE_LOOP ( 'NONE', ( #14618, #25457 ) ) ;
#13051 = DIRECTION ( 'NONE',  ( 0.000000000000000000, -1.000000000000000000, 0.000000000000000000 ) ) ;
#13052 = CARTESIAN_POINT ( 'NONE',  ( 135.0000000000000284, -7.797609721147493289, 7.985501965054816687 ) ) ;
#13053 = DIRECTION ( 'NONE',  ( 1.000000000000000000, 0.000000000000000000, -0.000000000000000000 ) ) ;
#13054 = AXIS2_PLACEMENT_3D ( 'NONE', #218, #4825, #19831 ) ;
#13055 = CARTESIAN_POINT ( 'NONE',  ( -3.608439182435052128, -6.250000000000110134, -49.30801270189224539 ) ) ;
#13056 = ORIENTED_EDGE ( 'NONE', *, *, #1895, .F. ) ;
#13057 = CARTESIAN_POINT ( 'NONE',  ( 6.000000000000000888, 7.762456499804234384E-14, -119.1636751345948113 ) ) ;
#13058 = LINE ( 'NONE', #22391, #26259 ) ;
#13059 = FACE_OUTER_BOUND ( 'NONE', #29315, .T. ) ;
#13060 = CARTESIAN_POINT ( 'NONE',  ( -4.763139720814407951, 2.749999999999946709, -173.7500000000000284 ) ) ;
#13061 =( BOUNDED_CURVE ( )  B_SPLINE_CURVE ( 2, ( #8480, #6180, #22630, #11591, #4780, #4919, #29972, #23090, #9558 ),
 .UNSPECIFIED., .F., .F. ) 
 B_SPLINE_CURVE_WITH_KNOTS ( ( 3, 2, 2, 2, 3 ),
 ( 0.5861111111111111382, 0.5870370370370370239, 0.5888888888888889062, 0.5907407407407407884, 0.5916666666666666741 ),
 .UNSPECIFIED. ) 
 CURVE ( )  GEOMETRIC_REPRESENTATION_ITEM ( )  RATIONAL_B_SPLINE_CURVE ( ( 0.9330127018922194093, 0.9330127018922234061, 1.000000000000000000, 0.8660254037844388186, 1.000000000000000000, 0.8660254037844388186, 1.000000000000000000, 0.9330127018922194093, 0.9330127018922194093 ) ) 
 REPRESENTATION_ITEM ( '' )  );
#13062 = CARTESIAN_POINT ( 'NONE',  ( 118.8124999999998579, 1.035533905932749299, -2.499999999999784173 ) ) ;
#13063 = CARTESIAN_POINT ( 'NONE',  ( -0.06529312629391929856, -14.68416511718297990, 8.236104995426456910 ) ) ;
#13064 = CARTESIAN_POINT ( 'NONE',  ( 3.608439182435180470, 6.249999999999982236, -170.0580127018922383 ) ) ;
#13065 = CARTESIAN_POINT ( 'NONE',  ( -0.5000000001309222730, -10.00000000000000888, 4.869076758059741827 ) ) ;
#13066 = EDGE_CURVE ( 'NONE', #13876, #1067, #3011, .T. ) ;
#13067 = CARTESIAN_POINT ( 'NONE',  ( 4.763139720814407951, 2.750000000000002665, -108.2500000000000142 ) ) ;
#13068 = DIRECTION ( 'NONE',  ( -7.147005652999508048E-36, 5.642372883946980038E-36, 1.000000000000000000 ) ) ;
#13069 = CARTESIAN_POINT ( 'NONE',  ( 4.763139720814407951, -2.749999999999988454, -104.0000000000000426 ) ) ;
#13070 = VECTOR ( 'NONE', #18718, 1000.000000000000000 ) ;
#13071 = CARTESIAN_POINT ( 'NONE',  ( 0.000000000000000000, 0.000000000000000000, 0.000000000000000000 ) ) ;
#13072 = CARTESIAN_POINT ( 'NONE',  ( 135.4055088883162909, -8.802581727796308542, 8.024171615095424315 ) ) ;
#13073 = VERTEX_POINT ( 'NONE', #14664 ) ;
#13074 = CARTESIAN_POINT ( 'NONE',  ( 15.37500000000013856, 1.665334536937734811E-13, -2.649519052838444910 ) ) ;
#13075 = CARTESIAN_POINT ( 'NONE',  ( 0.000000000000000000, -5.999999999999991118, -90.46132486540525974 ) ) ;
#13076 = CARTESIAN_POINT ( 'NONE',  ( 109.6877832217621318, -0.7662911109076485650, 1.849990392679652151 ) ) ;
#13077 = EDGE_CURVE ( 'NONE', #12351, #19802, #29199, .T. ) ;
#13078 = EDGE_CURVE ( 'NONE', #19519, #23669, #22318, .T. ) ;
#13079 = ORIENTED_EDGE ( 'NONE', *, *, #3218, .F. ) ;
#13080 = CARTESIAN_POINT ( 'NONE',  ( -4.763139720814407951, -2.750000000000016431, -158.5000000000000284 ) ) ;
#13081 = CARTESIAN_POINT ( 'NONE',  ( -5.999999999999919176, 1.607695154586804565, -65.40331216351300725 ) ) ;
#13082 = CARTESIAN_POINT ( 'NONE',  ( 108.7497167782375982, 1.308140751793696044, 1.308140751793640533 ) ) ;
#13083 = CARTESIAN_POINT ( 'NONE',  ( 7.216878364870455975, -6.409875621278545621E-14, -85.44198729810781856 ) ) ;
#13084 = CARTESIAN_POINT ( 'NONE',  ( 12.03867513459491789, 1.665334536937734811E-13, -2.500000000000057732 ) ) ;
#13085 = ORIENTED_EDGE ( 'NONE', *, *, #4895, .F. ) ;
#13086 = CARTESIAN_POINT ( 'NONE',  ( 24.91019988680152153, 2.044085285770432137, -0.5010375219942392322 ) ) ;
#13087 = ORIENTED_EDGE ( 'NONE', *, *, #20453, .F. ) ;
#13088 = CARTESIAN_POINT ( 'NONE',  ( 158.7187500000000000, 2.485281374238555774, -6.000000000000005329 ) ) ;
#13089 = CARTESIAN_POINT ( 'NONE',  ( 4.763139720814407951, 2.750000000000002665, -129.2500000000000284 ) ) ;
#13090 = CARTESIAN_POINT ( 'NONE',  ( 5.412658773652712085, -3.125000000000086153, -135.9330127018922383 ) ) ;
#13091 = ORIENTED_EDGE ( 'NONE', *, *, #8411, .F. ) ;
#13092 = CARTESIAN_POINT ( 'NONE',  ( -5.196152422706573404, -3.000000000000002665, -57.71132486540520290 ) ) ;
#13093 = CARTESIAN_POINT ( 'NONE',  ( 2.775557561562891351E-14, 6.250000000000033751, -125.5669872981078328 ) ) ;
#13094 = CARTESIAN_POINT ( 'NONE',  ( 4.763139720814407951, -2.749999999999988454, -170.0000000000000284 ) ) ;
#13095 = CARTESIAN_POINT ( 'NONE',  ( 159.5293203550124872, -11.10241815267761289, 4.553791194299030565 ) ) ;
#13096 = DIRECTION ( 'NONE',  ( 1.000000000000000000, -0.000000000000000000, -0.000000000000000000 ) ) ;
#13097 = ORIENTED_EDGE ( 'NONE', *, *, #5382, .T. ) ;
#13098 = DIRECTION ( 'NONE',  ( 1.734723475976824844E-16, -1.000000000000000000, 0.000000000000000000 ) ) ;
#13099 = CARTESIAN_POINT ( 'NONE',  ( 125.0000000000000568, -55.00000000000000711, -4.000000000000003553 ) ) ;
#13100 = CYLINDRICAL_SURFACE ( 'NONE', #29000, 6.000000000000000888 ) ;
#13101 = FACE_OUTER_BOUND ( 'NONE', #28358, .T. ) ;
#13102 = CARTESIAN_POINT ( 'NONE',  ( 117.2502832217622455, 1.308140751793612777, -1.308140751793307466 ) ) ;
#13103 = CARTESIAN_POINT ( 'NONE',  ( 2.775557561562891351E-14, 6.250000000000033751, -64.06698729810783277 ) ) ;
#13104 = CIRCLE ( 'NONE', #3210, 30.00000000000000355 ) ;
#13105 = CARTESIAN_POINT ( 'NONE',  ( 3.608439182435180470, 6.249999999999982236, -52.19198729810779014 ) ) ;
#13106 = CARTESIAN_POINT ( 'NONE',  ( 119.5238248654049897, 0.8284271247463257382, -1.999999999999731104 ) ) ;
#13107 = CARTESIAN_POINT ( 'NONE',  ( -5.196152422706601826, 2.999999999999975131, -55.53867513459487526 ) ) ;
#13108 = EDGE_CURVE ( 'NONE', #20574, #8576, #12737, .T. ) ;
#13109 = DIRECTION ( 'NONE',  ( 0.000000000000000000, 1.000000000000000000, -0.000000000000000000 ) ) ;
#13110 = CARTESIAN_POINT ( 'NONE',  ( -2.775557561562891351E-14, -5.500000000000115463, -131.2500000000000284 ) ) ;
#13111 = VERTEX_POINT ( 'NONE', #19420 ) ;
#13112 = CARTESIAN_POINT ( 'NONE',  ( 24.50000000000013145, 1.873492889145067508, -1.873492889145011997 ) ) ;
#13113 = DIRECTION ( 'NONE',  ( -1.734723475976806897E-15, 0.000000000000000000, 1.000000000000000000 ) ) ;
#13114 = CARTESIAN_POINT ( 'NONE',  ( -5.196152422706601826, 2.999999999999975131, -96.96132486540520290 ) ) ;
#13115 = EDGE_CURVE ( 'NONE', #8808, #1192, #12856, .T. ) ;
#13116 = CARTESIAN_POINT ( 'NONE',  ( -5.999999999999919176, 1.607695154586804565, -129.9033121635129930 ) ) ;
#13117 =( BOUNDED_CURVE ( )  B_SPLINE_CURVE ( 2, ( #18989, #510, #21730, #10055, #669, #28314, #4965, #14396, #23732 ),
 .UNSPECIFIED., .F., .T. ) 
 B_SPLINE_CURVE_WITH_KNOTS ( ( 3, 2, 2, 2, 3 ),
 ( 0.4972222222222222321, 0.4981481481481481732, 0.5000000000000000000, 0.5018518518518518823, 0.5027777777777777679 ),
 .UNSPECIFIED. ) 
 CURVE ( )  GEOMETRIC_REPRESENTATION_ITEM ( )  RATIONAL_B_SPLINE_CURVE ( ( 0.9330127018922194093, 0.9330127018922194093, 1.000000000000000000, 0.8660254037844388186, 1.000000000000000000, 0.8660254037844388186, 1.000000000000000000, 0.9330127018922194093, 0.9330127018922194093 ) ) 
 REPRESENTATION_ITEM ( '' )  );
#13118 = ORIENTED_EDGE ( 'NONE', *, *, #2889, .T. ) ;
#13119 = CARTESIAN_POINT ( 'NONE',  ( 114.1247167782374987, -1.849990392679440321, 0.000000000000000000 ) ) ;
#13120 = CARTESIAN_POINT ( 'NONE',  ( -3.608439182435052128, -6.250000000000110134, -118.9419872981078612 ) ) ;
#13121 = CARTESIAN_POINT ( 'NONE',  ( 140.0000000000000284, -11.45643923738959202, -5.000000000000004441 ) ) ;
#13122 = CARTESIAN_POINT ( 'NONE',  ( 115.2499999999998721, -5.551115123125782702E-14, 2.500000000000057732 ) ) ;
#13123 = ORIENTED_EDGE ( 'NONE', *, *, #11079, .T. ) ;
#13124 = DIRECTION ( 'NONE',  ( -7.147005652999508048E-36, 5.642372883946980038E-36, 1.000000000000000000 ) ) ;
#13125 = CARTESIAN_POINT ( 'NONE',  ( 143.3437500000000284, -6.000000000000005329, -2.485281374238555774 ) ) ;
#13126 = CARTESIAN_POINT ( 'NONE',  ( -3.464101615137757051, -5.999999999999979572, -138.5863248654051745 ) ) ;
#13127 = CARTESIAN_POINT ( 'NONE',  ( 0.000000000000000000, 5.499999999999991118, -52.49999999999999289 ) ) ;
#13128 = VECTOR ( 'NONE', #6651, 1000.000000000000000 ) ;
#13129 = CARTESIAN_POINT ( 'NONE',  ( 136.8824251345948539, 5.500000000000012434, 2.278174593052012309 ) ) ;
#13130 = CARTESIAN_POINT ( 'NONE',  ( -1.110223024625164676E-16, 2.000000000000012879, 2.021286199229734960E-15 ) ) ;
#13131 = CARTESIAN_POINT ( 'NONE',  ( 3.464101615137757051, -5.999999999999979572, -79.83632486540523132 ) ) ;
#13132 = CARTESIAN_POINT ( 'NONE',  ( -5.412658773652739619, 3.124999999999975131, -76.68301270189226670 ) ) ;
#13133 = CARTESIAN_POINT ( 'NONE',  ( 6.000000000000000888, -1.607695154586752384, -172.6533121635129930 ) ) ;
#13134 = CARTESIAN_POINT ( 'NONE',  ( 148.0163997308104058, 4.999999999999989342, 2.071067811865468400 ) ) ;
#13135 = DIRECTION ( 'NONE',  ( -7.147005652999508048E-36, 5.642372883946980038E-36, 1.000000000000000000 ) ) ;
#13136 = SURFACE_STYLE_FILL_AREA ( #29823 ) ;
#13137 = VECTOR ( 'NONE', #16196, 1000.000000000000000 ) ;
#13138 = CARTESIAN_POINT ( 'NONE',  ( 24.54902502698629618, -0.5994519693307550634, 2.381340238839862788 ) ) ;
#13139 = SURFACE_STYLE_USAGE ( .BOTH. , #29525 ) ;
#13140 = EDGE_CURVE ( 'NONE', #10034, #17588, #4959, .T. ) ;
#13141 = EDGE_CURVE ( 'NONE', #11998, #13496, #28392, .T. ) ;
#13142 = CARTESIAN_POINT ( 'NONE',  ( -6.350852961085760029, -1.281975124255709124E-13, -130.1250000000000284 ) ) ;
#13143 = CARTESIAN_POINT ( 'NONE',  ( 10.22617513459487881, 2.500000000000144773, -1.035533905932869425 ) ) ;
#13144 = AXIS2_PLACEMENT_3D ( 'NONE', #15616, #15458, #14975 ) ;
#13145 = CYLINDRICAL_SURFACE ( 'NONE', #25804, 6.000000000000000888 ) ;
#13146 = VERTEX_POINT ( 'NONE', #20007 ) ;
#13147 = CARTESIAN_POINT ( 'NONE',  ( -2.775557561562891351E-14, -5.500000000000115463, -59.25000000000002842 ) ) ;
#13148 = DIRECTION ( 'NONE',  ( 5.551115123125785167E-17, -1.000000000000000000, -8.881784197001256268E-16 ) ) ;
#13149 = CARTESIAN_POINT ( 'NONE',  ( 6.000000000000000888, 1.607695154586715303, -172.5193375672974412 ) ) ;
#13150 = CARTESIAN_POINT ( 'NONE',  ( 5.999999999999999112, 2.951592740943527306E-14, -162.6636751345948824 ) ) ;
#13151 = VERTEX_POINT ( 'NONE', #26302 ) ;
#13152 = CARTESIAN_POINT ( 'NONE',  ( 109.2499999999999147, 0.000000000000000000, 2.499999999999946709 ) ) ;
#13153 = CARTESIAN_POINT ( 'NONE',  ( 146.6250000000000284, 0.000000000000000000, -6.000000000000005329 ) ) ;
#13154 = CARTESIAN_POINT ( 'NONE',  ( 142.1324251345948539, -5.500000000000012434, -2.278174593052012309 ) ) ;
#13155 = CARTESIAN_POINT ( 'NONE',  ( 14.87500000000011013, 1.414213562373201061, -1.414213562373090038 ) ) ;
#13156 = TOROIDAL_SURFACE ( 'NONE', #10679, 16.00000000000000000, 1.000000000000000000 ) ;
#13157 = CARTESIAN_POINT ( 'NONE',  ( -3.464101615137757051, -5.999999999999979572, -49.16367513459483973 ) ) ;
#13158 = VECTOR ( 'NONE', #23558, 1000.000000000000000 ) ;
#13159 = VECTOR ( 'NONE', #30257, 1000.000000000000000 ) ;
#13160 = ORIENTED_EDGE ( 'NONE', *, *, #8303, .T. ) ;
#13161 = CARTESIAN_POINT ( 'NONE',  ( 140.5312500000000284, -2.485281374238555774, -6.000000000000005329 ) ) ;
#13162 = CARTESIAN_POINT ( 'NONE',  ( -5.999999999999963585, 1.780251999655701777E-13, -73.41367513459483973 ) ) ;
#13163 = ORIENTED_EDGE ( 'NONE', *, *, #25430, .T. ) ;
#13164 =( BOUNDED_CURVE ( )  B_SPLINE_CURVE ( 2, ( #17612, #5891, #29559, #17924, #8195, #27538, #8514, #15472, #15315 ),
 .UNSPECIFIED., .F., .F. ) 
 B_SPLINE_CURVE_WITH_KNOTS ( ( 3, 2, 2, 2, 3 ),
 ( 0.3235294117647058432, 0.3308823529411765163, 0.3382352941176470784, 0.3455882352941176405, 0.3529411764705882026 ),
 .UNSPECIFIED. ) 
 CURVE ( )  GEOMETRIC_REPRESENTATION_ITEM ( )  RATIONAL_B_SPLINE_CURVE ( ( 1.000000000000000000, 0.9238795325112867385, 1.000000000000000000, 0.9238795325112867385, 1.000000000000000000, 0.9238795325112867385, 1.000000000000000000, 0.9238795325112867385, 1.000000000000000000 ) ) 
 REPRESENTATION_ITEM ( '' )  );
#13165 = CARTESIAN_POINT ( 'NONE',  ( -6.350852961085760029, -1.281975124255709124E-13, -143.6250000000000000 ) ) ;
#13166 = ORIENTED_EDGE ( 'NONE', *, *, #21634, .F. ) ;
#13167 = CARTESIAN_POINT ( 'NONE',  ( -3.608439182435115633, 6.249999999999965361, -50.44198729810784698 ) ) ;
#13168 = CARTESIAN_POINT ( 'NONE',  ( 16.00000000000007105, 2.000000000000223821, -5.551115123125782702E-14 ) ) ;
#13169 = ORIENTED_EDGE ( 'NONE', *, *, #11414, .T. ) ;
#13170 = CARTESIAN_POINT ( 'NONE',  ( -3.175426480542816510, 5.499999999999865885, -76.37500000000001421 ) ) ;
#13171 = CARTESIAN_POINT ( 'NONE',  ( 13.31250000000003553, 2.649519052838298805, -1.097466725451559322 ) ) ;
#13172 = CARTESIAN_POINT ( 'NONE',  ( 2.775557561562891351E-14, 6.250000000000033751, -94.93301270189225249 ) ) ;
#13173 = VERTEX_POINT ( 'NONE', #5256 ) ;
#13174 = CARTESIAN_POINT ( 'NONE',  ( -5.687368478357993418, -9.417270245429932629, -26.95189157943835667 ) ) ;
#13175 = CARTESIAN_POINT ( 'NONE',  ( 3.464101615137757051, -5.999999999999979572, -83.41367513459481131 ) ) ;
#13176 = CARTESIAN_POINT ( 'NONE',  ( 140.0000000000000284, -10.00000000000000888, -7.500000000000007105 ) ) ;
#13177 = CARTESIAN_POINT ( 'NONE',  ( 135.0124395110251498, -7.358370994720393909, -8.428830671791343931 ) ) ;
#13178 = CARTESIAN_POINT ( 'NONE',  ( -6.000000000000007105, -1.607695154586655129, -65.26933756729742697 ) ) ;
#13179 = VECTOR ( 'NONE', #11611, 1000.000000000000000 ) ;
#13180 = EDGE_CURVE ( 'NONE', #8862, #13151, #3101, .T. ) ;
#13181 = CARTESIAN_POINT ( 'NONE',  ( -3.175426480542816066, -5.500000000000057732, -155.3750000000000000 ) ) ;
#13182 = CARTESIAN_POINT ( 'NONE',  ( 117.7738248654051034, 2.000000000000001776, 0.8284271247464157772 ) ) ;
#13183 = CARTESIAN_POINT ( 'NONE',  ( 6.350852961086080661, -9.614813431917819062E-14, -141.3750000000000568 ) ) ;
#13184 = DIRECTION ( 'NONE',  ( 1.000000000000000000, -5.551115123125773458E-17, -1.260129944081490338E-35 ) ) ;
#13185 = UNCERTAINTY_MEASURE_WITH_UNIT (LENGTH_MEASURE( 1.000000000000000082E-05 ), #23922, 'distance_accuracy_value', 'NONE');
#13186 = CARTESIAN_POINT ( 'NONE',  ( -4.763139720814407951, 2.749999999999946709, -88.25000000000005684 ) ) ;
#13187 =( NAMED_UNIT ( * ) PLANE_ANGLE_UNIT ( ) SI_UNIT ( $, .RADIAN. ) );
#13188 = CARTESIAN_POINT ( 'NONE',  ( 4.763139720814407951, -2.749999999999988454, -81.50000000000001421 ) ) ;
#13189 = DIRECTION ( 'NONE',  ( -1.000000000000000000, -0.000000000000000000, -0.000000000000000000 ) ) ;
#13190 = DIRECTION ( 'NONE',  ( -1.000000000000000000, -1.665334536937736783E-16, -2.220446049250315546E-16 ) ) ;
#13191 = CARTESIAN_POINT ( 'NONE',  ( 22.50000000000010303, -1.999999999999835243, 0.000000000000000000 ) ) ;
#13192 = CARTESIAN_POINT ( 'NONE',  ( 10.96132486540515849, 1.110223024625156540E-13, 2.499999999999835687 ) ) ;
#13193 = DIRECTION ( 'NONE',  ( -7.147005652999508048E-36, 5.642372883946980038E-36, 1.000000000000000000 ) ) ;
#13194 = VERTEX_POINT ( 'NONE', #19564 ) ;
#13195 = CARTESIAN_POINT ( 'NONE',  ( 162.0000000000000284, 6.000000000000005329, 0.000000000000000000 ) ) ;
#13196 = CARTESIAN_POINT ( 'NONE',  ( -0.5000000000000004441, -14.50000000000001243, 7.500000000000007105 ) ) ;
#13197 = CARTESIAN_POINT ( 'NONE',  ( 5.196152422706629359, -2.999999999999988898, -171.7886751345948255 ) ) ;
#13198 = CARTESIAN_POINT ( 'NONE',  ( 117.2502832217622455, 1.308140751793612777, -1.308140751793307466 ) ) ;
#13199 = LINE ( 'NONE', #20686, #25884 ) ;
#13200 = ORIENTED_EDGE ( 'NONE', *, *, #27470, .F. ) ;
#13201 =( BOUNDED_CURVE ( )  B_SPLINE_CURVE ( 2, ( #28640, #994, #17468, #19748, #17323, #7611, #26639, #16881, #14855 ),
 .UNSPECIFIED., .F., .T. ) 
 B_SPLINE_CURVE_WITH_KNOTS ( ( 3, 2, 2, 2, 3 ),
 ( 0.1916666666666666519, 0.1925925925925925375, 0.1944444444444444198, 0.1962962962962963021, 0.1972222222222222987 ),
 .UNSPECIFIED. ) 
 CURVE ( )  GEOMETRIC_REPRESENTATION_ITEM ( )  RATIONAL_B_SPLINE_CURVE ( ( 0.9330127018922194093, 0.9330127018922194093, 1.000000000000000000, 0.8660254037844388186, 1.000000000000000000, 0.8660254037844388186, 1.000000000000000000, 0.9330127018922154125, 0.9330127018922194093 ) ) 
 REPRESENTATION_ITEM ( '' )  );
#13202 = ORIENTED_EDGE ( 'NONE', *, *, #18843, .T. ) ;
#13203 = EDGE_CURVE ( 'NONE', #11924, #16705, #19020, .T. ) ;
#13204 = CARTESIAN_POINT ( 'NONE',  ( -3.175426480542816510, 5.499999999999865885, -94.37500000000002842 ) ) ;
#13205 = DIRECTION ( 'NONE',  ( 1.000000000000000000, -5.551115123125773458E-17, -1.260129944081490338E-35 ) ) ;
#13206 = CARTESIAN_POINT ( 'NONE',  ( 5.412658773652712085, -3.125000000000086153, -116.4330127018922099 ) ) ;
#13207 =( BOUNDED_CURVE ( )  B_SPLINE_CURVE ( 2, ( #4295, #20433, #20591, #25479, #27466, #13871, #4137, #16326, #23055 ),
 .UNSPECIFIED., .F., .T. ) 
 B_SPLINE_CURVE_WITH_KNOTS ( ( 3, 2, 2, 2, 3 ),
 ( 0.9916666666666665853, 0.9925925925925925819, 0.9944444444444444642, 0.9962962962962963465, 0.9972222222222222321 ),
 .UNSPECIFIED. ) 
 CURVE ( )  GEOMETRIC_REPRESENTATION_ITEM ( )  RATIONAL_B_SPLINE_CURVE ( ( 0.9330127018922194093, 0.9330127018922154125, 1.000000000000000000, 0.8660254037844388186, 1.000000000000000000, 0.8660254037844388186, 1.000000000000000000, 0.9330127018922194093, 0.9330127018922194093 ) ) 
 REPRESENTATION_ITEM ( '' )  );
#13208 = ORIENTED_EDGE ( 'NONE', *, *, #4974, .F. ) ;
#13209 = CARTESIAN_POINT ( 'NONE',  ( 0.8631338372297875372, -14.49999999999998579, -7.874007874011823560 ) ) ;
#13210 = CARTESIAN_POINT ( 'NONE',  ( 7.216878364870455975, -6.409875621278545621E-14, -51.80801270189225960 ) ) ;
#13211 = ORIENTED_EDGE ( 'NONE', *, *, #1587, .F. ) ;
#13212 = FILL_AREA_STYLE_COLOUR ( '', #140 ) ;
#13213 = EDGE_CURVE ( 'NONE', #5395, #19802, #22136, .T. ) ;
#13214 = CARTESIAN_POINT ( 'NONE',  ( 146.3511751345948255, -3.889087296526011706, 3.889087296526011706 ) ) ;
#13215 = DIRECTION ( 'NONE',  ( -1.000000000000000000, -1.665334536937736783E-16, -2.220446049250315546E-16 ) ) ;
#13216 = CARTESIAN_POINT ( 'NONE',  ( -6.350852961085760029, -1.281975124255709124E-13, -173.6250000000000284 ) ) ;
#13217 = CARTESIAN_POINT ( 'NONE',  ( 116.6249999999999716, -1.767766952966459693, -1.767766952966209892 ) ) ;
#13218 = CARTESIAN_POINT ( 'NONE',  ( 5.196152422706629359, 3.000000000000002665, -107.9613248654052171 ) ) ;
#13219 = CARTESIAN_POINT ( 'NONE',  ( 6.000000000000000888, 1.743066579297358182E-13, -87.08632486540520290 ) ) ;
#13220 = CARTESIAN_POINT ( 'NONE',  ( 135.0000000000000284, 0.000000000000000000, 0.000000000000000000 ) ) ;
#13221 = CARTESIAN_POINT ( 'NONE',  ( 3.175426480543072749, 5.499999999999865885, -108.1250000000000284 ) ) ;
#13222 = CARTESIAN_POINT ( 'NONE',  ( 5.196152422706629359, 3.000000000000002665, -162.5386751345948539 ) ) ;
#13223 = CARTESIAN_POINT ( 'NONE',  ( 6.000000000000052403, -1.607695154586662678, -81.73066243270260145 ) ) ;
#13224 = EDGE_LOOP ( 'NONE', ( #4576, #30349, #21010, #6043 ) ) ;
#13225 = CARTESIAN_POINT ( 'NONE',  ( 116.2499999999998437, 5.551115123125782702E-14, 2.500000000000168754 ) ) ;
#13226 = CARTESIAN_POINT ( 'NONE',  ( 110.1877832217620750, 0.7662911109078588412, -1.849990392679411677 ) ) ;
#13227 = ORIENTED_EDGE ( 'NONE', *, *, #12634, .T. ) ;
#13228 = CARTESIAN_POINT ( 'NONE',  ( -3.464101615137725076, 5.999999999999979572, -156.1636751345947687 ) ) ;
#13229 = CARTESIAN_POINT ( 'NONE',  ( -3.608439182435052128, -6.250000000000110134, -78.44198729810779014 ) ) ;
#13230 = LINE ( 'NONE', #4109, #25379 ) ;
#13231 = ORIENTED_EDGE ( 'NONE', *, *, #5752, .F. ) ;
#13232 = CARTESIAN_POINT ( 'NONE',  ( -5.999999999999956479, -1.607695154586745057, -75.76933756729744118 ) ) ;
#13233 = VERTEX_POINT ( 'NONE', #23092 ) ;
#13234 = VERTEX_POINT ( 'NONE', #6021 ) ;
#13235 = CARTESIAN_POINT ( 'NONE',  ( 154.3125000000000284, 4.242640687119298093, -4.242640687119298093 ) ) ;
#13236 = EDGE_CURVE ( 'NONE', #18697, #15961, #23156, .T. ) ;
#13237 = CARTESIAN_POINT ( 'NONE',  ( 4.763139720814407951, -2.749999999999988454, -125.0000000000000000 ) ) ;
#13238 = CARTESIAN_POINT ( 'NONE',  ( -5.412658773652684552, -3.125000000000099920, -137.9330127018922383 ) ) ;
#13239 = ORIENTED_EDGE ( 'NONE', *, *, #4003, .T. ) ;
#13240 = CARTESIAN_POINT ( 'NONE',  ( 5.999999999999949374, 1.607695154586804565, -57.59668783648704249 ) ) ;
#13241 = CARTESIAN_POINT ( 'NONE',  ( 7.216878364870455975, -6.409875621278545621E-14, -121.4419872981078043 ) ) ;
#13242 = CARTESIAN_POINT ( 'NONE',  ( -5.412658773652684552, -3.125000000000099920, -179.0669872981078186 ) ) ;
#13243 = CARTESIAN_POINT ( 'NONE',  ( -3.175426480542816510, 5.499999999999865885, -172.3750000000000000 ) ) ;
#13244 = FACE_OUTER_BOUND ( 'NONE', #15929, .T. ) ;
#13245 = SURFACE_SIDE_STYLE ('',( #17845 ) ) ;
#13246 = VERTEX_POINT ( 'NONE', #24766 ) ;
#13247 = CARTESIAN_POINT ( 'NONE',  ( 12.43750000000010836, -1.999999999999851674, 0.8284271247462955401 ) ) ;
#13248 = DIRECTION ( 'NONE',  ( 0.000000000000000000, 0.000000000000000000, -1.000000000000000000 ) ) ;
#13249 = EDGE_CURVE ( 'NONE', #7272, #14299, #15749, .T. ) ;
#13250 = CARTESIAN_POINT ( 'NONE',  ( 0.000000000000000000, 5.999999999999977796, -148.2113248654052313 ) ) ;
#13251 = FACE_OUTER_BOUND ( 'NONE', #17956, .T. ) ;
#13252 = CARTESIAN_POINT ( 'NONE',  ( -19.99999999999998224, -25.00000000000010658, 8.000000000000007105 ) ) ;
#13253 = CARTESIAN_POINT ( 'NONE',  ( 113.1252832217622029, -1.110223024625156540E-13, -1.849990392679523588 ) ) ;
#13254 = CARTESIAN_POINT ( 'NONE',  ( 5.412658773652712085, -3.125000000000086153, -67.56698729810783277 ) ) ;
#13255 = CARTESIAN_POINT ( 'NONE',  ( 2.775557561562891351E-14, -6.250000000000061284, -55.81698729810780435 ) ) ;
#13256 = CARTESIAN_POINT ( 'NONE',  ( 119.2738248654049471, -1.999999999999941602, -0.8284271247459952248 ) ) ;
#13257 = CARTESIAN_POINT ( 'NONE',  ( -3.175426480542816510, -5.500000000000057732, -47.37500000000000000 ) ) ;
#13258 = CARTESIAN_POINT ( 'NONE',  ( -3.464101615137725076, 5.999999999999979572, -55.66367513459481131 ) ) ;
#13259 = CARTESIAN_POINT ( 'NONE',  ( -2.775557561562891351E-14, -5.500000000000115463, -129.7500000000000284 ) ) ;
#13260 = CARTESIAN_POINT ( 'NONE',  ( 6.000000000000000888, -1.859271017917181981E-14, -115.5863248654052171 ) ) ;
#13261 = VERTEX_POINT ( 'NONE', #1413 ) ;
#13262 = CARTESIAN_POINT ( 'NONE',  ( 23.62500000000011724, 2.649519052838500421, -5.551115123125782702E-14 ) ) ;
#13263 = VECTOR ( 'NONE', #11542, 1000.000000000000000 ) ;
#13264 = CYLINDRICAL_SURFACE ( 'NONE', #9190, 2.000000000000012879 ) ;
#13265 = CARTESIAN_POINT ( 'NONE',  ( 3.464101615137852974, 5.999999999999884537, -97.33632486540517448 ) ) ;
#13266 = CARTESIAN_POINT ( 'NONE',  ( 140.3586002691896226, 2.071067811865468400, 4.999999999999989342 ) ) ;
#13267 = ORIENTED_EDGE ( 'NONE', *, *, #8979, .F. ) ;
#13268 = CARTESIAN_POINT ( 'NONE',  ( 113.2497167782375982, -1.308140751793585022, -1.308140751793640533 ) ) ;
#13269 = CARTESIAN_POINT ( 'NONE',  ( 15.08632486540523132, -1.767766952966265404, 1.767766952966376426 ) ) ;
#13270 = CARTESIAN_POINT ( 'NONE',  ( 3.608439182435180470, -6.249999999999997335, -118.6919872981078612 ) ) ;
#13271 = CARTESIAN_POINT ( 'NONE',  ( 135.0000000000000284, 3.279024082124037065, -4.561124296770755038 ) ) ;
#13272 = FACE_OUTER_BOUND ( 'NONE', #5089, .T. ) ;
#13273 = ORIENTED_EDGE ( 'NONE', *, *, #22012, .T. ) ;
#13274 = CARTESIAN_POINT ( 'NONE',  ( 159.3477600650482486, -12.04942537661511714, 3.940026486796909477 ) ) ;
#13275 = CARTESIAN_POINT ( 'NONE',  ( 144.6562500000000568, -6.000000000000005329, 2.485281374238555774 ) ) ;
#13276 = ADVANCED_FACE ( 'NONE', ( #29524 ), #13593, .T. ) ;
#13277 = VERTEX_POINT ( 'NONE', #24909 ) ;
#13278 = SURFACE_STYLE_FILL_AREA ( #3848 ) ;
#13279 = CARTESIAN_POINT ( 'NONE',  ( 4.763139720814407951, -2.749999999999988454, -53.00000000000004974 ) ) ;
#13280 = AXIS2_PLACEMENT_3D ( 'NONE', #28705, #14918, #905 ) ;
#13281 = CARTESIAN_POINT ( 'NONE',  ( 20.93750000000008171, 2.000000000000212275, -0.8284271247463557142 ) ) ;
#13282 = FACE_OUTER_BOUND ( 'NONE', #16753, .T. ) ;
#13283 = ADVANCED_FACE ( 'NONE', ( #6182 ), #10975, .T. ) ;
#13284 = CARTESIAN_POINT ( 'NONE',  ( -1.000000000000000888, 11.00000000000001066, -3.000000000000002665 ) ) ;
#13285 = CARTESIAN_POINT ( 'NONE',  ( 2.775557561562891351E-14, 6.250000000000033751, -69.43301270189222407 ) ) ;
#13286 = ADVANCED_FACE ( 'NONE', ( #8639 ), #18042, .T. ) ;
#13287 =( GEOMETRIC_REPRESENTATION_CONTEXT ( 3 ) GLOBAL_UNCERTAINTY_ASSIGNED_CONTEXT ( ( #1452 ) ) GLOBAL_UNIT_ASSIGNED_CONTEXT ( ( #15146, #26475, #12555 ) ) REPRESENTATION_CONTEXT ( 'NONE', 'WORKASPACE' ) );
#13288 = CARTESIAN_POINT ( 'NONE',  ( 147.1726497308104058, -5.000000000000004441, 0.000000000000000000 ) ) ;
#13289 = CARTESIAN_POINT ( 'NONE',  ( 6.000000000000007105, -1.607695154586741060, -177.7306624327026157 ) ) ;
#13290 = PRESENTATION_LAYER_ASSIGNMENT (  '', '', ( #9330 ) ) ;
#13291 = CARTESIAN_POINT ( 'NONE',  ( -6.000000000000007105, -1.607695154586655129, -94.34668783648703538 ) ) ;
#13292 =( BOUNDED_CURVE ( )  B_SPLINE_CURVE ( 2, ( #17519, #15686, #3496, #3646, #8103, #18126, #8426, #27441, #13376 ),
 .UNSPECIFIED., .F., .T. ) 
 B_SPLINE_CURVE_WITH_KNOTS ( ( 3, 2, 2, 2, 3 ),
 ( 0.6250000000000000000, 0.6259259259259258856, 0.6277777777777777679, 0.6296296296296296502, 0.6305555555555556468 ),
 .UNSPECIFIED. ) 
 CURVE ( )  GEOMETRIC_REPRESENTATION_ITEM ( )  RATIONAL_B_SPLINE_CURVE ( ( 0.9330127018922194093, 0.9330127018922194093, 1.000000000000000000, 0.8660254037844388186, 1.000000000000000000, 0.8660254037844388186, 1.000000000000000000, 0.9330127018922154125, 0.9330127018922194093 ) ) 
 REPRESENTATION_ITEM ( '' )  );
#13293 = CARTESIAN_POINT ( 'NONE',  ( 3.175426480543072749, 5.499999999999865885, -130.6250000000000284 ) ) ;
#13294 = ORIENTED_EDGE ( 'NONE', *, *, #23855, .F. ) ;
#13295 = CARTESIAN_POINT ( 'NONE',  ( -2.775557561562891351E-14, -5.500000000000115463, -66.75000000000002842 ) ) ;
#13296 = DIRECTION ( 'NONE',  ( -7.147005652999508048E-36, 5.642372883946980038E-36, 1.000000000000000000 ) ) ;
#13297 = SURFACE_STYLE_USAGE ( .BOTH. , #27216 ) ;
#13298 = ORIENTED_EDGE ( 'NONE', *, *, #20033, .T. ) ;
#13299 = CARTESIAN_POINT ( 'NONE',  ( 108.6874999999998010, -1.035533905932749299, -2.499999999999844569 ) ) ;
#13300 = CARTESIAN_POINT ( 'NONE',  ( 146.4375000000000284, -4.242640687119298093, -4.242640687119298093 ) ) ;
#13301 = DIRECTION ( 'NONE',  ( -1.000000000000000000, -1.665334536937736783E-16, -2.220446049250315546E-16 ) ) ;
#13302 = CARTESIAN_POINT ( 'NONE',  ( 13.31250000000012612, -0.8284271247460552878, 1.999999999999911626 ) ) ;
#13303 = CIRCLE ( 'NONE', #22077, 1.000000000000000000 ) ;
#13304 = CARTESIAN_POINT ( 'NONE',  ( 6.000000000000000888, 1.743066579297358182E-13, -48.66367513459482552 ) ) ;
#13305 = ORIENTED_EDGE ( 'NONE', *, *, #8979, .T. ) ;
#13306 = AXIS2_PLACEMENT_3D ( 'NONE', #2071, #27845, #11472 ) ;
#13307 = CARTESIAN_POINT ( 'NONE',  ( 141.1875000000000284, 4.242640687119269671, 4.242640687119298093 ) ) ;
#13308 = CARTESIAN_POINT ( 'NONE',  ( -3.464101615137757051, -5.999999999999979572, -122.0863248654051745 ) ) ;
#13309 = ORIENTED_EDGE ( 'NONE', *, *, #20609, .T. ) ;
#13310 = ADVANCED_FACE ( 'NONE', ( #6485 ), #25359, .F. ) ;
#13311 = ADVANCED_FACE ( 'NONE', ( #11441 ), #6638, .F. ) ;
#13312 = CARTESIAN_POINT ( 'NONE',  ( -3.175426480542816510, -5.500000000000057732, -144.8750000000000853 ) ) ;
#13313 = CARTESIAN_POINT ( 'NONE',  ( 12.25000000000006573, 5.551115123125782702E-14, 1.999999999999946265 ) ) ;
#13314 = ORIENTED_EDGE ( 'NONE', *, *, #20609, .F. ) ;
#13315 = CARTESIAN_POINT ( 'NONE',  ( 3.175426480543072749, -5.500000000000105693, -69.62500000000004263 ) ) ;
#13316 = CARTESIAN_POINT ( 'NONE',  ( 14.37500000000016520, 2.649519052838611444, -5.551115123125782702E-14 ) ) ;
#13317 = CARTESIAN_POINT ( 'NONE',  ( 5.412658773652712085, -3.125000000000086153, -96.93301270189225249 ) ) ;
#13318 = DIRECTION ( 'NONE',  ( 1.000000000000000000, 0.000000000000000000, 0.000000000000000000 ) ) ;
#13319 = CARTESIAN_POINT ( 'NONE',  ( -5.999999999999968026, -1.607695154586722186, -151.3466878364870354 ) ) ;
#13320 = CARTESIAN_POINT ( 'NONE',  ( 3.330669073875470114E-16, -5.999999999999999112, -5.329070518200752183E-15 ) ) ;
#13321 = CARTESIAN_POINT ( 'NONE',  ( -5.196152422706573404, -3.000000000000002665, -65.21132486540520290 ) ) ;
#13322 = APPLICATION_PROTOCOL_DEFINITION ( 'draft international standard', 'automotive_design', 1998, #13648 ) ;
#13323 = CIRCLE ( 'NONE', #26508, 4.000000000000006217 ) ;
#13324 = CARTESIAN_POINT ( 'NONE',  ( -4.763139720814407951, 2.749999999999946709, -152.7500000000000568 ) ) ;
#13325 = DIRECTION ( 'NONE',  ( -7.147005652999508048E-36, 5.642372883946980038E-36, 1.000000000000000000 ) ) ;
#13326 = CARTESIAN_POINT ( 'NONE',  ( -5.511802646642890657, 2.338480655328711855, -180.0000000000001137 ) ) ;
#13327 = CARTESIAN_POINT ( 'NONE',  ( -2.775557561562891351E-14, -5.500000000000115463, -89.25000000000005684 ) ) ;
#13328 = CARTESIAN_POINT ( 'NONE',  ( 104.1872167782373708, -1.849990392679351725, -0.7662911109074683758 ) ) ;
#13329 = FILL_AREA_STYLE_COLOUR ( '', #1217 ) ;
#13330 = CARTESIAN_POINT ( 'NONE',  ( -4.763139720814407951, 2.749999999999946709, -71.75000000000004263 ) ) ;
#13331 = CIRCLE ( 'NONE', #25545, 0.5000000000000004441 ) ;
#13332 = CARTESIAN_POINT ( 'NONE',  ( 3.464101615137757051, -5.999999999999979572, -120.3363248654051461 ) ) ;
#13333 = CARTESIAN_POINT ( 'NONE',  ( -3.464101615137725076, 5.999999999999979572, -142.0863248654052029 ) ) ;
#13334 = LINE ( 'NONE', #29715, #29488 ) ;
#13335 =( BOUNDED_CURVE ( )  B_SPLINE_CURVE ( 2, ( #28311, #7289, #16692, #23730, #12086, #21425, #19279, #5710, #5263 ),
 .UNSPECIFIED., .F., .F. ) 
 B_SPLINE_CURVE_WITH_KNOTS ( ( 3, 2, 2, 2, 3 ),
 ( 0.8027777777777777013, 0.8037037037037036979, 0.8055555555555555802, 0.8074074074074074625, 0.8083333333333333481 ),
 .UNSPECIFIED. ) 
 CURVE ( )  GEOMETRIC_REPRESENTATION_ITEM ( )  RATIONAL_B_SPLINE_CURVE ( ( 0.9330127018922194093, 0.9330127018922154125, 1.000000000000000000, 0.8660254037844388186, 1.000000000000000000, 0.8660254037844388186, 1.000000000000000000, 0.9330127018922194093, 0.9330127018922194093 ) ) 
 REPRESENTATION_ITEM ( '' )  );
#13336 = CARTESIAN_POINT ( 'NONE',  ( 6.055081547227420202, 3.114577045054877854E-15, -17.50000000000000000 ) ) ;
#13337 = CARTESIAN_POINT ( 'NONE',  ( -3.464101615137725076, 5.999999999999979572, -174.1636751345948255 ) ) ;
#13338 = ORIENTED_EDGE ( 'NONE', *, *, #22539, .T. ) ;
#13339 = CARTESIAN_POINT ( 'NONE',  ( 155.5312500000000568, -2.485281374238555774, -6.000000000000005329 ) ) ;
#13340 = CARTESIAN_POINT ( 'NONE',  ( 6.000000000000000888, -1.859271017917181981E-14, -137.1636751345948255 ) ) ;
#13341 = EDGE_CURVE ( 'NONE', #305, #28521, #30274, .T. ) ;
#13342 = CARTESIAN_POINT ( 'NONE',  ( 24.94529002296924602, 1.767886127012007424, -1.055868358531008244 ) ) ;
#13343 = ORIENTED_EDGE ( 'NONE', *, *, #5140, .T. ) ;
#13344 = EDGE_CURVE ( 'NONE', #15139, #14585, #10384, .T. ) ;
#13345 = PRESENTATION_LAYER_ASSIGNMENT (  '', '', ( #29966 ) ) ;
#13346 = VERTEX_POINT ( 'NONE', #7399 ) ;
#13347 = CARTESIAN_POINT ( 'NONE',  ( 3.175426480543072749, -5.500000000000105693, -101.1250000000000000 ) ) ;
#13348 = CARTESIAN_POINT ( 'NONE',  ( 3.608439182435180470, -6.249999999999997335, -113.5580127018922383 ) ) ;
#13349 = VERTEX_POINT ( 'NONE', #4923 ) ;
#13350 = CARTESIAN_POINT ( 'NONE',  ( -5.196152422706601826, 2.999999999999975131, -91.53867513459485394 ) ) ;
#13351 = CARTESIAN_POINT ( 'NONE',  ( -40.00000000000000000, -20.00000000000021316, 3.000000000000002665 ) ) ;
#13352 = AXIS2_PLACEMENT_3D ( 'NONE', #6366, #1766, #6072 ) ;
#13353 = LINE ( 'NONE', #13659, #16537 ) ;
#13354 = CARTESIAN_POINT ( 'NONE',  ( -3.608439182435115633, 6.249999999999965361, -52.80801270189225960 ) ) ;
#13355 = VERTEX_POINT ( 'NONE', #11595 ) ;
#13356 = CARTESIAN_POINT ( 'NONE',  ( -4.763139720814407951, -2.750000000000016431, -163.0000000000000284 ) ) ;
#13357 = CARTESIAN_POINT ( 'NONE',  ( 115.1249999999998863, 1.767766952966376426, 1.767766952966320915 ) ) ;
#13358 = CARTESIAN_POINT ( 'NONE',  ( -5.999999999999963585, 1.780251999655701777E-13, -78.83632486540523132 ) ) ;
#13359 = MECHANICAL_DESIGN_GEOMETRIC_PRESENTATION_REPRESENTATION (  '', ( #24109 ), #12373 ) ;
#13360 = CARTESIAN_POINT ( 'NONE',  ( -3.175426480542816066, 5.499999999999865885, -107.8750000000000284 ) ) ;
#13361 = CARTESIAN_POINT ( 'NONE',  ( 23.64882486540533435, 2.500000000000084821, -1.035533905932869425 ) ) ;
#13362 = CARTESIAN_POINT ( 'NONE',  ( 145.9613248654052313, -5.500000000000005329, 0.000000000000000000 ) ) ;
#13363 = CARTESIAN_POINT ( 'NONE',  ( 4.763139720814407951, -2.749999999999988454, -101.0000000000000284 ) ) ;
#13364 = CARTESIAN_POINT ( 'NONE',  ( -5.999999999999957367, 1.607695154586737507, -151.4806624327026157 ) ) ;
#13365 = CARTESIAN_POINT ( 'NONE',  ( 11.35117513459492322, 2.500000000000084821, 1.035533905932689347 ) ) ;
#13366 = CARTESIAN_POINT ( 'NONE',  ( -5.999999999999963585, 1.780251999655701777E-13, -84.83632486540523132 ) ) ;
#13367 = ORIENTED_EDGE ( 'NONE', *, *, #7882, .T. ) ;
#13368 = CARTESIAN_POINT ( 'NONE',  ( 14.18750000000011369, -2.649519052838298805, -1.097466725451559322 ) ) ;
#13369 = CARTESIAN_POINT ( 'NONE',  ( 115.8124999999997584, 1.035533905932719101, -2.499999999999784173 ) ) ;
#13370 = CARTESIAN_POINT ( 'NONE',  ( 111.4377832217621744, 1.849990392679532247, 0.7662911109078888172 ) ) ;
#13371 = CARTESIAN_POINT ( 'NONE',  ( 11.03867513459494454, 1.665334536937734811E-13, -2.500000000000113243 ) ) ;
#13372 =( BOUNDED_CURVE ( )  B_SPLINE_CURVE ( 2, ( #10156, #19529, #28862, #7822, #26564, #3205, #21975, #10305, #8444 ),
 .UNSPECIFIED., .F., .T. ) 
 B_SPLINE_CURVE_WITH_KNOTS ( ( 3, 2, 2, 2, 3 ),
 ( 0.3138888888888888840, 0.3148148148148148251, 0.3166666666666666519, 0.3185185185185185341, 0.3194444444444444753 ),
 .UNSPECIFIED. ) 
 CURVE ( )  GEOMETRIC_REPRESENTATION_ITEM ( )  RATIONAL_B_SPLINE_CURVE ( ( 0.9330127018922194093, 0.9330127018922194093, 1.000000000000000000, 0.8660254037844388186, 1.000000000000000000, 0.8660254037844388186, 1.000000000000000000, 0.9330127018922174109, 0.9330127018922194093 ) ) 
 REPRESENTATION_ITEM ( '' )  );
#13373 = ORIENTED_EDGE ( 'NONE', *, *, #14294, .F. ) ;
#13374 = CARTESIAN_POINT ( 'NONE',  ( 0.000000000000000000, -5.999999999999991118, -169.9613248654052029 ) ) ;
#13375 = CARTESIAN_POINT ( 'NONE',  ( 108.5622167782374277, 1.849990392679501827, -0.7662911109077087390 ) ) ;
#13376 = CARTESIAN_POINT ( 'NONE',  ( 6.000000000000000888, 1.743066579297358182E-13, -96.66367513459479710 ) ) ;
#13377 = ORIENTED_EDGE ( 'NONE', *, *, #2588, .F. ) ;
#13378 = CARTESIAN_POINT ( 'NONE',  ( -3.033369321062190593, 10.57893614291643125, -30.19141222485917808 ) ) ;
#13379 = EDGE_CURVE ( 'NONE', #8771, #12929, #3244, .T. ) ;
#13380 =( BOUNDED_CURVE ( )  B_SPLINE_CURVE ( 2, ( #1253, #20174, #29360, #22011, #947, #10662, #17732, #6022, #22478 ),
 .UNSPECIFIED., .F., .T. ) 
 B_SPLINE_CURVE_WITH_KNOTS ( ( 3, 2, 2, 2, 3 ),
 ( 0.4305555555555555802, 0.4314814814814814659, 0.4333333333333333481, 0.4351851851851852304, 0.4361111111111111160 ),
 .UNSPECIFIED. ) 
 CURVE ( )  GEOMETRIC_REPRESENTATION_ITEM ( )  RATIONAL_B_SPLINE_CURVE ( ( 0.9330127018922194093, 0.9330127018922234061, 1.000000000000000000, 0.8660254037844388186, 1.000000000000000000, 0.8660254037844388186, 1.000000000000000000, 0.9330127018922194093, 0.9330127018922194093 ) ) 
 REPRESENTATION_ITEM ( '' )  );
#13381 = VERTEX_POINT ( 'NONE', #14206 ) ;
#13382 = CARTESIAN_POINT ( 'NONE',  ( 157.4062500000000284, 6.000000000000005329, -2.485281374238555774 ) ) ;
#13383 = CIRCLE ( 'NONE', #9433, 1.000000000000000000 ) ;
#13384 = CARTESIAN_POINT ( 'NONE',  ( 3.175426480543072749, 5.499999999999865885, -121.6250000000000284 ) ) ;
#13385 = CARTESIAN_POINT ( 'NONE',  ( 7.216878364870455975, -6.409875621278545621E-14, -141.8080127018922099 ) ) ;
#13386 = EDGE_LOOP ( 'NONE', ( #19204, #26842, #1423, #27153 ) ) ;
#13387 = CARTESIAN_POINT ( 'NONE',  ( -5.999999999999957367, 1.607695154586737507, -160.4806624327025872 ) ) ;
#13388 = CARTESIAN_POINT ( 'NONE',  ( 3.608439182435180470, 6.249999999999982236, -127.1919872981078186 ) ) ;
#13389 = CARTESIAN_POINT ( 'NONE',  ( 2.775557561562891351E-14, -6.250000000000061284, -178.8169872981077901 ) ) ;
#13390 = CARTESIAN_POINT ( 'NONE',  ( -2.775557561562891351E-14, -5.500000000000115463, -171.7500000000000000 ) ) ;
#13391 = CARTESIAN_POINT ( 'NONE',  ( 160.2454070297168300, -11.22992225825531065, 4.233399354748597965 ) ) ;
#13392 = PRESENTATION_STYLE_ASSIGNMENT (( #24409 ) ) ;
#13393 = ORIENTED_EDGE ( 'NONE', *, *, #4064, .F. ) ;
#13394 = CARTESIAN_POINT ( 'NONE',  ( 12.37500000000013500, -1.414213562372979016, 1.414213562373034527 ) ) ;
#13395 = CARTESIAN_POINT ( 'NONE',  ( 160.2350387298822909, -11.23134877322066849, -4.226361252505896893 ) ) ;
#13396 = CARTESIAN_POINT ( 'NONE',  ( 140.1488248654052029, -3.889087296526011706, -3.889087296526011706 ) ) ;
#13397 = CARTESIAN_POINT ( 'NONE',  ( 23.08632486540540540, -1.767766952966209892, 1.767766952966376426 ) ) ;
#13398 = CARTESIAN_POINT ( 'NONE',  ( 110.1252832217622029, -1.665334536937734811E-13, -1.849990392679412565 ) ) ;
#13399 = CARTESIAN_POINT ( 'NONE',  ( -5.412658773652739619, 3.124999999999975131, -77.31698729810781856 ) ) ;
#13400 = CARTESIAN_POINT ( 'NONE',  ( -5.196152422706601826, 2.999999999999975131, -110.4613248654052171 ) ) ;
#13401 = CARTESIAN_POINT ( 'NONE',  ( -2.775557561562891351E-14, -5.500000000000115463, -47.25000000000001421 ) ) ;
#13402 = CYLINDRICAL_SURFACE ( 'NONE', #15113, 9.999999999999996447 ) ;
#13403 = CARTESIAN_POINT ( 'NONE',  ( -5.999999999999963585, -1.487416814333745711E-14, -153.8363248654052313 ) ) ;
#13404 = CARTESIAN_POINT ( 'NONE',  ( -3.175426480542816510, 5.499999999999865885, -128.8750000000000000 ) ) ;
#13405 = ORIENTED_EDGE ( 'NONE', *, *, #30195, .F. ) ;
#13406 = CARTESIAN_POINT ( 'NONE',  ( -3.464101615137757051, -5.999999999999979572, -119.0863248654052171 ) ) ;
#13407 = EDGE_CURVE ( 'NONE', #3582, #5729, #8578, .T. ) ;
#13408 = CARTESIAN_POINT ( 'NONE',  ( -5.999999999999963585, 0.000000000000000000, -179.3363248654052313 ) ) ;
#13409 = CYLINDRICAL_SURFACE ( 'NONE', #18252, 6.000000000000000888 ) ;
#13410 = CARTESIAN_POINT ( 'NONE',  ( 139.1398502691896510, -3.535533905932752852, 3.535533905932725318 ) ) ;
#13411 = ORIENTED_EDGE ( 'NONE', *, *, #16710, .T. ) ;
#13412 = CARTESIAN_POINT ( 'NONE',  ( 109.1247167782376124, -1.849990392679523588, 1.110223024625156540E-13 ) ) ;
#13413 = CARTESIAN_POINT ( 'NONE',  ( 10.12500000000007816, 1.414213562373201061, 1.414213562373145550 ) ) ;
#13414 = CARTESIAN_POINT ( 'NONE',  ( 2.775557561562891351E-14, 6.250000000000033751, -112.0669872981078186 ) ) ;
#13415 = CARTESIAN_POINT ( 'NONE',  ( 135.0000000000000284, 2.227160363700459556, -5.061403124386353980 ) ) ;
#13416 = MECHANICAL_DESIGN_GEOMETRIC_PRESENTATION_REPRESENTATION (  '', ( #15387 ), #5501 ) ;
#13417 = CARTESIAN_POINT ( 'NONE',  ( 105.7113248654051461, 2.000000000000057288, 0.000000000000000000 ) ) ;
#13418 = ORIENTED_EDGE ( 'NONE', *, *, #13974, .F. ) ;
#13419 = CARTESIAN_POINT ( 'NONE',  ( 159.8821365566051895, -12.37993144645533938, 3.487185471932420011 ) ) ;
#13420 = CARTESIAN_POINT ( 'NONE',  ( 139.3125000000000284, 4.242640687119298093, -4.242640687119298093 ) ) ;
#13421 = ORIENTED_EDGE ( 'NONE', *, *, #26025, .T. ) ;
#13422 = VERTEX_POINT ( 'NONE', #181 ) ;
#13423 =( LENGTH_UNIT ( ) NAMED_UNIT ( * ) SI_UNIT ( .MILLI., .METRE. ) );
#13424 = CARTESIAN_POINT ( 'NONE',  ( -3.175426480542816510, -5.500000000000057732, -51.87500000000002132 ) ) ;
#13425 = CARTESIAN_POINT ( 'NONE',  ( 21.93750000000006395, 2.000000000000212275, -0.8284271247462955401 ) ) ;
#13426 = DIRECTION ( 'NONE',  ( -7.147005652999508048E-36, 5.642372883946980038E-36, 1.000000000000000000 ) ) ;
#13427 = CARTESIAN_POINT ( 'NONE',  ( 105.0446384121982675, -1.023503819632144651, 1.804923305114234156 ) ) ;
#13428 = CARTESIAN_POINT ( 'NONE',  ( -3.608439182435052128, -6.250000000000110134, -65.80801270189225249 ) ) ;
#13429 = AXIS2_PLACEMENT_3D ( 'NONE', #18601, #27322, #27459 ) ;
#13430 = CARTESIAN_POINT ( 'NONE',  ( 149.8913997308104058, -2.071067811865468400, 4.999999999999989342 ) ) ;
#13431 = CARTESIAN_POINT ( 'NONE',  ( -5.999999999999963585, 1.780251999655701777E-13, -77.33632486540524553 ) ) ;
#13432 = CARTESIAN_POINT ( 'NONE',  ( -21.99999999999993605, 11.00000000000003730, -14.99152654425661879 ) ) ;
#13433 = DIRECTION ( 'NONE',  ( 0.000000000000000000, 0.000000000000000000, -1.000000000000000000 ) ) ;
#13434 = SURFACE_SIDE_STYLE ('',( #18346 ) ) ;
#13435 = CARTESIAN_POINT ( 'NONE',  ( -2.775557561562891351E-14, -5.500000000000115463, -129.7500000000000284 ) ) ;
#13436 = CARTESIAN_POINT ( 'NONE',  ( 137.5386751345948255, -5.500000000000005329, 0.000000000000000000 ) ) ;
#13437 = CARTESIAN_POINT ( 'NONE',  ( 0.000000000000000000, 0.000000000000000000, 0.000000000000000000 ) ) ;
#13438 = CARTESIAN_POINT ( 'NONE',  ( -5.999999999999963585, 3.021315404115421074E-15, -177.8363248654052029 ) ) ;
#13439 = ORIENTED_EDGE ( 'NONE', *, *, #26102, .T. ) ;
#13440 = EDGE_CURVE ( 'NONE', #19914, #24100, #20, .T. ) ;
#13441 = CARTESIAN_POINT ( 'NONE',  ( -3.175426480542816066, 5.499999999999865885, -61.37500000000000711 ) ) ;
#13442 = DIRECTION ( 'NONE',  ( 1.000000000000000000, -5.551115123125773458E-17, -1.260129944081490338E-35 ) ) ;
#13443 = DIRECTION ( 'NONE',  ( 1.000000000000000000, 0.000000000000000000, 0.000000000000000000 ) ) ;
#13444 = CARTESIAN_POINT ( 'NONE',  ( -3.464101615137757051, -5.999999999999979572, -174.5863248654051745 ) ) ;
#13445 = ORIENTED_EDGE ( 'NONE', *, *, #25187, .F. ) ;
#13446 = CARTESIAN_POINT ( 'NONE',  ( 108.1874999999998579, 1.035533905932719101, 2.500000000000205169 ) ) ;
#13447 = CARTESIAN_POINT ( 'NONE',  ( 146.1562500000000568, -6.000000000000005329, 2.485281374238556218 ) ) ;
#13448 = DIRECTION ( 'NONE',  ( 1.000000000000000000, 6.938893903907222067E-15, 0.000000000000000000 ) ) ;
#13449 = CARTESIAN_POINT ( 'NONE',  ( 13.56250000000003375, -1.999999999999971800, -0.8284271247462354770 ) ) ;
#13450 = LINE ( 'NONE', #22495, #26339 ) ;
#13451 = ADVANCED_FACE ( 'NONE', ( #20936 ), #28121, .F. ) ;
#13452 = AXIS2_PLACEMENT_3D ( 'NONE', #26427, #21699, #8137 ) ;
#13453 = CARTESIAN_POINT ( 'NONE',  ( 136.8750000000000284, 0.000000000000000000, 6.000000000000005329 ) ) ;
#13454 = CARTESIAN_POINT ( 'NONE',  ( 14.14882486540528816, -2.499999999999964473, 1.035533905932749299 ) ) ;
#13455 = COLOUR_RGB ( '', 0.31764706, 0.68627451, 0.89019608) ;
#13456 = VERTEX_POINT ( 'NONE', #11744 ) ;
#13457 =( BOUNDED_CURVE ( )  B_SPLINE_CURVE ( 2, ( #19815, #3822, #10935, #3359, #17539, #7979, #12632, #3666, #15401 ),
 .UNSPECIFIED., .F., .F. ) 
 B_SPLINE_CURVE_WITH_KNOTS ( ( 3, 2, 2, 2, 3 ),
 ( 0.2343750000000000000, 0.2421875000000000000, 0.2500000000000000000, 0.2578125000000000000, 0.2656250000000000000 ),
 .UNSPECIFIED. ) 
 CURVE ( )  GEOMETRIC_REPRESENTATION_ITEM ( )  RATIONAL_B_SPLINE_CURVE ( ( 1.000000000000000000, 0.9238795325112867385, 1.000000000000000000, 0.9238795325112867385, 1.000000000000000000, 0.9238795325112867385, 1.000000000000000000, 0.9238795325112867385, 1.000000000000000000 ) ) 
 REPRESENTATION_ITEM ( '' )  );
#13458 = CARTESIAN_POINT ( 'NONE',  ( 0.000000000000000000, 5.499999999999991118, -144.0000000000000284 ) ) ;
#13459 = ORIENTED_EDGE ( 'NONE', *, *, #28782, .T. ) ;
#13460 = CARTESIAN_POINT ( 'NONE',  ( 13.00000000000003908, 2.000000000000112799, 0.000000000000000000 ) ) ;
#13461 = VERTEX_POINT ( 'NONE', #21089 ) ;
#13462 = CARTESIAN_POINT ( 'NONE',  ( -6.350852961085760029, -1.281975124255709124E-13, -74.62500000000000000 ) ) ;
#13463 = CARTESIAN_POINT ( 'NONE',  ( 3.608439182435180470, -6.249999999999997335, -88.05801270189223828 ) ) ;
#13464 =( BOUNDED_CURVE ( )  B_SPLINE_CURVE ( 2, ( #27282, #5785, #29440, #6256, #17819, #24984, #3934, #13364, #1650 ),
 .UNSPECIFIED., .F., .T. ) 
 B_SPLINE_CURVE_WITH_KNOTS ( ( 3, 2, 2, 2, 3 ),
 ( 0.2194444444444444697, 0.2203703703703703831, 0.2222222222222222099, 0.2240740740740740644, 0.2249999999999999778 ),
 .UNSPECIFIED. ) 
 CURVE ( )  GEOMETRIC_REPRESENTATION_ITEM ( )  RATIONAL_B_SPLINE_CURVE ( ( 0.9330127018922194093, 0.9330127018922204085, 1.000000000000000000, 0.8660254037844388186, 1.000000000000000000, 0.8660254037844388186, 1.000000000000000000, 0.9330127018922205195, 0.9330127018922196314 ) ) 
 REPRESENTATION_ITEM ( '' )  );
#13465 = CARTESIAN_POINT ( 'NONE',  ( 119.9999999999998437, -0.3289648646781667685, 2.003997983321501586 ) ) ;
#13466 = B_SPLINE_CURVE_WITH_KNOTS ( 'NONE', 3,
 ( #26640, #22526, #17934, #10546, #19903, #29404, #27250, #19749, #24342, #24809 ),
 .UNSPECIFIED., .F., .F.,
 ( 4, 2, 2, 2, 4 ),
 ( 0.000000000000000000, 0.001275962895115241537, 0.002551925790230482639, 0.003827888685345722658, 0.005103851580460961809 ),
 .UNSPECIFIED. ) ;
#13467 = CARTESIAN_POINT ( 'NONE',  ( 5.196152422706629359, 3.000000000000002665, -150.5386751345948539 ) ) ;
#13468 = CARTESIAN_POINT ( 'NONE',  ( 6.000000000000000888, 1.743066579297358182E-13, -53.16367513459481131 ) ) ;
#13469 = CARTESIAN_POINT ( 'NONE',  ( 24.49999999999999289, 0.6095397824026904665, 2.424553825690067832 ) ) ;
#13470 = CARTESIAN_POINT ( 'NONE',  ( 0.000000000000000000, 0.000000000000000000, 0.000000000000000000 ) ) ;
#13471 = DIRECTION ( 'NONE',  ( 0.000000000000000000, 0.000000000000000000, 1.000000000000000000 ) ) ;
#13472 = CARTESIAN_POINT ( 'NONE',  ( 0.000000000000000000, 5.499999999999991118, -157.5000000000000284 ) ) ;
#13473 = CARTESIAN_POINT ( 'NONE',  ( 139.9451382466496057, -9.135892426262346433, -7.783435338407951321 ) ) ;
#13474 = AXIS2_PLACEMENT_3D ( 'NONE', #23102, #30145, #23260 ) ;
#13475 = DIRECTION ( 'NONE',  ( -1.000000000000000000, -1.734723475976843579E-16, 0.000000000000000000 ) ) ;
#13476 = EDGE_CURVE ( 'NONE', #30226, #2399, #21956, .T. ) ;
#13477 = CARTESIAN_POINT ( 'NONE',  ( 6.350852961086080661, -9.614813431917819062E-14, -90.37500000000001421 ) ) ;
#13478 = CARTESIAN_POINT ( 'NONE',  ( 117.2113248654051034, -1.999999999999890754, 3.330669073875469621E-13 ) ) ;
#13479 = CARTESIAN_POINT ( 'NONE',  ( 4.763139720814407951, -2.749999999999988454, -69.50000000000000000 ) ) ;
#13480 = CYLINDRICAL_SURFACE ( 'NONE', #13882, 6.000000000000000888 ) ;
#13481 = CARTESIAN_POINT ( 'NONE',  ( 149.7336002691896226, -4.999999999999989342, 2.071067811865468400 ) ) ;
#13482 = CARTESIAN_POINT ( 'NONE',  ( 0.000000000000000000, 5.999999999999977796, -164.7113248654051745 ) ) ;
#13483 = CARTESIAN_POINT ( 'NONE',  ( 6.000000000000000888, -3.330669073875464691E-16, -7.560779664488942560E-35 ) ) ;
#13484 = CARTESIAN_POINT ( 'NONE',  ( 135.4369327280547566, -8.875721941249034685, -8.012675569329063663 ) ) ;
#13485 = CARTESIAN_POINT ( 'NONE',  ( 5.196152422706629359, 3.000000000000002665, -104.0386751345948539 ) ) ;
#13486 = CARTESIAN_POINT ( 'NONE',  ( 19.56250000000009948, -1.999999999999911626, -0.8284271247461753029 ) ) ;
#13487 = CARTESIAN_POINT ( 'NONE',  ( -3.464101615137725076, 5.999999999999979572, -94.66367513459479710 ) ) ;
#13488 = DIRECTION ( 'NONE',  ( -7.147005652999508048E-36, 5.642372883946980038E-36, 1.000000000000000000 ) ) ;
#13489 = ADVANCED_FACE ( 'NONE', ( #10161 ), #28867, .T. ) ;
#13490 = DIRECTION ( 'NONE',  ( 1.000000000000000000, 0.000000000000000000, 0.000000000000000000 ) ) ;
#13491 = ORIENTED_EDGE ( 'NONE', *, *, #29132, .T. ) ;
#13492 = CARTESIAN_POINT ( 'NONE',  ( 155.8125000000000284, 4.242640687119298093, -4.242640687119298093 ) ) ;
#13493 = DIRECTION ( 'NONE',  ( -7.147005652999508048E-36, 5.642372883946980038E-36, 1.000000000000000000 ) ) ;
#13494 = CARTESIAN_POINT ( 'NONE',  ( 118.9377832217621460, -1.849990392679472073, -0.7662911109077087390 ) ) ;
#13495 = CARTESIAN_POINT ( 'NONE',  ( 6.000000000000000888, -1.859271017917181981E-14, -147.6636751345948255 ) ) ;
#13496 = VERTEX_POINT ( 'NONE', #15077 ) ;
#13497 = ORIENTED_EDGE ( 'NONE', *, *, #25590, .T. ) ;
#13498 = CARTESIAN_POINT ( 'NONE',  ( -3.175426480542816510, -5.500000000000057732, -99.87500000000000000 ) ) ;
#13499 = CONICAL_SURFACE ( 'NONE', #2180, 6.500000000000016875, 0.7419472680059175929 ) ;
#13500 = CARTESIAN_POINT ( 'NONE',  ( 17.46132486540527395, 5.551115123125782702E-14, -2.500000000000002220 ) ) ;
#13501 = CARTESIAN_POINT ( 'NONE',  ( 5.412658773652712085, -3.125000000000086153, -105.9330127018922667 ) ) ;
#13502 = ORIENTED_EDGE ( 'NONE', *, *, #6301, .T. ) ;
#13503 = CARTESIAN_POINT ( 'NONE',  ( 2.799076333356274106E-14, 11.00000000000000000, -19.00000000000002132 ) ) ;
#13504 = DIRECTION ( 'NONE',  ( -0.000000000000000000, -0.000000000000000000, -1.000000000000000000 ) ) ;
#13505 = CARTESIAN_POINT ( 'NONE',  ( -4.763139720814407951, 2.749999999999946709, -166.2500000000000000 ) ) ;
#13506 = CARTESIAN_POINT ( 'NONE',  ( -3.608439182435052128, -6.250000000000110134, -53.80801270189219565 ) ) ;
#13507 = CARTESIAN_POINT ( 'NONE',  ( -5.999999999999963585, 1.780251999655701777E-13, -56.33632486540525264 ) ) ;
#13508 = ORIENTED_EDGE ( 'NONE', *, *, #27367, .F. ) ;
#13509 = LINE ( 'NONE', #4242, #24658 ) ;
#13510 = CARTESIAN_POINT ( 'NONE',  ( 5.196152422706629359, -2.999999999999988898, -166.7113248654051745 ) ) ;
#13511 = CARTESIAN_POINT ( 'NONE',  ( -2.775557561562891351E-14, -5.500000000000115463, -159.7500000000000568 ) ) ;
#13512 = CARTESIAN_POINT ( 'NONE',  ( 116.0624999999999005, 2.500000000000055067, 1.035533905932929599 ) ) ;
#13513 = DIRECTION ( 'NONE',  ( 1.000000000000000000, -5.551115123125773458E-17, -1.260129944081490338E-35 ) ) ;
#13514 =( BOUNDED_CURVE ( )  B_SPLINE_CURVE ( 2, ( #17390, #3362, #7827, #8452, #12496, #12791, #26705, #5988, #10311 ),
 .UNSPECIFIED., .F., .F. ) 
 B_SPLINE_CURVE_WITH_KNOTS ( ( 3, 2, 2, 2, 3 ),
 ( 0.3916666666666666630, 0.3925925925925926041, 0.3944444444444444309, 0.3962962962962963132, 0.3972222222222222543 ),
 .UNSPECIFIED. ) 
 CURVE ( )  GEOMETRIC_REPRESENTATION_ITEM ( )  RATIONAL_B_SPLINE_CURVE ( ( 0.9330127018922194093, 0.9330127018922194093, 1.000000000000000000, 0.8660254037844388186, 1.000000000000000000, 0.8660254037844388186, 1.000000000000000000, 0.9330127018922174109, 0.9330127018922194093 ) ) 
 REPRESENTATION_ITEM ( '' )  );
#13515 = ADVANCED_FACE ( 'NONE', ( #26859 ), #21542, .T. ) ;
#13516 = CARTESIAN_POINT ( 'NONE',  ( -2.775557561562891351E-14, -5.500000000000115463, -105.7500000000000142 ) ) ;
#13517 = CARTESIAN_POINT ( 'NONE',  ( 105.7113248654051461, 2.000000000000057288, 0.000000000000000000 ) ) ;
#13518 = CARTESIAN_POINT ( 'NONE',  ( 6.000000000000000888, 1.743066579297358182E-13, -87.66367513459482552 ) ) ;
#13519 = EDGE_CURVE ( 'NONE', #26206, #23261, #17092, .T. ) ;
#13520 = CARTESIAN_POINT ( 'NONE',  ( 3.175426480543072749, -5.500000000000105693, -98.12500000000004263 ) ) ;
#13521 = CARTESIAN_POINT ( 'NONE',  ( 160.7961002691896510, 2.071067811865468400, -4.999999999999989342 ) ) ;
#13522 = CARTESIAN_POINT ( 'NONE',  ( -0.04562205425673543369, -14.50000000000001243, 8.291335958003944739 ) ) ;
#13523 = ORIENTED_EDGE ( 'NONE', *, *, #4523, .T. ) ;
#13524 = CARTESIAN_POINT ( 'NONE',  ( 11.43750000000000355, 1.097466725451559322, -2.649519052838298805 ) ) ;
#13525 = CARTESIAN_POINT ( 'NONE',  ( 117.3750000000000142, -1.767766952966320915, 1.767766952966431937 ) ) ;
#13526 = CARTESIAN_POINT ( 'NONE',  ( 111.9377832217620465, -1.849990392679441875, -0.7662911109075883909 ) ) ;
#13527 = CARTESIAN_POINT ( 'NONE',  ( 116.0000000000000142, 6.735557395310442023E-16, 5.500000000000000000 ) ) ;
#13528 = ORIENTED_EDGE ( 'NONE', *, *, #12480, .T. ) ;
#13529 = FACE_OUTER_BOUND ( 'NONE', #5767, .T. ) ;
#13530 = CARTESIAN_POINT ( 'NONE',  ( 109.3747167782375556, -1.665334536937734811E-13, -1.849990392679523588 ) ) ;
#13531 = CARTESIAN_POINT ( 'NONE',  ( 3.608439182435180470, 6.249999999999982236, -91.19198729810783277 ) ) ;
#13532 = ORIENTED_EDGE ( 'NONE', *, *, #8021, .F. ) ;
#13533 = CARTESIAN_POINT ( 'NONE',  ( 6.055081547227420202, 0.000000000000000000, 0.000000000000000000 ) ) ;
#13534 = ORIENTED_EDGE ( 'NONE', *, *, #22809, .F. ) ;
#13535 = CARTESIAN_POINT ( 'NONE',  ( 157.8750000000000568, 0.000000000000000000, 6.000000000000005329 ) ) ;
#13536 = ORIENTED_EDGE ( 'NONE', *, *, #1921, .T. ) ;
#13537 = VECTOR ( 'NONE', #30374, 1000.000000000000000 ) ;
#13538 = CARTESIAN_POINT ( 'NONE',  ( -3.175426480542816510, -5.500000000000057732, -117.8750000000000142 ) ) ;
#13539 = CARTESIAN_POINT ( 'NONE',  ( 2.775557561562891351E-14, 6.250000000000033751, -139.9330127018922383 ) ) ;
#13540 = ORIENTED_EDGE ( 'NONE', *, *, #23519, .T. ) ;
#13541 = CARTESIAN_POINT ( 'NONE',  ( 156.9300748654052313, 2.278174593051842223, -5.500000000000182077 ) ) ;
#13542 = CARTESIAN_POINT ( 'NONE',  ( 7.216878364870455975, -6.409875621278545621E-14, -125.9419872981078186 ) ) ;
#13543 = CARTESIAN_POINT ( 'NONE',  ( -3.608439182435052128, -6.250000000000110134, -177.4419872981078470 ) ) ;
#13544 = CARTESIAN_POINT ( 'NONE',  ( 159.8766298123001093, -12.37305747749753415, 3.498085420967321113 ) ) ;
#13545 = ORIENTED_EDGE ( 'NONE', *, *, #17310, .T. ) ;
#13546 = CARTESIAN_POINT ( 'NONE',  ( 12.25000000000006573, 5.551115123125782702E-14, 1.999999999999946265 ) ) ;
#13547 = FACE_OUTER_BOUND ( 'NONE', #2972, .T. ) ;
#13548 = CARTESIAN_POINT ( 'NONE',  ( 0.000000000000000000, 0.000000000000000000, 0.000000000000000000 ) ) ;
#13549 = AXIS2_PLACEMENT_3D ( 'NONE', #6621, #13124, #20613 ) ;
#13550 = CARTESIAN_POINT ( 'NONE',  ( 119.9999999999997868, -1.999999999999875211, 2.320366121466830552E-14 ) ) ;
#13551 = DIRECTION ( 'NONE',  ( 1.000000000000000000, -5.551115123125773458E-17, 0.000000000000000000 ) ) ;
#13552 = CARTESIAN_POINT ( 'NONE',  ( 3.608439182435180470, -6.249999999999997335, -61.69198729810783988 ) ) ;
#13553 = CARTESIAN_POINT ( 'NONE',  ( -3.464101615137757051, -5.999999999999979572, -170.6636751345948255 ) ) ;
#13554 = CARTESIAN_POINT ( 'NONE',  ( 6.350852961086080661, -9.614813431917819062E-14, -49.87500000000001421 ) ) ;
#13555 = LINE ( 'NONE', #25171, #2803 ) ;
#13556 = FACE_OUTER_BOUND ( 'NONE', #9545, .T. ) ;
#13557 =( BOUNDED_CURVE ( )  B_SPLINE_CURVE ( 2, ( #10939, #3977, #13400, #20430, #29789, #25169, #18758, #1992, #4886 ),
 .UNSPECIFIED., .F., .T. ) 
 B_SPLINE_CURVE_WITH_KNOTS ( ( 3, 2, 2, 2, 3 ),
 ( 0.4750000000000000888, 0.4759259259259259744, 0.4777777777777777457, 0.4796296296296296280, 0.4805555555555555136 ),
 .UNSPECIFIED. ) 
 CURVE ( )  GEOMETRIC_REPRESENTATION_ITEM ( )  RATIONAL_B_SPLINE_CURVE ( ( 0.9330127018922194093, 0.9330127018922234061, 1.000000000000000000, 0.8660254037844388186, 1.000000000000000000, 0.8660254037844388186, 1.000000000000000000, 0.9330127018922234061, 0.9330127018922194093 ) ) 
 REPRESENTATION_ITEM ( '' )  );
#13558 = ADVANCED_FACE ( 'NONE', ( #8127 ), #9863, .F. ) ;
#13559 = CARTESIAN_POINT ( 'NONE',  ( 3.175426480543072749, 5.499999999999865885, -120.1250000000000284 ) ) ;
#13560 = CARTESIAN_POINT ( 'NONE',  ( 117.2113248654051034, -1.999999999999890754, 3.330669073875469621E-13 ) ) ;
#13561 = CARTESIAN_POINT ( 'NONE',  ( 104.7401757384974985, -0.1191742713688042632, -1.850113936623924538 ) ) ;
#13562 = ORIENTED_EDGE ( 'NONE', *, *, #7947, .F. ) ;
#13563 = CARTESIAN_POINT ( 'NONE',  ( 22.12500000000006040, -2.649519052838111843, 0.000000000000000000 ) ) ;
#13564 = AXIS2_PLACEMENT_3D ( 'NONE', #22488, #29536, #17898 ) ;
#13565 = LINE ( 'NONE', #9070, #21458 ) ;
#13566 = FACE_OUTER_BOUND ( 'NONE', #6759, .T. ) ;
#13567 = CARTESIAN_POINT ( 'NONE',  ( 137.2648502691896510, 3.535533905932725318, 3.535533905932752852 ) ) ;
#13568 = VERTEX_POINT ( 'NONE', #24569 ) ;
#13569 = CARTESIAN_POINT ( 'NONE',  ( 111.6247167782376408, 1.849990392679523588, 0.000000000000000000 ) ) ;
#13570 = CARTESIAN_POINT ( 'NONE',  ( -14.99999999999999289, -25.00000000000007816, 7.500000000000007105 ) ) ;
#13571 = CARTESIAN_POINT ( 'NONE',  ( 2.775557561562891351E-14, 6.250000000000033751, -113.5669872981078186 ) ) ;
#13572 = CARTESIAN_POINT ( 'NONE',  ( 6.000000000000000888, -1.859271017917181981E-14, -109.5863248654052029 ) ) ;
#13573 = AXIS2_PLACEMENT_3D ( 'NONE', #29765, #11218, #6730 ) ;
#13574 = CARTESIAN_POINT ( 'NONE',  ( 113.6488248654048618, 2.000000000000122125, -0.8284271247460553989 ) ) ;
#13575 = ORIENTED_EDGE ( 'NONE', *, *, #399, .F. ) ;
#13576 = VERTEX_POINT ( 'NONE', #16943 ) ;
#13577 = CARTESIAN_POINT ( 'NONE',  ( 6.000000000000000888, -1.859271017917181981E-14, -126.0863248654052171 ) ) ;
#13578 = CARTESIAN_POINT ( 'NONE',  ( 142.0312500000000284, -2.485281374238555774, -6.000000000000005329 ) ) ;
#13579 = CARTESIAN_POINT ( 'NONE',  ( 7.216878364870455975, -6.409875621278545621E-14, -145.4419872981078470 ) ) ;
#13580 = CARTESIAN_POINT ( 'NONE',  ( -5.999999999999962697, 3.323446944526963891E-14, -157.4136751345948539 ) ) ;
#13581 = SURFACE_STYLE_FILL_AREA ( #1559 ) ;
#13582 = AXIS2_PLACEMENT_3D ( 'NONE', #18048, #24914, #27510 ) ;
#13583 = EDGE_CURVE ( 'NONE', #13146, #5962, #26272, .T. ) ;
#13584 = CARTESIAN_POINT ( 'NONE',  ( 14.66367513459496053, -1.767766952966320915, 1.767766952966431937 ) ) ;
#13585 = CARTESIAN_POINT ( 'NONE',  ( 24.87500000000009237, 1.414213562373312083, -1.414213562373145550 ) ) ;
#13586 = DIRECTION ( 'NONE',  ( 1.000000000000000000, -0.000000000000000000, -0.000000000000000000 ) ) ;
#13587 = DIRECTION ( 'NONE',  ( -1.000000000000000000, 0.000000000000000000, 0.000000000000000000 ) ) ;
#13588 = CARTESIAN_POINT ( 'NONE',  ( 7.216878364870455975, -6.409875621278545621E-14, -68.30801270189220986 ) ) ;
#13589 = CARTESIAN_POINT ( 'NONE',  ( 144.0788997308104058, -4.999999999999989342, 2.071067811865468400 ) ) ;
#13590 = CARTESIAN_POINT ( 'NONE',  ( 5.196152422706629359, -2.999999999999988898, -177.7886751345948539 ) ) ;
#13591 = CARTESIAN_POINT ( 'NONE',  ( -20.99177011976446394, 10.49588505988223375, -1.500282997124227719E-34 ) ) ;
#13592 = CARTESIAN_POINT ( 'NONE',  ( -5.999999999999962697, 3.323446944526963891E-14, -156.8363248654052313 ) ) ;
#13593 = CYLINDRICAL_SURFACE ( 'NONE', #15311, 12.00000000000000178 ) ;
#13594 = EDGE_CURVE ( 'NONE', #4124, #19006, #3264, .T. ) ;
#13595 = CARTESIAN_POINT ( 'NONE',  ( 3.175426480543072749, -5.500000000000105693, -120.6250000000000284 ) ) ;
#13596 = CYLINDRICAL_SURFACE ( 'NONE', #12585, 2.499999999999999112 ) ;
#13597 = ORIENTED_EDGE ( 'NONE', *, *, #28715, .T. ) ;
#13598 = CARTESIAN_POINT ( 'NONE',  ( 4.763139720814407951, 2.750000000000002665, -52.75000000000002132 ) ) ;
#13599 = CARTESIAN_POINT ( 'NONE',  ( 6.000000000000014211, -1.607695154586730180, -153.7306624327026157 ) ) ;
#13600 = FACE_OUTER_BOUND ( 'NONE', #904, .T. ) ;
#13601 = CARTESIAN_POINT ( 'NONE',  ( 3.464101615137757051, -5.999999999999979572, -162.9136751345947971 ) ) ;
#13602 = VERTEX_POINT ( 'NONE', #22441 ) ;
#13603 = CARTESIAN_POINT ( 'NONE',  ( 104.9999999999998579, 2.500000000000002220, 0.000000000000000000 ) ) ;
#13604 = CARTESIAN_POINT ( 'NONE',  ( 147.8437500000000284, -6.000000000000005329, -2.485281374238556218 ) ) ;
#13605 = CARTESIAN_POINT ( 'NONE',  ( 12.62500000000013678, -1.414213562372979016, -1.414213562373145550 ) ) ;
#13606 = CARTESIAN_POINT ( 'NONE',  ( 111.2886751345946834, 2.000000000000001776, 3.330669073875469621E-13 ) ) ;
#13607 = CARTESIAN_POINT ( 'NONE',  ( 136.9687500000000000, -2.485281374238585972, 6.000000000000005329 ) ) ;
#13608 = CARTESIAN_POINT ( 'NONE',  ( 14.21132486540527218, -2.499999999999946709, -5.551115123125782702E-14 ) ) ;
#13609 = VERTEX_POINT ( 'NONE', #27326 ) ;
#13610 = CARTESIAN_POINT ( 'NONE',  ( -6.350852961085760029, -1.281975124255709124E-13, -140.6249999999999716 ) ) ;
#13611 = VERTEX_POINT ( 'NONE', #27022 ) ;
#13612 = CARTESIAN_POINT ( 'NONE',  ( 11.50000000000006573, -1.999999999999835243, 0.000000000000000000 ) ) ;
#13613 = ORIENTED_EDGE ( 'NONE', *, *, #17212, .F. ) ;
#13614 = EDGE_CURVE ( 'NONE', #23117, #18461, #15060, .T. ) ;
#13615 = CARTESIAN_POINT ( 'NONE',  ( 6.350852961086080661, -9.614813431917819062E-14, -73.87500000000000000 ) ) ;
#13616 = CARTESIAN_POINT ( 'NONE',  ( 18.96132486540530593, 1.110223024625156540E-13, 2.499999999999724665 ) ) ;
#13617 = CARTESIAN_POINT ( 'NONE',  ( -2.511346088334902138, -10.71107091704336156, -30.45263927933804027 ) ) ;
#13618 = CARTESIAN_POINT ( 'NONE',  ( -5.999999999999963585, -1.487416814333745711E-14, -134.3363248654052313 ) ) ;
#13619 = CARTESIAN_POINT ( 'NONE',  ( 140.1146164139961456, -11.55730820707150919, -4.524920606409365220 ) ) ;
#13620 = CYLINDRICAL_SURFACE ( 'NONE', #2971, 6.000000000000000888 ) ;
#13621 = CARTESIAN_POINT ( 'NONE',  ( 120.2502832217622739, 1.308140751793612777, -1.308140751793418488 ) ) ;
#13622 = EDGE_CURVE ( 'NONE', #15775, #9719, #27174, .T. ) ;
#13623 = CONTEXT_DEPENDENT_SHAPE_REPRESENTATION ( #15806, #9450 ) ;
#13624 = CARTESIAN_POINT ( 'NONE',  ( -6.350852961085760029, -1.281975124255709124E-13, -146.6250000000000284 ) ) ;
#13625 = CARTESIAN_POINT ( 'NONE',  ( 140.1633619592320770, -9.008502785496828480, -7.928502883319133332 ) ) ;
#13626 = CARTESIAN_POINT ( 'NONE',  ( 5.412658773652712085, -3.125000000000086153, -164.4330127018922667 ) ) ;
#13627 = CARTESIAN_POINT ( 'NONE',  ( 22.53867513459501026, 1.110223024625156540E-13, 2.499999999999835687 ) ) ;
#13628 = TOROIDAL_SURFACE ( 'NONE', #12633, 9.999999999999998224, 1.000000000000000000 ) ;
#13629 = CARTESIAN_POINT ( 'NONE',  ( 6.350852961086080661, -9.614813431917819062E-14, -87.37500000000005684 ) ) ;
#13630 = VECTOR ( 'NONE', #6336, 1000.000000000000000 ) ;
#13631 = VECTOR ( 'NONE', #6609, 1000.000000000000000 ) ;
#13632 = CARTESIAN_POINT ( 'NONE',  ( 116.9613248654049897, 5.551115123125782702E-14, 2.000000000000223821 ) ) ;
#13633 = CARTESIAN_POINT ( 'NONE',  ( 0.000000000000000000, 5.499999999999991118, -75.00000000000001421 ) ) ;
#13634 = LINE ( 'NONE', #22981, #15214 ) ;
#13635 = LINE ( 'NONE', #13795, #30181 ) ;
#13636 = AXIS2_PLACEMENT_3D ( 'NONE', #26583, #15097, #7699 ) ;
#13637 = CARTESIAN_POINT ( 'NONE',  ( 0.000000000000000000, -5.999999999999991118, -71.53867513459482552 ) ) ;
#13638 = CARTESIAN_POINT ( 'NONE',  ( 20.75000000000012790, 1.665334536937734811E-13, -2.000000000000001776 ) ) ;
#13639 = CARTESIAN_POINT ( 'NONE',  ( 0.000000000000000000, 0.000000000000000000, 0.000000000000000000 ) ) ;
#13640 = CARTESIAN_POINT ( 'NONE',  ( 117.2497167782375129, -1.308140751793585022, -1.308140751793640533 ) ) ;
#13641 = CARTESIAN_POINT ( 'NONE',  ( 6.000000000000000888, 7.762456499804234384E-14, -139.5863248654051745 ) ) ;
#13642 =( BOUNDED_CURVE ( )  B_SPLINE_CURVE ( 2, ( #25090, #30320, #18522 ),
 .UNSPECIFIED., .F., .F. ) 
 B_SPLINE_CURVE_WITH_KNOTS ( ( 3, 3 ),
 ( 0.01327334991652243112, 0.01388888888888888465 ),
 .UNSPECIFIED. ) 
 CURVE ( )  GEOMETRIC_REPRESENTATION_ITEM ( )  RATIONAL_B_SPLINE_CURVE ( ( 0.9626167487138490575, 0.9330127018922196314, 0.9330127018922194093 ) ) 
 REPRESENTATION_ITEM ( '' )  );
#13643 = ORIENTED_EDGE ( 'NONE', *, *, #16133, .F. ) ;
#13644 = CARTESIAN_POINT ( 'NONE',  ( 153.5625000000000568, -4.242640687119298093, 4.242640687119298093 ) ) ;
#13645 = CARTESIAN_POINT ( 'NONE',  ( 5.196152422706629359, -2.999999999999988898, -108.7886751345948397 ) ) ;
#13646 = AXIS2_PLACEMENT_3D ( 'NONE', #18395, #8856, #4071 ) ;
#13647 = CARTESIAN_POINT ( 'NONE',  ( 118.0627832217622455, -0.7662911109076485650, -1.849990392679171425 ) ) ;
#13648 = APPLICATION_CONTEXT ( 'automotive_design' ) ;
#13649 = CARTESIAN_POINT ( 'NONE',  ( -20.99999999999998224, -54.99999999999990763, 4.000000000000003553 ) ) ;
#13650 = ORIENTED_EDGE ( 'NONE', *, *, #168, .F. ) ;
#13651 = ORIENTED_EDGE ( 'NONE', *, *, #11537, .T. ) ;
#13652 =( BOUNDED_CURVE ( )  B_SPLINE_CURVE ( 2, ( #6003, #24749, #27037, #15421, #7763, #20066, #12729, #29412, #29102 ),
 .UNSPECIFIED., .F., .T. ) 
 B_SPLINE_CURVE_WITH_KNOTS ( ( 3, 2, 2, 2, 3 ),
 ( 0.3305555555555556024, 0.3314814814814814881, 0.3333333333333333703, 0.3351851851851851416, 0.3361111111111110272 ),
 .UNSPECIFIED. ) 
 CURVE ( )  GEOMETRIC_REPRESENTATION_ITEM ( )  RATIONAL_B_SPLINE_CURVE ( ( 0.9330127018922194093, 0.9330127018922234061, 1.000000000000000000, 0.8660254037844388186, 1.000000000000000000, 0.8660254037844388186, 1.000000000000000000, 0.9330127018922234061, 0.9330127018922194093 ) ) 
 REPRESENTATION_ITEM ( '' )  );
#13653 = AXIS2_PLACEMENT_3D ( 'NONE', #18701, #2393, #27714 ) ;
#13654 = ORIENTED_EDGE ( 'NONE', *, *, #26369, .F. ) ;
#13655 = EDGE_CURVE ( 'NONE', #1119, #1053, #15748, .T. ) ;
#13656 = CARTESIAN_POINT ( 'NONE',  ( 4.763139720814407951, -2.749999999999988454, -96.50000000000002842 ) ) ;
#13657 = CARTESIAN_POINT ( 'NONE',  ( 5.412658773652739619, 3.124999999999988898, -104.1830127018922241 ) ) ;
#13658 = CARTESIAN_POINT ( 'NONE',  ( 140.0493945286584108, -8.932592928453178871, -8.013407610087551092 ) ) ;
#13659 = CARTESIAN_POINT ( 'NONE',  ( -4.999999999999984013, -69.50000000000001421, -8.000000000000007105 ) ) ;
#13660 = CARTESIAN_POINT ( 'NONE',  ( 0.4053696738521634368, -11.00000000000001066, -31.00000000000002842 ) ) ;
#13661 = VERTEX_POINT ( 'NONE', #8451 ) ;
#13662 = CARTESIAN_POINT ( 'NONE',  ( -5.999999999999963585, -1.487416814333745711E-14, -165.8363248654052029 ) ) ;
#13663 = EDGE_CURVE ( 'NONE', #9581, #26206, #3905, .T. ) ;
#13664 = FACE_OUTER_BOUND ( 'NONE', #5310, .T. ) ;
#13665 = CARTESIAN_POINT ( 'NONE',  ( 4.763139720814407951, -2.749999999999988454, -173.0000000000000568 ) ) ;
#13666 = CARTESIAN_POINT ( 'NONE',  ( 139.7940636821621752, -8.829150386088183922, 8.127229673620972150 ) ) ;
#13667 = CARTESIAN_POINT ( 'NONE',  ( -6.350852961085760029, -1.281975124255709124E-13, -161.6250000000000284 ) ) ;
#13668 = CARTESIAN_POINT ( 'NONE',  ( 115.6874999999997584, -1.035533905932719101, -2.499999999999844569 ) ) ;
#13669 = CARTESIAN_POINT ( 'NONE',  ( 3.175426480543072749, 5.499999999999865885, -109.6249999999999716 ) ) ;
#13670 = CARTESIAN_POINT ( 'NONE',  ( 6.000000000000000888, -1.607695154586752384, -159.1533121635129646 ) ) ;
#13671 = CARTESIAN_POINT ( 'NONE',  ( -3.464101615137757051, -5.999999999999979572, -166.1636751345947687 ) ) ;
#13672 = CARTESIAN_POINT ( 'NONE',  ( 3.175426480543072749, -5.500000000000105693, -95.12500000000002842 ) ) ;
#13673 = CARTESIAN_POINT ( 'NONE',  ( 158.3586002691896510, 2.071067811865468400, 4.999999999999989342 ) ) ;
#13674 = CARTESIAN_POINT ( 'NONE',  ( 0.2071426722869369463, -15.61926834800564023, 7.893137763387031214 ) ) ;
#13675 = ORIENTED_EDGE ( 'NONE', *, *, #14028, .F. ) ;
#13676 = CARTESIAN_POINT ( 'NONE',  ( 11.81250000000017764, 1.097466725451679892, 2.649519052838238409 ) ) ;
#13677 = CARTESIAN_POINT ( 'NONE',  ( 118.1249999999999147, 1.767766952966320915, 1.767766952966431937 ) ) ;
#13678 = DIRECTION ( 'NONE',  ( 1.000000000000000000, -5.551115123125773458E-17, -1.260129944081490338E-35 ) ) ;
#13679 = CARTESIAN_POINT ( 'NONE',  ( 112.4377832217622455, 1.849990392679621953, 0.7662911109081291805 ) ) ;
#13680 = CARTESIAN_POINT ( 'NONE',  ( 23.91367513459499605, -1.767766952966154381, -1.767766952966542959 ) ) ;
#13681 = ORIENTED_EDGE ( 'NONE', *, *, #17566, .T. ) ;
#13682 = CARTESIAN_POINT ( 'NONE',  ( 12.96132486540529882, 1.110223024625156540E-13, 2.500000000000002220 ) ) ;
#13683 = CARTESIAN_POINT ( 'NONE',  ( 109.3122167782373566, -0.7662911109077388261, -1.849990392679351725 ) ) ;
#13684 = CARTESIAN_POINT ( 'NONE',  ( -5.412658773652684552, -3.125000000000099920, -86.06698729810780435 ) ) ;
#13685 = ADVANCED_BREP_SHAPE_REPRESENTATION ( '', ( #13969, #18805 ), #19755 ) ;
#13686 = EDGE_LOOP ( 'NONE', ( #22622, #30310, #11536, #13807 ) ) ;
#13687 = CARTESIAN_POINT ( 'NONE',  ( 106.8988248654050892, 0.8284271247462354770, 2.000000000000212275 ) ) ;
#13688 = CIRCLE ( 'NONE', #15136, 4.999999999999999112 ) ;
#13689 = SHAPE_REPRESENTATION ( 'Clamp rod', ( #18805 ), #1599 ) ;
#13690 = ORIENTED_EDGE ( 'NONE', *, *, #21327, .T. ) ;
#13691 = EDGE_LOOP ( 'NONE', ( #10669, #11729, #4733, #7972 ) ) ;
#13692 = CARTESIAN_POINT ( 'NONE',  ( 148.7812500000000284, 2.485281374238585972, 6.000000000000005329 ) ) ;
#13693 = ORIENTED_EDGE ( 'NONE', *, *, #15537, .T. ) ;
#13694 = EDGE_CURVE ( 'NONE', #1235, #152, #25243, .T. ) ;
#13695 = CARTESIAN_POINT ( 'NONE',  ( 4.763139720814407951, -2.749999999999988454, -122.0000000000000000 ) ) ;
#13696 = CARTESIAN_POINT ( 'NONE',  ( 22.31250000000008882, 2.649519052838478661, -1.097466725451499370 ) ) ;
#13697 = EDGE_CURVE ( 'NONE', #8975, #856, #12948, .T. ) ;
#13698 = CARTESIAN_POINT ( 'NONE',  ( 2.775557561562891351E-14, 6.250000000000033751, -127.9330127018922809 ) ) ;
#13699 = ORIENTED_EDGE ( 'NONE', *, *, #22857, .F. ) ;
#13700 = DIRECTION ( 'NONE',  ( -7.147005652999508048E-36, 5.642372883946980038E-36, 1.000000000000000000 ) ) ;
#13701 = CARTESIAN_POINT ( 'NONE',  ( 2.775557561562891351E-14, -6.250000000000061284, -171.3169872981078470 ) ) ;
#13702 = CARTESIAN_POINT ( 'NONE',  ( 7.216878364870455975, -6.409875621278545621E-14, -173.9419872981078470 ) ) ;
#13703 = ORIENTED_EDGE ( 'NONE', *, *, #15885, .T. ) ;
#13704 = CARTESIAN_POINT ( 'NONE',  ( -0.07769256095282929542, -15.23231281889968969, -7.500000000000007105 ) ) ;
#13705 = FACE_OUTER_BOUND ( 'NONE', #8494, .T. ) ;
#13706 = CARTESIAN_POINT ( 'NONE',  ( 0.000000000000000000, 0.000000000000000000, 0.000000000000000000 ) ) ;
#13707 = FACE_OUTER_BOUND ( 'NONE', #10212, .T. ) ;
#13708 = CARTESIAN_POINT ( 'NONE',  ( -40.00000000000000000, -20.00000000000021316, -3.000000000000002665 ) ) ;
#13709 = CARTESIAN_POINT ( 'NONE',  ( 112.9377832217622171, -1.849990392679381701, -0.7662911109076485650 ) ) ;
#13710 = CARTESIAN_POINT ( 'NONE',  ( 5.412658773652712085, -3.125000000000086153, -76.56698729810784698 ) ) ;
#13711 = CARTESIAN_POINT ( 'NONE',  ( 2.775557561562891351E-14, -6.250000000000061284, -60.31698729810780435 ) ) ;
#13712 = CARTESIAN_POINT ( 'NONE',  ( -3.608439182435052128, -6.250000000000110134, -181.3080127018922383 ) ) ;
#13713 = CARTESIAN_POINT ( 'NONE',  ( -0.6927266194436478841, -9.614546761112784168, -4.200333198739684804 ) ) ;
#13714 = CARTESIAN_POINT ( 'NONE',  ( 3.464101615137757051, -5.999999999999979572, -153.3363248654051745 ) ) ;
#13715 = LINE ( 'NONE', #5860, #4481 ) ;
#13716 = CARTESIAN_POINT ( 'NONE',  ( 3.175426480543072749, 5.499999999999865885, -118.6250000000000284 ) ) ;
#13717 = CARTESIAN_POINT ( 'NONE',  ( -6.350852961085760029, -1.281975124255709124E-13, -155.6249999999999716 ) ) ;
#13718 = CARTESIAN_POINT ( 'NONE',  ( -5.999999999999963585, -1.487416814333745711E-14, -137.9136751345947971 ) ) ;
#13719 = CARTESIAN_POINT ( 'NONE',  ( 154.2113248654052313, 5.500000000000005329, 0.000000000000000000 ) ) ;
#13720 = ORIENTED_EDGE ( 'NONE', *, *, #28341, .F. ) ;
#13721 = CARTESIAN_POINT ( 'NONE',  ( 19.81250000000015277, 1.097466725451679892, 2.649519052838298805 ) ) ;
#13722 = CARTESIAN_POINT ( 'NONE',  ( 5.999999999999949374, 1.607695154586804565, -123.0193375672974696 ) ) ;
#13723 = DIRECTION ( 'NONE',  ( -8.326672684688675286E-17, -2.081668171172168821E-17, 1.000000000000000000 ) ) ;
#13724 = CARTESIAN_POINT ( 'NONE',  ( 136.3273502691896510, -5.000000000000004441, 0.000000000000000000 ) ) ;
#13725 = EDGE_LOOP ( 'NONE', ( #9885, #7850, #8342, #23154 ) ) ;
#13726 = CARTESIAN_POINT ( 'NONE',  ( 108.4997167782375982, 1.308140751793668288, -1.308140751793418488 ) ) ;
#13727 = CARTESIAN_POINT ( 'NONE',  ( -5.196152422706601826, 2.999999999999975131, -121.5386751345948255 ) ) ;
#13728 = CARTESIAN_POINT ( 'NONE',  ( 113.0622167782374561, -1.849990392679532247, 0.7662911109078888172 ) ) ;
#13729 = CARTESIAN_POINT ( 'NONE',  ( 7.216878364870455975, -6.409875621278545621E-14, -113.9419872981078328 ) ) ;
#13730 = CARTESIAN_POINT ( 'NONE',  ( 17.21132486540530238, -2.499999999999891198, -1.110223024625156540E-13 ) ) ;
#13731 = CARTESIAN_POINT ( 'NONE',  ( 113.4613248654050182, 0.000000000000000000, -2.000000000000001776 ) ) ;
#13732 = ORIENTED_EDGE ( 'NONE', *, *, #15426, .T. ) ;
#13733 = CARTESIAN_POINT ( 'NONE',  ( -6.000000000000000888, 1.067854986875958443E-15, 7.560779664488942560E-35 ) ) ;
#13734 = CARTESIAN_POINT ( 'NONE',  ( 140.8125000000000284, 4.242640687119298093, -4.242640687119298093 ) ) ;
#13735 = ADVANCED_FACE ( 'NONE', ( #17697 ), #16019, .T. ) ;
#13736 = CARTESIAN_POINT ( 'NONE',  ( 2.775557561562891351E-14, -6.250000000000061284, -49.81698729810779724 ) ) ;
#13737 = CARTESIAN_POINT ( 'NONE',  ( 5.412658773652712085, -3.125000000000086153, -147.0669872981078470 ) ) ;
#13738 = FACE_OUTER_BOUND ( 'NONE', #17070, .T. ) ;
#13739 = SURFACE_STYLE_FILL_AREA ( #30277 ) ;
#13740 = CARTESIAN_POINT ( 'NONE',  ( 22.50000000000010303, -1.999999999999835243, 0.000000000000000000 ) ) ;
#13741 = CARTESIAN_POINT ( 'NONE',  ( -7.216878364870328078, 0.000000000000000000, -69.05801270189226670 ) ) ;
#13742 =( BOUNDED_CURVE ( )  B_SPLINE_CURVE ( 2, ( #395, #19163, #704, #2698, #7903, #26484, #21466, #17318, #7320 ),
 .UNSPECIFIED., .F., .T. ) 
 B_SPLINE_CURVE_WITH_KNOTS ( ( 3, 2, 2, 2, 3 ),
 ( 0.9583333333333332593, 0.9592592592592592560, 0.9611111111111111382, 0.9629629629629629095, 0.9638888888888889062 ),
 .UNSPECIFIED. ) 
 CURVE ( )  GEOMETRIC_REPRESENTATION_ITEM ( )  RATIONAL_B_SPLINE_CURVE ( ( 0.9330127018922194093, 0.9330127018922154125, 1.000000000000000000, 0.8660254037844388186, 1.000000000000000000, 0.8660254037844388186, 1.000000000000000000, 0.9330127018922154125, 0.9330127018922194093 ) ) 
 REPRESENTATION_ITEM ( '' )  );
#13743 = CARTESIAN_POINT ( 'NONE',  ( 143.6101497308104058, 3.535533905932725318, 3.535533905932725318 ) ) ;
#13744 = FACE_OUTER_BOUND ( 'NONE', #25887, .T. ) ;
#13745 = CARTESIAN_POINT ( 'NONE',  ( -3.464101615137725076, 5.999999999999979572, -73.66367513459483973 ) ) ;
#13746 = CARTESIAN_POINT ( 'NONE',  ( 5.999999999999999112, 2.951592740943527306E-14, -155.1636751345948539 ) ) ;
#13747 = DIRECTION ( 'NONE',  ( 0.000000000000000000, -0.000000000000000000, 1.000000000000000000 ) ) ;
#13748 = LINE ( 'NONE', #1874, #11135 ) ;
#13749 = CARTESIAN_POINT ( 'NONE',  ( 109.6874999999997868, -1.035533905932659149, -2.499999999999724221 ) ) ;
#13750 = CARTESIAN_POINT ( 'NONE',  ( 3.175426480543072749, -5.500000000000105693, -123.6250000000000426 ) ) ;
#13751 = MECHANICAL_DESIGN_GEOMETRIC_PRESENTATION_REPRESENTATION (  '', ( #924 ), #25958 ) ;
#13752 = DIRECTION ( 'NONE',  ( 1.000000000000000000, -0.000000000000000000, -0.000000000000000000 ) ) ;
#13753 = CARTESIAN_POINT ( 'NONE',  ( 5.196152422706629359, 3.000000000000002665, -143.0386751345948255 ) ) ;
#13754 = ORIENTED_EDGE ( 'NONE', *, *, #29061, .T. ) ;
#13755 = CARTESIAN_POINT ( 'NONE',  ( 3.175426480543072749, -5.500000000000105693, -51.62500000000002842 ) ) ;
#13756 = CARTESIAN_POINT ( 'NONE',  ( 0.000000000000000000, -5.999999999999991118, -154.9613248654052597 ) ) ;
#13757 = CARTESIAN_POINT ( 'NONE',  ( -5.999999999999963585, 1.780251999655701777E-13, -77.33632486540524553 ) ) ;
#13758 = ORIENTED_EDGE ( 'NONE', *, *, #18744, .T. ) ;
#13759 = CARTESIAN_POINT ( 'NONE',  ( 104.5624999999997442, -2.499999999999934719, -1.035533905932689347 ) ) ;
#13760 = CARTESIAN_POINT ( 'NONE',  ( 142.8750000000000284, 0.000000000000000000, 6.000000000000005329 ) ) ;
#13761 = EDGE_CURVE ( 'NONE', #16234, #29267, #1116, .T. ) ;
#13762 = CARTESIAN_POINT ( 'NONE',  ( -2.081668171172168020E-16, -5.204170427930420051E-17, 2.499999999999999112 ) ) ;
#13763 = CARTESIAN_POINT ( 'NONE',  ( 138.6562500000000568, -6.000000000000005329, 2.485281374238555774 ) ) ;
#13764 = CARTESIAN_POINT ( 'NONE',  ( 21.91367513459491079, -1.767766952966154381, -1.767766952966431937 ) ) ;
#13765 = ORIENTED_EDGE ( 'NONE', *, *, #10051, .T. ) ;
#13766 = AXIS2_PLACEMENT_3D ( 'NONE', #17235, #10006, #1203 ) ;
#13767 = CARTESIAN_POINT ( 'NONE',  ( -4.763139720814407951, 2.749999999999946709, -139.2499999999999716 ) ) ;
#13768 = EDGE_CURVE ( 'NONE', #13277, #2002, #7352, .T. ) ;
#13769 = VECTOR ( 'NONE', #18838, 1000.000000000000000 ) ;
#13770 = ORIENTED_EDGE ( 'NONE', *, *, #2712, .T. ) ;
#13771 = CARTESIAN_POINT ( 'NONE',  ( 15.12500000000000000, 1.414213562373201061, 1.414213562373034527 ) ) ;
#13772 = ORIENTED_EDGE ( 'NONE', *, *, #27082, .F. ) ;
#13773 = VECTOR ( 'NONE', #25975, 1000.000000000000000 ) ;
#13774 = CARTESIAN_POINT ( 'NONE',  ( -6.350852961085760029, -1.281975124255709124E-13, -67.12500000000002842 ) ) ;
#13775 = CARTESIAN_POINT ( 'NONE',  ( 18.52382486540528461, 1.035533905932869425, -2.499999999999904521 ) ) ;
#13776 = CARTESIAN_POINT ( 'NONE',  ( -3.608439182435115633, 6.249999999999965361, -87.30801270189223828 ) ) ;
#13777 = CARTESIAN_POINT ( 'NONE',  ( 10.12500000000007816, 1.414213562373201061, 1.414213562373145550 ) ) ;
#13778 = EDGE_LOOP ( 'NONE', ( #27227, #11341, #10758, #26515 ) ) ;
#13779 = CARTESIAN_POINT ( 'NONE',  ( 154.5074251345949108, 2.278174593052074925, -5.499999999999950262 ) ) ;
#13780 = DIRECTION ( 'NONE',  ( 0.000000000000000000, 0.000000000000000000, -1.000000000000000000 ) ) ;
#13781 = CARTESIAN_POINT ( 'NONE',  ( 119.6877832217621176, -0.7662911109077686911, 1.849990392679532247 ) ) ;
#13782 = SHAPE_DEFINITION_REPRESENTATION ( #3750, #1893 ) ;
#13783 = CARTESIAN_POINT ( 'NONE',  ( 4.763139720814407951, 2.750000000000002665, -150.2500000000000000 ) ) ;
#13784 = CARTESIAN_POINT ( 'NONE',  ( 140.0000000000000284, -9.819569584722252387, -7.620286941409521120 ) ) ;
#13785 = CARTESIAN_POINT ( 'NONE',  ( 0.000000000000000000, 5.499999999999991118, -142.5000000000000284 ) ) ;
#13786 = CARTESIAN_POINT ( 'NONE',  ( -3.608439182435052128, -6.250000000000110134, -160.3080127018922383 ) ) ;
#13787 = CARTESIAN_POINT ( 'NONE',  ( -5.999999999999963585, -1.487416814333745711E-14, -123.8363248654052171 ) ) ;
#13788 = STYLED_ITEM ( 'NONE', ( #24968 ), #26910 ) ;
#13789 = CARTESIAN_POINT ( 'NONE',  ( 3.175426480543072749, -5.500000000000105693, -78.62500000000001421 ) ) ;
#13790 = CARTESIAN_POINT ( 'NONE',  ( 116.7738248654050892, 2.000000000000061728, 0.8284271247462955401 ) ) ;
#13791 = CARTESIAN_POINT ( 'NONE',  ( 3.175426480543072749, 5.499999999999865885, -72.12500000000005684 ) ) ;
#13792 = CARTESIAN_POINT ( 'NONE',  ( -5.999999999999963585, 8.134310703387671600E-14, -120.8363248654052171 ) ) ;
#13793 = CARTESIAN_POINT ( 'NONE',  ( 150.5773502691896510, 5.000000000000004441, 0.000000000000000000 ) ) ;
#13794 = CARTESIAN_POINT ( 'NONE',  ( 10.96132486540515849, 1.110223024625156540E-13, 2.499999999999835687 ) ) ;
#13795 = CARTESIAN_POINT ( 'NONE',  ( -4.999999999999886313, -10.50000000000000888, 8.000000000000007105 ) ) ;
#13796 = EDGE_CURVE ( 'NONE', #25418, #28105, #13557, .T. ) ;
#13797 = CARTESIAN_POINT ( 'NONE',  ( 157.5000000000000284, 6.000000000000005329, 0.000000000000000000 ) ) ;
#13798 = CARTESIAN_POINT ( 'NONE',  ( 20.18750000000014566, 0.8284271247463557142, 1.999999999999911626 ) ) ;
#13799 = EDGE_CURVE ( 'NONE', #19518, #12143, #2317, .T. ) ;
#13800 = CARTESIAN_POINT ( 'NONE',  ( 6.000000000000000888, 7.762456499804234384E-14, -119.1636751345948113 ) ) ;
#13801 = CARTESIAN_POINT ( 'NONE',  ( 6.000000000000000888, -1.859271017917181981E-14, -170.1636751345948539 ) ) ;
#13802 = ORIENTED_EDGE ( 'NONE', *, *, #17887, .F. ) ;
#13803 = CARTESIAN_POINT ( 'NONE',  ( 158.6250000000000568, 0.000000000000000000, -6.000000000000005329 ) ) ;
#13804 = CARTESIAN_POINT ( 'NONE',  ( -20.99999999999998224, -25.00000000000010658, -4.000000000000003553 ) ) ;
#13805 = CARTESIAN_POINT ( 'NONE',  ( 114.6877832217621318, -0.7662911109077987781, 1.849990392679591977 ) ) ;
#13806 = CARTESIAN_POINT ( 'NONE',  ( 5.999999999999949374, 1.607695154586804565, -157.5193375672974128 ) ) ;
#13807 = ORIENTED_EDGE ( 'NONE', *, *, #29482, .F. ) ;
#13808 = ORIENTED_EDGE ( 'NONE', *, *, #9688, .F. ) ;
#13809 = ADVANCED_FACE ( 'NONE', ( #22093 ), #3035, .T. ) ;
#13810 = ORIENTED_EDGE ( 'NONE', *, *, #12576, .T. ) ;
#13811 = CARTESIAN_POINT ( 'NONE',  ( -3.175426480542816510, -5.500000000000057732, -90.87500000000001421 ) ) ;
#13812 = CIRCLE ( 'NONE', #29445, 17.50000000000004619 ) ;
#13813 = CARTESIAN_POINT ( 'NONE',  ( -5.412658773652739619, 3.124999999999975131, -108.1830127018922383 ) ) ;
#13814 = VERTEX_POINT ( 'NONE', #7944 ) ;
#13815 = FACE_OUTER_BOUND ( 'NONE', #5674, .T. ) ;
#13816 = MECHANICAL_DESIGN_GEOMETRIC_PRESENTATION_REPRESENTATION (  '', ( #14778 ), #7398 ) ;
#13817 = CARTESIAN_POINT ( 'NONE',  ( -3.175426480542816510, -5.500000000000057732, -164.3750000000000568 ) ) ;
#13818 = CARTESIAN_POINT ( 'NONE',  ( 4.758024543289591790, -9.918640242984132271, -28.66037974350899376 ) ) ;
#13819 = ORIENTED_EDGE ( 'NONE', *, *, #23392, .T. ) ;
#13820 = CARTESIAN_POINT ( 'NONE',  ( 6.000000000000000888, -1.859271017917181981E-14, -47.16367513459483263 ) ) ;
#13821 = CIRCLE ( 'NONE', #519, 1.000000000000000000 ) ;
#13822 = CARTESIAN_POINT ( 'NONE',  ( 6.350852961086080661, -9.614813431917819062E-14, -172.8750000000000284 ) ) ;
#13823 = LINE ( 'NONE', #27888, #7149 ) ;
#13824 = CARTESIAN_POINT ( 'NONE',  ( -3.175426480542816510, 5.499999999999865885, -166.3750000000000568 ) ) ;
#13825 = CARTESIAN_POINT ( 'NONE',  ( 117.9999999999997868, 2.500000000000002220, 2.220446049250313081E-13 ) ) ;
#13826 = CARTESIAN_POINT ( 'NONE',  ( -3.175426480542816066, 5.499999999999865885, -100.3749999999999858 ) ) ;
#13827 = FACE_OUTER_BOUND ( 'NONE', #26135, .T. ) ;
#13828 =( BOUNDED_CURVE ( )  B_SPLINE_CURVE ( 2, ( #12575, #24061, #851, #9947, #715, #9794, #28357, #7332, #26205 ),
 .UNSPECIFIED., .F., .T. ) 
 B_SPLINE_CURVE_WITH_KNOTS ( ( 3, 2, 2, 2, 3 ),
 ( 0.4411764705882352811, 0.4485294117647058987, 0.4558823529411764608, 0.4632352941176470784, 0.4705882352941176405 ),
 .UNSPECIFIED. ) 
 CURVE ( )  GEOMETRIC_REPRESENTATION_ITEM ( )  RATIONAL_B_SPLINE_CURVE ( ( 1.000000000000000000, 0.9238795325112867385, 1.000000000000000000, 0.9238795325112867385, 1.000000000000000000, 0.9238795325112867385, 1.000000000000000000, 0.9238795325112867385, 1.000000000000000000 ) ) 
 REPRESENTATION_ITEM ( '' )  );
#13829 = CARTESIAN_POINT ( 'NONE',  ( 3.175426480543072749, 5.499999999999865885, -99.12500000000005684 ) ) ;
#13830 = CARTESIAN_POINT ( 'NONE',  ( 158.9211002691896795, -4.999999999999989342, -2.071067811865468400 ) ) ;
#13831 = CARTESIAN_POINT ( 'NONE',  ( -0.07769256095284231278, -15.23231281889969857, 7.499999999999993783 ) ) ;
#13832 = ORIENTED_EDGE ( 'NONE', *, *, #13476, .F. ) ;
#13833 = CARTESIAN_POINT ( 'NONE',  ( 12.06250000000005507, -2.649519052838238409, 1.097466725451619718 ) ) ;
#13834 = CARTESIAN_POINT ( 'NONE',  ( 116.4374999999997726, -2.499999999999934719, 1.035533905932929599 ) ) ;
#13835 = EDGE_CURVE ( 'NONE', #20658, #28850, #26422, .T. ) ;
#13836 = CARTESIAN_POINT ( 'NONE',  ( 15.97617513459489125, -1.035533905932629173, -2.499999999999964473 ) ) ;
#13837 = CONICAL_SURFACE ( 'NONE', #29470, 577.3502691896271699, 0.5235987755982998149 ) ;
#13838 = CARTESIAN_POINT ( 'NONE',  ( 107.1252832217622455, 0.000000000000000000, -1.849990392679523588 ) ) ;
#13839 = CARTESIAN_POINT ( 'NONE',  ( 23.72617513459496053, -2.499999999999904521, 1.035533905932749299 ) ) ;
#13840 =( BOUNDED_CURVE ( )  B_SPLINE_CURVE ( 2, ( #28280, #20947, #18504, #7257, #27827, #5383, #28722, #14936, #9725 ),
 .UNSPECIFIED., .F., .T. ) 
 B_SPLINE_CURVE_WITH_KNOTS ( ( 3, 2, 2, 2, 3 ),
 ( 0.8694444444444444642, 0.8703703703703703498, 0.8722222222222222321, 0.8740740740740741144, 0.8750000000000000000 ),
 .UNSPECIFIED. ) 
 CURVE ( )  GEOMETRIC_REPRESENTATION_ITEM ( )  RATIONAL_B_SPLINE_CURVE ( ( 0.9330127018922194093, 0.9330127018922234061, 1.000000000000000000, 0.8660254037844388186, 1.000000000000000000, 0.8660254037844388186, 1.000000000000000000, 0.9330127018922194093, 0.9330127018922194093 ) ) 
 REPRESENTATION_ITEM ( '' )  );
#13841 = VERTEX_POINT ( 'NONE', #14740 ) ;
#13842 = CARTESIAN_POINT ( 'NONE',  ( 6.000000000000000888, 1.743066579297358182E-13, -112.5863248654052029 ) ) ;
#13843 = AXIS2_PLACEMENT_3D ( 'NONE', #30068, #20560, #17978 ) ;
#13844 = ORIENTED_EDGE ( 'NONE', *, *, #17707, .F. ) ;
#13845 = ADVANCED_FACE ( 'NONE', ( #5030 ), #16907, .T. ) ;
#13846 = LINE ( 'NONE', #20875, #12578 ) ;
#13847 = EDGE_CURVE ( 'NONE', #30104, #13277, #11825, .T. ) ;
#13848 =( GEOMETRIC_REPRESENTATION_CONTEXT ( 3 ) GLOBAL_UNCERTAINTY_ASSIGNED_CONTEXT ( ( #7178 ) ) GLOBAL_UNIT_ASSIGNED_CONTEXT ( ( #3707, #5858, #12824 ) ) REPRESENTATION_CONTEXT ( 'NONE', 'WORKASPACE' ) );
#13849 = ORIENTED_EDGE ( 'NONE', *, *, #18882, .F. ) ;
#13850 = CARTESIAN_POINT ( 'NONE',  ( 147.7500000000000284, -6.000000000000005329, 0.000000000000000000 ) ) ;
#13851 = ORIENTED_EDGE ( 'NONE', *, *, #17911, .T. ) ;
#13852 = CARTESIAN_POINT ( 'NONE',  ( -3.175426480542816510, 5.499999999999865885, -113.8750000000000000 ) ) ;
#13853 = CARTESIAN_POINT ( 'NONE',  ( 21.81250000000006395, -2.649519052838238409, 1.097466725451499370 ) ) ;
#13854 = CARTESIAN_POINT ( 'NONE',  ( -3.608439182435115633, 6.249999999999965361, -127.8080127018922383 ) ) ;
#13855 = ORIENTED_EDGE ( 'NONE', *, *, #2331, .T. ) ;
#13856 = CARTESIAN_POINT ( 'NONE',  ( 2.775557561562891351E-14, 6.250000000000033751, -170.5669872981078186 ) ) ;
#13857 = CARTESIAN_POINT ( 'NONE',  ( 3.608439182435180470, -6.249999999999997335, -175.6919872981078186 ) ) ;
#13858 = CARTESIAN_POINT ( 'NONE',  ( 159.9741911234880547, -12.51693588432441651, 3.259847203776756075 ) ) ;
#13859 = AXIS2_PLACEMENT_3D ( 'NONE', #15707, #22740, #17852 ) ;
#13860 = CARTESIAN_POINT ( 'NONE',  ( 11.06250000000006928, 2.000000000000091926, 0.8284271247461753029 ) ) ;
#13861 = SURFACE_STYLE_FILL_AREA ( #14695 ) ;
#13862 = CARTESIAN_POINT ( 'NONE',  ( 109.2886751345947971, 2.000000000000057288, 1.110223024625156540E-13 ) ) ;
#13863 = CARTESIAN_POINT ( 'NONE',  ( -5.999999999999963585, 8.134310703387671600E-14, -136.4136751345948255 ) ) ;
#13864 = AXIS2_PLACEMENT_3D ( 'NONE', #16629, #23808, #26244 ) ;
#13865 = CARTESIAN_POINT ( 'NONE',  ( 0.000000000000000000, -5.999999999999991118, -150.4613248654052029 ) ) ;
#13866 = CARTESIAN_POINT ( 'NONE',  ( 111.6252832217622739, 0.000000000000000000, 1.849990392679523588 ) ) ;
#13867 = CARTESIAN_POINT ( 'NONE',  ( -3.608439182435115633, 6.249999999999965361, -77.44198729810777593 ) ) ;
#13868 = CARTESIAN_POINT ( 'NONE',  ( -3.608439182435052128, -6.250000000000110134, -61.94198729810783277 ) ) ;
#13869 = CARTESIAN_POINT ( 'NONE',  ( 3.175426480543072749, 5.499999999999865885, -48.12500000000000000 ) ) ;
#13870 = CARTESIAN_POINT ( 'NONE',  ( 6.000000000000000888, 1.743066579297358182E-13, -111.0863248654051887 ) ) ;
#13871 = CARTESIAN_POINT ( 'NONE',  ( 3.464101615137757051, -5.999999999999979572, -47.41367513459483973 ) ) ;
#13872 = DIRECTION ( 'NONE',  ( 1.000000000000000000, 0.000000000000000000, -0.000000000000000000 ) ) ;
#13873 = CARTESIAN_POINT ( 'NONE',  ( -3.175426480542816510, -5.500000000000057732, -125.3749999999999858 ) ) ;
#13874 = CARTESIAN_POINT ( 'NONE',  ( 135.0000000000000284, -8.132376923925228596, -7.784896983692046746 ) ) ;
#13875 = CARTESIAN_POINT ( 'NONE',  ( -2.910268709469104432E-14, -11.00000000000000000, -14.99152654425661702 ) ) ;
#13876 = VERTEX_POINT ( 'NONE', #12159 ) ;
#13877 = CARTESIAN_POINT ( 'NONE',  ( 19.43749999999998224, 1.097466725451559322, -2.649519052838298805 ) ) ;
#13878 = EDGE_CURVE ( 'NONE', #13234, #26278, #29568, .T. ) ;
#13879 = CARTESIAN_POINT ( 'NONE',  ( 143.9136751345948539, 0.000000000000000000, -5.500000000000005329 ) ) ;
#13880 = DIRECTION ( 'NONE',  ( 0.000000000000000000, -1.000000000000000000, 0.000000000000000000 ) ) ;
#13881 = ORIENTED_EDGE ( 'NONE', *, *, #7847, .T. ) ;
#13882 = AXIS2_PLACEMENT_3D ( 'NONE', #1918, #29713, #6681 ) ;
#13883 = CARTESIAN_POINT ( 'NONE',  ( 108.7497167782375982, 1.308140751793696044, 1.308140751793640533 ) ) ;
#13884 = CARTESIAN_POINT ( 'NONE',  ( 0.000000000000000000, 0.000000000000000000, 0.000000000000000000 ) ) ;
#13885 = CARTESIAN_POINT ( 'NONE',  ( 112.0622167782374277, -1.849990392679472073, 0.7662911109078888172 ) ) ;
#13886 =( BOUNDED_CURVE ( )  B_SPLINE_CURVE ( 2, ( #21831, #2920, #2627, #910, #28562, #10308, #10159, #7530, #19673 ),
 .UNSPECIFIED., .F., .F. ) 
 B_SPLINE_CURVE_WITH_KNOTS ( ( 3, 2, 2, 2, 3 ),
 ( 0.7875000000000001998, 0.7937500000000005107, 0.8000000000000008216, 0.8062500000000010214, 0.8125000000000013323 ),
 .UNSPECIFIED. ) 
 CURVE ( )  GEOMETRIC_REPRESENTATION_ITEM ( )  RATIONAL_B_SPLINE_CURVE ( ( 0.9999999999999973355, 0.9238795325112894030, 1.000000000000000000, 0.9238795325112867385, 1.000000000000000000, 0.9238795325112867385, 1.000000000000000000, 0.9238795325112705292, 1.000000000000016209 ) ) 
 REPRESENTATION_ITEM ( '' )  );
#13887 = CARTESIAN_POINT ( 'NONE',  ( 2.775557561562891351E-14, -6.250000000000061284, -109.8169872981078470 ) ) ;
#13888 = VECTOR ( 'NONE', #1411, 1000.000000000000000 ) ;
#13889 = CARTESIAN_POINT ( 'NONE',  ( 22.27382486540526330, -2.499999999999904521, -1.035533905932749299 ) ) ;
#13890 = EDGE_CURVE ( 'NONE', #30108, #15655, #24084, .T. ) ;
#13891 = CARTESIAN_POINT ( 'NONE',  ( 10.00000000000014744, 1.031164828675704914, 2.068637288563754062 ) ) ;
#13892 = ORIENTED_EDGE ( 'NONE', *, *, #24669, .F. ) ;
#13893 = CARTESIAN_POINT ( 'NONE',  ( 5.196152422706629359, 3.000000000000002665, -141.5386751345948255 ) ) ;
#13894 = CARTESIAN_POINT ( 'NONE',  ( 134.0625000000000284, -4.242640687119298093, 4.242640687119298093 ) ) ;
#13895 = CARTESIAN_POINT ( 'NONE',  ( -7.216878364870328078, 0.000000000000000000, -138.6919872981077901 ) ) ;
#13896 = CIRCLE ( 'NONE', #6977, 10.00000000000001421 ) ;
#13897 = DIRECTION ( 'NONE',  ( 0.000000000000000000, 0.000000000000000000, -1.000000000000000000 ) ) ;
#13898 = PRODUCT_DEFINITION_SHAPE ( 'NONE', 'NONE',  #10482 ) ;
#13899 = CARTESIAN_POINT ( 'NONE',  ( 21.06250000000004619, 2.000000000000151879, 0.8284271247461152399 ) ) ;
#13900 = FILL_AREA_STYLE_COLOUR ( '', #24466 ) ;
#13901 = CARTESIAN_POINT ( 'NONE',  ( 7.216878364870455975, -6.409875621278545621E-14, -66.80801270189228092 ) ) ;
#13902 = CARTESIAN_POINT ( 'NONE',  ( 141.2663997308104058, -4.999999999999989342, -2.071067811865468400 ) ) ;
#13903 = CARTESIAN_POINT ( 'NONE',  ( 11.91367513459487526, -1.767766952966154381, -1.767766952966542959 ) ) ;
#13904 = CARTESIAN_POINT ( 'NONE',  ( -5.196152422706573404, -3.000000000000002665, -70.28867513459479710 ) ) ;
#13905 = CARTESIAN_POINT ( 'NONE',  ( 6.000000000000000888, -3.330669073875464691E-16, -7.560779664488942560E-35 ) ) ;
#13906 = CARTESIAN_POINT ( 'NONE',  ( 24.68421870695930309, -2.320578051741148062, -0.02763398118663714514 ) ) ;
#13907 = CARTESIAN_POINT ( 'NONE',  ( 6.000000000000000888, 1.743066579297358182E-13, -66.66367513459481131 ) ) ;
#13908 = CARTESIAN_POINT ( 'NONE',  ( 108.6874999999998010, -1.035533905932749299, -2.499999999999844569 ) ) ;
#13909 = CARTESIAN_POINT ( 'NONE',  ( 0.000000000000000000, 5.499999999999991118, -121.5000000000000568 ) ) ;
#13910 = CARTESIAN_POINT ( 'NONE',  ( -7.216878364870328078, 0.000000000000000000, -145.5580127018922667 ) ) ;
#13911 = SURFACE_SIDE_STYLE ('',( #18649 ) ) ;
#13912 = ORIENTED_EDGE ( 'NONE', *, *, #1538, .F. ) ;
#13913 = EDGE_CURVE ( 'NONE', #11180, #14866, #618, .T. ) ;
#13914 = CARTESIAN_POINT ( 'NONE',  ( -3.175426480542816066, -5.500000000000057732, -56.37500000000004263 ) ) ;
#13915 = CARTESIAN_POINT ( 'NONE',  ( -5.999999999999963585, -1.487416814333745711E-14, -133.4136751345948255 ) ) ;
#13916 = EDGE_CURVE ( 'NONE', #6411, #22196, #4268, .T. ) ;
#13917 = DIRECTION ( 'NONE',  ( 1.000000000000000000, -0.000000000000000000, -0.000000000000000000 ) ) ;
#13918 = ORIENTED_EDGE ( 'NONE', *, *, #21545, .T. ) ;
#13919 = CARTESIAN_POINT ( 'NONE',  ( 120.1247167782375698, -1.849990392679523588, 0.000000000000000000 ) ) ;
#13920 = CARTESIAN_POINT ( 'NONE',  ( 138.2812500000000284, 2.485281374238585972, 6.000000000000005329 ) ) ;
#13921 = CARTESIAN_POINT ( 'NONE',  ( 2.775557561562891351E-14, -6.250000000000061284, -105.3169872981078470 ) ) ;
#13922 = LINE ( 'NONE', #14078, #13179 ) ;
#13923 = CARTESIAN_POINT ( 'NONE',  ( 132.0937500000000568, 6.000000000000005329, 2.485281374238585972 ) ) ;
#13924 = FACE_OUTER_BOUND ( 'NONE', #8666, .T. ) ;
#13925 = B_SPLINE_CURVE_WITH_KNOTS ( 'NONE', 2,
 ( #13875, #6758, #16027 ),
 .UNSPECIFIED., .F., .F.,
 ( 3, 3 ),
 ( 0.000000000000000000, 1.000000000000000000 ),
 .UNSPECIFIED. ) ;
#13926 = CARTESIAN_POINT ( 'NONE',  ( 6.350852961086080661, -9.614813431917819062E-14, -136.8750000000000568 ) ) ;
#13927 =( BOUNDED_CURVE ( )  B_SPLINE_CURVE ( 2, ( #6335, #24614, #5870, #26906, #10677, #13154, #26749, #8656, #20333 ),
 .UNSPECIFIED., .F., .F. ) 
 B_SPLINE_CURVE_WITH_KNOTS ( ( 3, 2, 2, 2, 3 ),
 ( 0.3124999999999988898, 0.3187499999999990896, 0.3249999999999992895, 0.3312499999999996558, 0.3374999999999998557 ),
 .UNSPECIFIED. ) 
 CURVE ( )  GEOMETRIC_REPRESENTATION_ITEM ( )  RATIONAL_B_SPLINE_CURVE ( ( 1.000000000000013545, 0.9238795325112731938, 1.000000000000000000, 0.9238795325112867385, 1.000000000000000000, 0.9238795325112867385, 1.000000000000000000, 0.9238795325112887369, 0.9999999999999980016 ) ) 
 REPRESENTATION_ITEM ( '' )  );
#13928 = VECTOR ( 'NONE', #25578, 1000.000000000000000 ) ;
#13929 = CARTESIAN_POINT ( 'NONE',  ( 11.37500000000010658, -1.414213562372979016, 1.414213562372979016 ) ) ;
#13930 = ORIENTED_EDGE ( 'NONE', *, *, #24287, .T. ) ;
#13931 = CARTESIAN_POINT ( 'NONE',  ( 4.763139720814407951, -2.749999999999988454, -68.00000000000000000 ) ) ;
#13932 = CARTESIAN_POINT ( 'NONE',  ( 156.6636751345948255, 0.000000000000000000, 5.500000000000005329 ) ) ;
#13933 = CARTESIAN_POINT ( 'NONE',  ( -6.000000000000023093, 1.607695154586625819, -140.4033121635129930 ) ) ;
#13934 = CARTESIAN_POINT ( 'NONE',  ( 5.412658773652739619, 3.124999999999988898, -89.18301270189220986 ) ) ;
#13935 = AXIS2_PLACEMENT_3D ( 'NONE', #6552, #2108, #20542 ) ;
#13936 = CARTESIAN_POINT ( 'NONE',  ( 119.7113248654050750, 2.000000000000001776, 1.110223024625156540E-13 ) ) ;
#13937 = CARTESIAN_POINT ( 'NONE',  ( 104.7497167782376408, 1.308140751793640533, 1.308140751793640533 ) ) ;
#13938 = DIRECTION ( 'NONE',  ( -7.147005652999508048E-36, 5.642372883946980038E-36, 1.000000000000000000 ) ) ;
#13939 = CARTESIAN_POINT ( 'NONE',  ( 117.6877832217621034, -0.7662911109077388261, 1.849990392679712103 ) ) ;
#13940 = CARTESIAN_POINT ( 'NONE',  ( 3.175426480543072749, 5.499999999999865885, -150.1250000000000284 ) ) ;
#13941 = CARTESIAN_POINT ( 'NONE',  ( 140.0570668326235193, -8.936721004324988726, -8.008823461752308859 ) ) ;
#13942 = CARTESIAN_POINT ( 'NONE',  ( -4.763139720814407951, -2.750000000000016431, -139.0000000000000000 ) ) ;
#13943 = CARTESIAN_POINT ( 'NONE',  ( -3.608439182435052128, -6.250000000000110134, -157.3080127018922383 ) ) ;
#13944 = CARTESIAN_POINT ( 'NONE',  ( -9.999999999999779732, -89.00000000000001421, -3.000000000000002665 ) ) ;
#13945 = CARTESIAN_POINT ( 'NONE',  ( 105.2113248654051745, -1.999999999999974021, 0.000000000000000000 ) ) ;
#13946 = CARTESIAN_POINT ( 'NONE',  ( 4.763139720814407951, -2.749999999999988454, -81.50000000000001421 ) ) ;
#13947 = DIRECTION ( 'NONE',  ( -7.147005652999508048E-36, 5.642372883946980038E-36, 1.000000000000000000 ) ) ;
#13948 = CARTESIAN_POINT ( 'NONE',  ( -6.350852961085760029, -1.281975124255709124E-13, -71.62500000000005684 ) ) ;
#13949 = EDGE_CURVE ( 'NONE', #13349, #11180, #1709, .T. ) ;
#13950 = AXIS2_PLACEMENT_3D ( 'NONE', #19688, #12801, #29028 ) ;
#13951 = CARTESIAN_POINT ( 'NONE',  ( 139.8143194369503703, -9.354716546993699922, 7.895755101431983114 ) ) ;
#13952 = CARTESIAN_POINT ( 'NONE',  ( 149.9211002691896226, -4.999999999999989342, -2.071067811865468400 ) ) ;
#13953 = CARTESIAN_POINT ( 'NONE',  ( 6.000000000000000888, -1.859271017917181981E-14, -114.0863248654052029 ) ) ;
#13954 = CARTESIAN_POINT ( 'NONE',  ( -5.999999999999963585, -1.487416814333745711E-14, -124.4136751345948255 ) ) ;
#13955 = CARTESIAN_POINT ( 'NONE',  ( 159.3750000000000568, 0.000000000000000000, 6.000000000000005329 ) ) ;
#13956 = CARTESIAN_POINT ( 'NONE',  ( 3.464101615137852974, 5.999999999999884537, -133.9136751345947971 ) ) ;
#13957 = CARTESIAN_POINT ( 'NONE',  ( 19.87500000000017053, 1.414213562373312083, -1.414213562373145550 ) ) ;
#13958 = CARTESIAN_POINT ( 'NONE',  ( -5.999999999999963585, 1.780251999655701777E-13, -94.41367513459482552 ) ) ;
#13959 = DIRECTION ( 'NONE',  ( -1.000000000000000000, -1.665334536937731113E-16, 1.526556658859586792E-16 ) ) ;
#13960 = SURFACE_SIDE_STYLE ('',( #25581 ) ) ;
#13961 = ORIENTED_EDGE ( 'NONE', *, *, #12845, .T. ) ;
#13962 = CARTESIAN_POINT ( 'NONE',  ( 155.2500000000000284, -6.000000000000005329, 0.000000000000000000 ) ) ;
#13963 =( NAMED_UNIT ( * ) PLANE_ANGLE_UNIT ( ) SI_UNIT ( $, .RADIAN. ) );
#13964 = CARTESIAN_POINT ( 'NONE',  ( 114.5627832217621602, 0.7662911109078588412, 1.849990392679712103 ) ) ;
#13965 = CARTESIAN_POINT ( 'NONE',  ( 0.000000000000000000, 5.999999999999977796, -179.7113248654052029 ) ) ;
#13966 = VERTEX_POINT ( 'NONE', #5938 ) ;
#13967 = ORIENTED_EDGE ( 'NONE', *, *, #19213, .F. ) ;
#13968 = ORIENTED_EDGE ( 'NONE', *, *, #10567, .F. ) ;
#13969 = MANIFOLD_SOLID_BREP ( 'Cut-Sweep1', #28141 ) ;
#13970 = CARTESIAN_POINT ( 'NONE',  ( 3.175426480543072749, -5.500000000000105693, -92.12500000000001421 ) ) ;
#13971 = CARTESIAN_POINT ( 'NONE',  ( 7.216878364870455975, -6.409875621278545621E-14, -104.3080127018922525 ) ) ;
#13972 = LINE ( 'NONE', #28182, #11 ) ;
#13973 = DIRECTION ( 'NONE',  ( 1.000000000000000000, 9.251858538542971828E-16, 0.000000000000000000 ) ) ;
#13974 = EDGE_CURVE ( 'NONE', #28542, #20142, #25074, .T. ) ;
#13975 =( BOUNDED_CURVE ( )  B_SPLINE_CURVE ( 3, ( #21416, #2070, #19118, #14091 ),
 .UNSPECIFIED., .F., .F. ) 
 B_SPLINE_CURVE_WITH_KNOTS ( ( 4, 4 ),
 ( 1.570796326794896558, 3.141592653589793116 ),
 .UNSPECIFIED. ) 
 CURVE ( )  GEOMETRIC_REPRESENTATION_ITEM ( )  RATIONAL_B_SPLINE_CURVE ( ( 1.000000000000000000, 0.8047378541243649375, 0.8047378541243649375, 1.000000000000000000 ) ) 
 REPRESENTATION_ITEM ( '' )  );
#13976 = CARTESIAN_POINT ( 'NONE',  ( 4.874391507318805772, -9.861790235658062898, -28.50395189876375213 ) ) ;
#13977 = ORIENTED_EDGE ( 'NONE', *, *, #24803, .T. ) ;
#13978 = CARTESIAN_POINT ( 'NONE',  ( 136.0000000000000284, -8.946933499675676416, 8.000000000000007105 ) ) ;
#13979 =( LENGTH_UNIT ( ) NAMED_UNIT ( * ) SI_UNIT ( .MILLI., .METRE. ) );
#13980 = CARTESIAN_POINT ( 'NONE',  ( 4.763139720814407951, 2.750000000000002665, -168.2500000000000000 ) ) ;
#13981 = CARTESIAN_POINT ( 'NONE',  ( -5.196152422706573404, -3.000000000000002665, -80.78867513459486815 ) ) ;
#13982 = CARTESIAN_POINT ( 'NONE',  ( -4.763139720814407951, -2.750000000000016431, -164.5000000000000284 ) ) ;
#13983 = CARTESIAN_POINT ( 'NONE',  ( 112.3124999999997726, -1.035533905932598975, 2.500000000000265121 ) ) ;
#13984 = CARTESIAN_POINT ( 'NONE',  ( 6.350852961086080661, -9.614813431917819062E-14, -99.37499999999998579 ) ) ;
#13985 = CARTESIAN_POINT ( 'NONE',  ( 0.000000000000000000, 0.000000000000000000, 0.000000000000000000 ) ) ;
#13986 = CARTESIAN_POINT ( 'NONE',  ( -5.999999999999963585, -1.487416814333745711E-14, -137.9136751345947971 ) ) ;
#13987 = CARTESIAN_POINT ( 'NONE',  ( -3.175426480542816510, -5.500000000000057732, -96.87499999999997158 ) ) ;
#13988 = EDGE_CURVE ( 'NONE', #8626, #5164, #16696, .T. ) ;
#13989 = CARTESIAN_POINT ( 'NONE',  ( 161.0000000000000284, -12.64911064067353408, -3.000000000000002665 ) ) ;
#13990 = CARTESIAN_POINT ( 'NONE',  ( 158.7336002691896510, -4.999999999999989342, 2.071067811865468400 ) ) ;
#13991 = CARTESIAN_POINT ( 'NONE',  ( 134.9999999999997158, -7.147106270679951301, 8.399947834374497546 ) ) ;
#13992 = EDGE_LOOP ( 'NONE', ( #15890, #3999, #26253, #25813 ) ) ;
#13993 = CARTESIAN_POINT ( 'NONE',  ( 10.74999999999998224, 1.873492889145123019, 1.873492889144734441 ) ) ;
#13994 = CARTESIAN_POINT ( 'NONE',  ( 112.4999999999999147, -2.499999999999835687, 0.000000000000000000 ) ) ;
#13995 = CARTESIAN_POINT ( 'NONE',  ( 16.03867513459497474, 5.551115123125782702E-14, -2.500000000000057732 ) ) ;
#13996 = CARTESIAN_POINT ( 'NONE',  ( 107.8127832217621318, -1.849990392679472073, 0.7662911109079489913 ) ) ;
#13997 = CARTESIAN_POINT ( 'NONE',  ( 125.0000000000000568, -55.00000000000000711, -5.000000000000004441 ) ) ;
#13998 = ORIENTED_EDGE ( 'NONE', *, *, #13115, .F. ) ;
#13999 = CYLINDRICAL_SURFACE ( 'NONE', #27837, 2.000000000000012879 ) ;
#14000 = CARTESIAN_POINT ( 'NONE',  ( 6.000000000000052403, -1.607695154586662678, -169.6533121635129646 ) ) ;
#14001 = CARTESIAN_POINT ( 'NONE',  ( 105.9372167782374135, -0.7662911109076184779, 1.849990392679652151 ) ) ;
#14002 = ORIENTED_EDGE ( 'NONE', *, *, #20529, .F. ) ;
#14003 = CARTESIAN_POINT ( 'NONE',  ( 6.000000000000000888, -1.859271017917181981E-14, -141.0863248654051745 ) ) ;
#14004 = CARTESIAN_POINT ( 'NONE',  ( 151.4062500000000000, 6.000000000000005329, -2.485281374238555774 ) ) ;
#14005 = CARTESIAN_POINT ( 'NONE',  ( 4.763139720814407951, 2.750000000000002665, -117.2500000000000142 ) ) ;
#14006 = CARTESIAN_POINT ( 'NONE',  ( 20.68750000000004974, -1.097466725451439196, 2.649519052838419153 ) ) ;
#14007 = CARTESIAN_POINT ( 'NONE',  ( 3.608439182435180470, 6.249999999999982236, -129.5580127018922383 ) ) ;
#14008 = VERTEX_POINT ( 'NONE', #13358 ) ;
#14009 =( LENGTH_UNIT ( ) NAMED_UNIT ( * ) SI_UNIT ( .MILLI., .METRE. ) );
#14010 = CARTESIAN_POINT ( 'NONE',  ( -5.412658773652739619, 3.124999999999975131, -168.8169872981077901 ) ) ;
#14011 = CARTESIAN_POINT ( 'NONE',  ( 109.2499999999999147, 0.000000000000000000, 2.499999999999946709 ) ) ;
#14012 = ADVANCED_FACE ( 'NONE', ( #19933 ), #8560, .T. ) ;
#14013 = CARTESIAN_POINT ( 'NONE',  ( 10.56250000000007461, -1.999999999999971800, -0.8284271247462354770 ) ) ;
#14014 =( BOUNDED_CURVE ( )  B_SPLINE_CURVE ( 2, ( #12129, #5447, #7174, #24200, #709, #23768, #5300, #16588, #14567 ),
 .UNSPECIFIED., .F., .T. ) 
 B_SPLINE_CURVE_WITH_KNOTS ( ( 3, 2, 2, 2, 3 ),
 ( 0.3361111111111110827, 0.3370370370370370239, 0.3388888888888889062, 0.3407407407407407329, 0.3416666666666666741 ),
 .UNSPECIFIED. ) 
 CURVE ( )  GEOMETRIC_REPRESENTATION_ITEM ( )  RATIONAL_B_SPLINE_CURVE ( ( 0.9330127018922194093, 0.9330127018922174109, 1.000000000000000000, 0.8660254037844388186, 1.000000000000000000, 0.8660254037844388186, 1.000000000000000000, 0.9330127018922194093, 0.9330127018922194093 ) ) 
 REPRESENTATION_ITEM ( '' )  );
#14015 = CARTESIAN_POINT ( 'NONE',  ( 153.4761751345948255, 3.889087296526011706, 3.889087296526011706 ) ) ;
#14016 = CARTESIAN_POINT ( 'NONE',  ( -5.999999999999963585, -1.487416814333745711E-14, -134.9136751345948255 ) ) ;
#14017 = CARTESIAN_POINT ( 'NONE',  ( 157.7738248654052029, -3.889087296526011706, 3.889087296526011706 ) ) ;
#14018 = CARTESIAN_POINT ( 'NONE',  ( 109.1877832217621034, 0.7662911109079489913, -1.849990392679291551 ) ) ;
#14019 = MECHANICAL_DESIGN_GEOMETRIC_PRESENTATION_REPRESENTATION (  '', ( #8568 ), #16934 ) ;
#14020 = CARTESIAN_POINT ( 'NONE',  ( 5.412658773652712085, -3.125000000000086153, -177.9330127018922099 ) ) ;
#14021 = CYLINDRICAL_SURFACE ( 'NONE', #19986, 6.000000000000000888 ) ;
#14022 =( NAMED_UNIT ( * ) PLANE_ANGLE_UNIT ( ) SI_UNIT ( $, .RADIAN. ) );
#14023 = STYLED_ITEM ( 'NONE', ( #29339 ), #2852 ) ;
#14024 = DIRECTION ( 'NONE',  ( 0.000000000000000000, 0.000000000000000000, -1.000000000000000000 ) ) ;
#14025 = EDGE_CURVE ( 'NONE', #18896, #19610, #10562, .T. ) ;
#14026 = CARTESIAN_POINT ( 'NONE',  ( -4.763139720814407951, -2.750000000000016431, -122.5000000000000568 ) ) ;
#14027 =( BOUNDED_CURVE ( )  B_SPLINE_CURVE ( 2, ( #15449, #22489, #22329, #12992, #8814, #6030, #25218, #18199, #4186 ),
 .UNSPECIFIED., .F., .T. ) 
 B_SPLINE_CURVE_WITH_KNOTS ( ( 3, 2, 2, 2, 3 ),
 ( 0.9194444444444443976, 0.9203703703703703942, 0.9222222222222222765, 0.9240740740740740478, 0.9250000000000000444 ),
 .UNSPECIFIED. ) 
 CURVE ( )  GEOMETRIC_REPRESENTATION_ITEM ( )  RATIONAL_B_SPLINE_CURVE ( ( 0.9330127018922194093, 0.9330127018922154125, 1.000000000000000000, 0.8660254037844388186, 1.000000000000000000, 0.8660254037844388186, 1.000000000000000000, 0.9330127018922154125, 0.9330127018922194093 ) ) 
 REPRESENTATION_ITEM ( '' )  );
#14028 = EDGE_CURVE ( 'NONE', #28619, #16115, #10766, .T. ) ;
#14029 = CARTESIAN_POINT ( 'NONE',  ( 5.999999999999949374, 1.607695154586804565, -166.5193375672974128 ) ) ;
#14030 = CARTESIAN_POINT ( 'NONE',  ( 154.3050748654052597, 5.500000000000012434, 2.278174593052012309 ) ) ;
#14031 = ORIENTED_EDGE ( 'NONE', *, *, #14025, .F. ) ;
#14032 = CARTESIAN_POINT ( 'NONE',  ( 19.37500000000014211, 1.665334536937734811E-13, -2.649519052838333888 ) ) ;
#14033 = FACE_OUTER_BOUND ( 'NONE', #2758, .T. ) ;
#14034 = FACE_BOUND ( 'NONE', #15173, .T. ) ;
#14035 = ORIENTED_EDGE ( 'NONE', *, *, #8584, .T. ) ;
#14036 = CARTESIAN_POINT ( 'NONE',  ( 111.8122167782374419, 0.7662911109077987781, 1.849990392679772278 ) ) ;
#14037 = CARTESIAN_POINT ( 'NONE',  ( 0.000000000000000000, -5.999999999999991118, -115.0386751345948682 ) ) ;
#14038 = CIRCLE ( 'NONE', #19411, 0.5000000000000004441 ) ;
#14039 = CARTESIAN_POINT ( 'NONE',  ( 3.608439182435180470, -6.249999999999997335, -109.6919872981078186 ) ) ;
#14040 = FILL_AREA_STYLE_COLOUR ( '', #5740 ) ;
#14041 = CARTESIAN_POINT ( 'NONE',  ( 113.3988248654051745, -0.8284271247460852639, -1.999999999999791278 ) ) ;
#14042 = VERTEX_POINT ( 'NONE', #27278 ) ;
#14043 = ORIENTED_EDGE ( 'NONE', *, *, #11945, .T. ) ;
#14044 = CARTESIAN_POINT ( 'NONE',  ( 20.60117513459488237, -1.035533905932568999, 2.499999999999844569 ) ) ;
#14045 = CARTESIAN_POINT ( 'NONE',  ( 135.0937500000000284, 6.000000000000005329, 2.485281374238585972 ) ) ;
#14046 = CARTESIAN_POINT ( 'NONE',  ( -5.412658773652684552, -3.125000000000099920, -135.5669872981078470 ) ) ;
#14047 = CARTESIAN_POINT ( 'NONE',  ( 12.68750000000013500, -1.097466725451379244, 2.649519052838178457 ) ) ;
#14048 = FILL_AREA_STYLE_COLOUR ( '', #19666 ) ;
#14049 = EDGE_CURVE ( 'NONE', #20809, #30356, #11767, .T. ) ;
#14050 = CARTESIAN_POINT ( 'NONE',  ( 19.12500000000014211, 1.414213562373256572, 1.414213562373034527 ) ) ;
#14051 = DIRECTION ( 'NONE',  ( 0.000000000000000000, 0.000000000000000000, -1.000000000000000000 ) ) ;
#14052 = CARTESIAN_POINT ( 'NONE',  ( -6.000000000000000888, 1.067854986875958443E-15, 7.560779664488942560E-35 ) ) ;
#14053 = CYLINDRICAL_SURFACE ( 'NONE', #25495, 6.000000000000000888 ) ;
#14054 = CARTESIAN_POINT ( 'NONE',  ( 146.6101497308104058, 3.535533905932725318, 3.535533905932725318 ) ) ;
#14055 = CARTESIAN_POINT ( 'NONE',  ( 112.1636751345948113, 1.414213562373034527, -1.414213562373145550 ) ) ;
#14056 = CARTESIAN_POINT ( 'NONE',  ( 12.72617513459496408, -2.499999999999964473, 1.035533905932749299 ) ) ;
#14057 = DIRECTION ( 'NONE',  ( -7.147005652999508048E-36, 5.642372883946980038E-36, 1.000000000000000000 ) ) ;
#14058 = AXIS2_PLACEMENT_3D ( 'NONE', #8965, #27366, #27215 ) ;
#14059 = CARTESIAN_POINT ( 'NONE',  ( 24.80639502529410834, -0.7518803807380188831, -2.066273979619694501 ) ) ;
#14060 = FACE_OUTER_BOUND ( 'NONE', #28515, .T. ) ;
#14061 = CARTESIAN_POINT ( 'NONE',  ( 108.3124999999997442, -1.035533905932629173, 2.500000000000205169 ) ) ;
#14062 = LINE ( 'NONE', #11445, #6414 ) ;
#14063 = EDGE_CURVE ( 'NONE', #2929, #269, #13742, .T. ) ;
#14064 = CARTESIAN_POINT ( 'NONE',  ( 15.77382486540523310, 2.500000000000084821, 1.035533905932689347 ) ) ;
#14065 = CARTESIAN_POINT ( 'NONE',  ( 5.412658773652739619, 3.124999999999988898, -143.1830127018922667 ) ) ;
#14066 = CARTESIAN_POINT ( 'NONE',  ( -5.999999999999957367, 1.607695154586737507, -148.4806624327026157 ) ) ;
#14067 =( BOUNDED_CURVE ( )  B_SPLINE_CURVE ( 2, ( #17145, #26469, #1566 ),
 .UNSPECIFIED., .F., .F. ) 
 B_SPLINE_CURVE_WITH_KNOTS ( ( 3, 3 ),
 ( 0.8875000000000003997, 0.8903868608885109337 ),
 .UNSPECIFIED. ) 
 CURVE ( )  GEOMETRIC_REPRESENTATION_ITEM ( )  RATIONAL_B_SPLINE_CURVE ( ( 0.9999999999999945599, 0.9648401279346661141, 0.9621607869126811430 ) ) 
 REPRESENTATION_ITEM ( '' )  );
#14068 = DIRECTION ( 'NONE',  ( -5.551115123125774074E-17, -1.000000000000000000, -6.394689268473234689E-36 ) ) ;
#14069 = ORIENTED_EDGE ( 'NONE', *, *, #14398, .F. ) ;
#14070 = CARTESIAN_POINT ( 'NONE',  ( -3.175426480542816066, -5.500000000000057732, -57.87500000000004974 ) ) ;
#14071 = CYLINDRICAL_SURFACE ( 'NONE', #25194, 6.000000000000000888 ) ;
#14072 = CARTESIAN_POINT ( 'NONE',  ( 5.196152422706629359, -2.999999999999988898, -178.7113248654052029 ) ) ;
#14073 = ORIENTED_EDGE ( 'NONE', *, *, #9650, .F. ) ;
#14074 = CARTESIAN_POINT ( 'NONE',  ( 107.0624999999998010, 2.500000000000114575, 1.035533905932989551 ) ) ;
#14075 = CARTESIAN_POINT ( 'NONE',  ( 142.3125000000000284, 4.242640687119298093, -4.242640687119298093 ) ) ;
#14076 = CARTESIAN_POINT ( 'NONE',  ( 11.50000000000006573, -1.999999999999835243, 0.000000000000000000 ) ) ;
#14077 = CARTESIAN_POINT ( 'NONE',  ( -3.608439182435052128, -6.250000000000110134, -102.4419872981078328 ) ) ;
#14078 = CARTESIAN_POINT ( 'NONE',  ( -40.00000000000000000, -20.00000000000021316, 4.000000000000003553 ) ) ;
#14079 = CARTESIAN_POINT ( 'NONE',  ( 135.4687500000000853, -2.485281374238585972, 6.000000000000005329 ) ) ;
#14080 = CARTESIAN_POINT ( 'NONE',  ( -5.999999999999963585, -1.487416814333745711E-14, -172.4136751345948255 ) ) ;
#14081 = VECTOR ( 'NONE', #439, 1000.000000000000000 ) ;
#14082 = CARTESIAN_POINT ( 'NONE',  ( -4.763139720814407951, 2.749999999999946709, -134.7500000000000284 ) ) ;
#14083 = ORIENTED_EDGE ( 'NONE', *, *, #25628, .T. ) ;
#14084 = ORIENTED_EDGE ( 'NONE', *, *, #21167, .F. ) ;
#14085 = SURFACE_SIDE_STYLE ('',( #23858 ) ) ;
#14086 = CARTESIAN_POINT ( 'NONE',  ( 4.763139720814407951, 2.750000000000002665, -61.75000000000002842 ) ) ;
#14087 = EDGE_CURVE ( 'NONE', #20687, #2600, #14871, .T. ) ;
#14088 = CARTESIAN_POINT ( 'NONE',  ( 0.000000000000000000, 5.999999999999977796, -66.28867513459479710 ) ) ;
#14089 = EDGE_CURVE ( 'NONE', #25684, #29332, #8321, .T. ) ;
#14090 = CARTESIAN_POINT ( 'NONE',  ( 5.412658773652739619, 3.124999999999988898, -90.68301270189226670 ) ) ;
#14091 = CARTESIAN_POINT ( 'NONE',  ( -0.5000000000000004441, -10.00000000000000888, -5.000000000000004441 ) ) ;
#14092 = VECTOR ( 'NONE', #22233, 1000.000000000000000 ) ;
#14093 = CARTESIAN_POINT ( 'NONE',  ( 161.0000000000000284, 0.000000000000000000, 0.000000000000000000 ) ) ;
#14094 = CYLINDRICAL_SURFACE ( 'NONE', #24071, 2.499999999999999112 ) ;
#14095 = CARTESIAN_POINT ( 'NONE',  ( 118.5627832217621034, 0.7662911109077087390, 1.849990392679772278 ) ) ;
#14096 = AXIS2_PLACEMENT_3D ( 'NONE', #16549, #4820, #212 ) ;
#14097 = CARTESIAN_POINT ( 'NONE',  ( -2.775557561562891351E-14, -5.500000000000115463, -149.2500000000000000 ) ) ;
#14098 = CARTESIAN_POINT ( 'NONE',  ( 140.0000000000000284, -9.600000000000010303, -7.200000000000006395 ) ) ;
#14099 = CARTESIAN_POINT ( 'NONE',  ( 3.175426480543072749, 5.499999999999865885, -138.1250000000000284 ) ) ;
#14100 = CARTESIAN_POINT ( 'NONE',  ( 3.608439182435180470, 6.249999999999982236, -162.5580127018921814 ) ) ;
#14101 = CARTESIAN_POINT ( 'NONE',  ( -5.196152422706601826, 2.999999999999975131, -89.46132486540525974 ) ) ;
#14102 = CARTESIAN_POINT ( 'NONE',  ( 6.350852961086080661, -9.614813431917819062E-14, -75.37500000000002842 ) ) ;
#14103 = SURFACE_STYLE_FILL_AREA ( #66 ) ;
#14104 = CARTESIAN_POINT ( 'NONE',  ( -3.175426480542816510, 5.499999999999865885, -62.87500000000001421 ) ) ;
#14105 = SURFACE_SIDE_STYLE ('',( #25724 ) ) ;
#14106 = CARTESIAN_POINT ( 'NONE',  ( 6.000000000000000888, -1.607695154586752384, -114.1533121635129930 ) ) ;
#14107 = CARTESIAN_POINT ( 'NONE',  ( -5.196152422706573404, -3.000000000000002665, -175.2886751345948539 ) ) ;
#14108 =( GEOMETRIC_REPRESENTATION_CONTEXT ( 3 ) GLOBAL_UNCERTAINTY_ASSIGNED_CONTEXT ( ( #25912 ) ) GLOBAL_UNIT_ASSIGNED_CONTEXT ( ( #22010, #29359, #24298 ) ) REPRESENTATION_CONTEXT ( 'NONE', 'WORKASPACE' ) );
#14109 = CARTESIAN_POINT ( 'NONE',  ( 155.4375000000000284, -4.242640687119298093, -4.242640687119298093 ) ) ;
#14110 = CYLINDRICAL_SURFACE ( 'NONE', #1318, 6.000000000000000888 ) ;
#14111 = CARTESIAN_POINT ( 'NONE',  ( 119.4997167782375982, 1.308140751793723799, -1.308140751793640533 ) ) ;
#14112 = CYLINDRICAL_SURFACE ( 'NONE', #24290, 6.000000000000000888 ) ;
#14113 =( BOUNDED_CURVE ( )  B_SPLINE_CURVE ( 2, ( #13915, #28426, #9567, #14213, #5230, #16952, #7255, #12503, #2635 ),
 .UNSPECIFIED., .F., .T. ) 
 B_SPLINE_CURVE_WITH_KNOTS ( ( 3, 2, 2, 2, 3 ),
 ( 0.3583333333333333370, 0.3592592592592592782, 0.3611111111111111049, 0.3629629629629629872, 0.3638888888888889284 ),
 .UNSPECIFIED. ) 
 CURVE ( )  GEOMETRIC_REPRESENTATION_ITEM ( )  RATIONAL_B_SPLINE_CURVE ( ( 0.9330127018922194093, 0.9330127018922194093, 1.000000000000000000, 0.8660254037844388186, 1.000000000000000000, 0.8660254037844388186, 1.000000000000000000, 0.9330127018922174109, 0.9330127018922194093 ) ) 
 REPRESENTATION_ITEM ( '' )  );
#14114 = ORIENTED_EDGE ( 'NONE', *, *, #17517, .F. ) ;
#14115 = CARTESIAN_POINT ( 'NONE',  ( 148.5937500000000284, 6.000000000000005329, 2.485281374238585972 ) ) ;
#14116 = PRESENTATION_LAYER_ASSIGNMENT (  '', '', ( #27787 ) ) ;
#14117 = CARTESIAN_POINT ( 'NONE',  ( 115.5627832217620892, 0.7662911109077987781, 1.849990392679772278 ) ) ;
#14118 = CARTESIAN_POINT ( 'NONE',  ( -3.175426480542816510, -5.500000000000057732, -153.8750000000000000 ) ) ;
#14119 = CARTESIAN_POINT ( 'NONE',  ( -6.000000000000007105, -1.607695154586655129, -85.34668783648703538 ) ) ;
#14120 = ORIENTED_EDGE ( 'NONE', *, *, #23526, .T. ) ;
#14121 = ORIENTED_EDGE ( 'NONE', *, *, #10064, .F. ) ;
#14122 = VERTEX_POINT ( 'NONE', #10088 ) ;
#14123 = CARTESIAN_POINT ( 'NONE',  ( 4.763139720814407951, 2.750000000000002665, -93.25000000000000000 ) ) ;
#14124 = EDGE_CURVE ( 'NONE', #12257, #20028, #27509, .T. ) ;
#14125 = CARTESIAN_POINT ( 'NONE',  ( 3.608439182435180470, -6.249999999999997335, -107.5580127018922667 ) ) ;
#14126 = DIRECTION ( 'NONE',  ( 1.000000000000000000, 0.000000000000000000, -0.000000000000000000 ) ) ;
#14127 = CARTESIAN_POINT ( 'NONE',  ( 158.6101497308104058, 3.535533905932725318, 3.535533905932725318 ) ) ;
#14128 = AXIS2_PLACEMENT_3D ( 'NONE', #23716, #23569, #28738 ) ;
#14129 = CARTESIAN_POINT ( 'NONE',  ( 0.000000000000000000, 5.499999999999991118, -163.5000000000000284 ) ) ;
#14130 = CARTESIAN_POINT ( 'NONE',  ( 6.000000000000000888, -1.607695154586752384, -63.15331216351300014 ) ) ;
#14131 =( GEOMETRIC_REPRESENTATION_CONTEXT ( 3 ) GLOBAL_UNCERTAINTY_ASSIGNED_CONTEXT ( ( #9765 ) ) GLOBAL_UNIT_ASSIGNED_CONTEXT ( ( #8652, #25531, #16366 ) ) REPRESENTATION_CONTEXT ( 'NONE', 'WORKASPACE' ) );
#14132 = AXIS2_PLACEMENT_3D ( 'NONE', #8926, #16478, #11718 ) ;
#14133 = SURFACE_STYLE_USAGE ( .BOTH. , #16576 ) ;
#14134 = CARTESIAN_POINT ( 'NONE',  ( 4.763139720814407951, 2.750000000000002665, -174.2500000000000284 ) ) ;
#14135 = DIRECTION ( 'NONE',  ( 1.000000000000000000, -5.551115123125773458E-17, -1.260129944081490338E-35 ) ) ;
#14136 = CARTESIAN_POINT ( 'NONE',  ( -3.175426480542816510, -5.500000000000057732, -153.8750000000000000 ) ) ;
#14137 = CARTESIAN_POINT ( 'NONE',  ( 114.0624999999997300, 2.500000000000114575, 1.035533905932989551 ) ) ;
#14138 = CARTESIAN_POINT ( 'NONE',  ( -3.175426480542816066, 5.499999999999865885, -98.87499999999998579 ) ) ;
#14139 = CARTESIAN_POINT ( 'NONE',  ( -5.999999999999956479, -1.607695154586745057, -159.7693375672974412 ) ) ;
#14140 = DIRECTION ( 'NONE',  ( 0.000000000000000000, 1.000000000000000000, 0.000000000000000000 ) ) ;
#14141 = CARTESIAN_POINT ( 'NONE',  ( -3.175426480542816510, -5.500000000000057732, -87.87500000000000000 ) ) ;
#14142 = CARTESIAN_POINT ( 'NONE',  ( 159.7648502691896510, 3.535533905932725318, 3.535533905932752852 ) ) ;
#14143 = CARTESIAN_POINT ( 'NONE',  ( 0.8056953124617616258, -15.44741955337846306, 8.223657085175583248 ) ) ;
#14144 = VERTEX_POINT ( 'NONE', #2041 ) ;
#14145 = CARTESIAN_POINT ( 'NONE',  ( 10.12500000000007816, -2.649519052838111843, 1.110223024625156540E-13 ) ) ;
#14146 = CARTESIAN_POINT ( 'NONE',  ( 113.4374999999998863, -2.499999999999994671, 1.035533905932869425 ) ) ;
#14147 = CARTESIAN_POINT ( 'NONE',  ( -6.000000000000000888, 1.067854986875958443E-15, 7.560779664488942560E-35 ) ) ;
#14148 = CARTESIAN_POINT ( 'NONE',  ( 108.1252832217622455, 0.000000000000000000, -1.849990392679301543 ) ) ;
#14149 = CARTESIAN_POINT ( 'NONE',  ( 23.78867513459503868, -2.499999999999891198, -2.220446049250313081E-13 ) ) ;
#14150 = ORIENTED_EDGE ( 'NONE', *, *, #14400, .F. ) ;
#14151 = FACE_OUTER_BOUND ( 'NONE', #20241, .T. ) ;
#14152 =( GEOMETRIC_REPRESENTATION_CONTEXT ( 3 ) GLOBAL_UNCERTAINTY_ASSIGNED_CONTEXT ( ( #23887 ) ) GLOBAL_UNIT_ASSIGNED_CONTEXT ( ( #3816, #23042, #11229 ) ) REPRESENTATION_CONTEXT ( 'NONE', 'WORKASPACE' ) );
#14153 = ADVANCED_FACE ( 'NONE', ( #6643 ), #22938, .T. ) ;
#14154 = ORIENTED_EDGE ( 'NONE', *, *, #5857, .T. ) ;
#14155 = CARTESIAN_POINT ( 'NONE',  ( -5.196152422706573404, -3.000000000000002665, -141.7113248654052313 ) ) ;
#14156 = CARTESIAN_POINT ( 'NONE',  ( 148.3125000000000284, 4.242640687119298093, -4.242640687119298093 ) ) ;
#14157 = ORIENTED_EDGE ( 'NONE', *, *, #9261, .T. ) ;
#14158 = CARTESIAN_POINT ( 'NONE',  ( -6.350852961085760029, -1.281975124255709124E-13, -110.6249999999999858 ) ) ;
#14159 = CARTESIAN_POINT ( 'NONE',  ( 23.37500000000003553, 2.649519052838444910, 0.000000000000000000 ) ) ;
#14160 = EDGE_CURVE ( 'NONE', #15916, #13609, #4333, .T. ) ;
#14161 = CARTESIAN_POINT ( 'NONE',  ( 7.216878364870455975, -6.409875621278545621E-14, -132.8080127018922667 ) ) ;
#14162 = ORIENTED_EDGE ( 'NONE', *, *, #20383, .F. ) ;
#14163 =( NAMED_UNIT ( * ) PLANE_ANGLE_UNIT ( ) SI_UNIT ( $, .RADIAN. ) );
#14164 = CARTESIAN_POINT ( 'NONE',  ( 2.775557561562891351E-14, -6.250000000000061284, -165.3169872981078470 ) ) ;
#14165 = CARTESIAN_POINT ( 'NONE',  ( 106.7499999999999147, -8.326672684688674053E-14, -2.499999999999946709 ) ) ;
#14166 = SURFACE_STYLE_USAGE ( .BOTH. , #4737 ) ;
#14167 = CARTESIAN_POINT ( 'NONE',  ( 0.1950468348593054624, -15.42105542096816073, -8.274702966242770685 ) ) ;
#14168 = CARTESIAN_POINT ( 'NONE',  ( -5.999999999999919176, 1.607695154586804565, -95.40331216351297883 ) ) ;
#14169 = CARTESIAN_POINT ( 'NONE',  ( 119.2113248654050466, -1.999999999999946265, 2.220446049250313081E-13 ) ) ;
#14170 = DIRECTION ( 'NONE',  ( 1.000000000000000000, -5.551115123125773458E-17, -1.260129944081490338E-35 ) ) ;
#14171 = CARTESIAN_POINT ( 'NONE',  ( 108.1252832217622455, 0.000000000000000000, -1.849990392679301543 ) ) ;
#14172 = CARTESIAN_POINT ( 'NONE',  ( -3.608439182435052128, -6.250000000000110134, -178.3080127018922383 ) ) ;
#14173 = CARTESIAN_POINT ( 'NONE',  ( -0.5043617743979594836, -9.495638225602176519, -4.110987936241992102 ) ) ;
#14174 = CARTESIAN_POINT ( 'NONE',  ( 0.000000000000000000, 0.000000000000000000, 0.000000000000000000 ) ) ;
#14175 = AXIS2_PLACEMENT_3D ( 'NONE', #28451, #7424, #16832 ) ;
#14176 = CARTESIAN_POINT ( 'NONE',  ( 5.999999999999974243, 1.607695154586759934, -123.5966878364870212 ) ) ;
#14177 = CARTESIAN_POINT ( 'NONE',  ( 0.000000000000000000, 5.499999999999991118, -124.5000000000000568 ) ) ;
#14178 = CARTESIAN_POINT ( 'NONE',  ( 135.0976013656030261, -7.965572835763115478, -8.241760388316306418 ) ) ;
#14179 = CARTESIAN_POINT ( 'NONE',  ( 114.7886751345947403, -1.999999999999946265, 0.000000000000000000 ) ) ;
#14180 = VERTEX_POINT ( 'NONE', #9101 ) ;
#14181 = CARTESIAN_POINT ( 'NONE',  ( 23.12500000000011724, -2.649519052838167354, -1.665334536937734811E-13 ) ) ;
#14182 = CARTESIAN_POINT ( 'NONE',  ( -0.04479393756897805806, -15.28421419621745692, -7.194883460697197641 ) ) ;
#14183 = LINE ( 'NONE', #6761, #13159 ) ;
#14184 = CARTESIAN_POINT ( 'NONE',  ( 5.999999999999949374, 1.607695154586804565, -156.0193375672974412 ) ) ;
#14185 = ORIENTED_EDGE ( 'NONE', *, *, #22847, .T. ) ;
#14186 = CARTESIAN_POINT ( 'NONE',  ( 118.6488248654050324, 2.000000000000122125, -0.8284271247459952248 ) ) ;
#14187 = ADVANCED_FACE ( 'NONE', ( #5744 ), #4175, .T. ) ;
#14188 = CARTESIAN_POINT ( 'NONE',  ( -3.464101615137757051, -5.999999999999979572, -176.6636751345947687 ) ) ;
#14189 = CARTESIAN_POINT ( 'NONE',  ( 6.000000000000000888, -1.607695154586752384, -125.2306624327026157 ) ) ;
#14190 = CARTESIAN_POINT ( 'NONE',  ( 113.3363248654051176, -1.414213562373201061, -1.414213562373034527 ) ) ;
#14191 = VERTEX_POINT ( 'NONE', #18498 ) ;
#14192 = ORIENTED_EDGE ( 'NONE', *, *, #11786, .F. ) ;
#14193 = CARTESIAN_POINT ( 'NONE',  ( -3.464101615137725076, 5.999999999999979572, -141.1636751345948255 ) ) ;
#14194 = CARTESIAN_POINT ( 'NONE',  ( 135.0000000000000284, 6.000000000000005329, 0.000000000000000000 ) ) ;
#14195 = EDGE_CURVE ( 'NONE', #15497, #18067, #23137, .T. ) ;
#14196 =( BOUNDED_CURVE ( )  B_SPLINE_CURVE ( 2, ( #14397, #9290, #24269, #18990, #3217, #3369, #19685, #9600, #19128 ),
 .UNSPECIFIED., .F., .T. ) 
 B_SPLINE_CURVE_WITH_KNOTS ( ( 3, 2, 2, 2, 3 ),
 ( 0.9416666666666666519, 0.9425925925925926485, 0.9444444444444444198, 0.9462962962962963021, 0.9472222222222221877 ),
 .UNSPECIFIED. ) 
 CURVE ( )  GEOMETRIC_REPRESENTATION_ITEM ( )  RATIONAL_B_SPLINE_CURVE ( ( 0.9330127018922194093, 0.9330127018922154125, 1.000000000000000000, 0.8660254037844388186, 1.000000000000000000, 0.8660254037844388186, 1.000000000000000000, 0.9330127018922234061, 0.9330127018922194093 ) ) 
 REPRESENTATION_ITEM ( '' )  );
#14197 = ORIENTED_EDGE ( 'NONE', *, *, #10950, .F. ) ;
#14198 = CARTESIAN_POINT ( 'NONE',  ( -3.608439182435052128, -6.250000000000110134, -139.9419872981078470 ) ) ;
#14199 = FILL_AREA_STYLE ('',( #7081 ) ) ;
#14200 = CARTESIAN_POINT ( 'NONE',  ( 12.75000000000017764, -1.873492889144845464, 1.873492889144845464 ) ) ;
#14201 = CARTESIAN_POINT ( 'NONE',  ( 5.999999999999949374, -1.607695154586841868, -171.1533121635130215 ) ) ;
#14202 = CARTESIAN_POINT ( 'NONE',  ( 144.2663997308104058, -4.999999999999989342, -2.071067811865468400 ) ) ;
#14203 = CARTESIAN_POINT ( 'NONE',  ( 135.0000000000000284, 0.000000000000000000, 0.000000000000000000 ) ) ;
#14204 = CARTESIAN_POINT ( 'NONE',  ( 0.000000000000000000, -9.500000000000008882, 8.000000000000007105 ) ) ;
#14205 = CARTESIAN_POINT ( 'NONE',  ( 5.000000000000087930, 5.551115123125782702E-14, -5.551115123125782702E-14 ) ) ;
#14206 = CARTESIAN_POINT ( 'NONE',  ( -5.999999999999963585, -1.487416814333745711E-14, -97.41367513459481131 ) ) ;
#14207 = CYLINDRICAL_SURFACE ( 'NONE', #26854, 2.499999999999999112 ) ;
#14208 = CARTESIAN_POINT ( 'NONE',  ( 111.7499999999998010, 0.000000000000000000, -2.499999999999946709 ) ) ;
#14209 = DIRECTION ( 'NONE',  ( -0.000000000000000000, -0.000000000000000000, -1.000000000000000000 ) ) ;
#14210 = CARTESIAN_POINT ( 'NONE',  ( 5.999999999999999112, 2.951592740943527306E-14, -149.1636751345948824 ) ) ;
#14211 = ORIENTED_EDGE ( 'NONE', *, *, #7561, .F. ) ;
#14212 = CARTESIAN_POINT ( 'NONE',  ( -3.175426480542816066, 5.499999999999865885, -53.87500000000003553 ) ) ;
#14213 = CARTESIAN_POINT ( 'NONE',  ( -3.464101615137757051, -5.999999999999979572, -133.1636751345948539 ) ) ;
#14214 = CARTESIAN_POINT ( 'NONE',  ( 3.464101615137852974, 5.999999999999884537, -79.33632486540523132 ) ) ;
#14215 = LINE ( 'NONE', #6948, #17035 ) ;
#14216 = EDGE_LOOP ( 'NONE', ( #2258, #2713, #9502, #6744 ) ) ;
#14217 = CARTESIAN_POINT ( 'NONE',  ( 106.1874999999999289, 1.035533905932839449, 2.500000000000265121 ) ) ;
#14218 = CARTESIAN_POINT ( 'NONE',  ( 140.3437500000000284, -6.000000000000005329, -2.485281374238556218 ) ) ;
#14219 = MANIFOLD_SOLID_BREP ( 'Cut-Sweep1', #3118 ) ;
#14220 = EDGE_CURVE ( 'NONE', #3951, #3318, #18039, .T. ) ;
#14221 = CARTESIAN_POINT ( 'NONE',  ( 7.216878364870455975, -6.409875621278545621E-14, -100.4419872981078328 ) ) ;
#14222 = CARTESIAN_POINT ( 'NONE',  ( 142.6011751345948539, 3.889087296526011706, -3.889087296526011706 ) ) ;
#14223 = CARTESIAN_POINT ( 'NONE',  ( 161.2351497308104058, 3.535533905932725318, -3.535533905932725318 ) ) ;
#14224 = CARTESIAN_POINT ( 'NONE',  ( 118.9999999999998437, 2.500000000000057732, 2.220446049250313081E-13 ) ) ;
#14225 = ORIENTED_EDGE ( 'NONE', *, *, #24418, .T. ) ;
#14226 = ADVANCED_FACE ( 'NONE', ( #23255 ), #14502, .F. ) ;
#14227 = CARTESIAN_POINT ( 'NONE',  ( 4.763139720814407951, 2.750000000000002665, -133.7500000000000284 ) ) ;
#14228 = EDGE_CURVE ( 'NONE', #23810, #10268, #23549, .T. ) ;
#14229 = ORIENTED_EDGE ( 'NONE', *, *, #29117, .F. ) ;
#14230 = ORIENTED_EDGE ( 'NONE', *, *, #3096, .T. ) ;
#14231 = CARTESIAN_POINT ( 'NONE',  ( -5.196152422706601826, 2.999999999999975131, -162.9613248654052029 ) ) ;
#14232 = CARTESIAN_POINT ( 'NONE',  ( 3.175426480543072749, -5.500000000000105693, -68.12500000000002842 ) ) ;
#14233 = AXIS2_PLACEMENT_3D ( 'NONE', #9517, #12004, #9051 ) ;
#14234 = CARTESIAN_POINT ( 'NONE',  ( 140.0000000000000284, -8.500000000000007105, 8.000000000000007105 ) ) ;
#14235 = CARTESIAN_POINT ( 'NONE',  ( 5.196152422706629359, 3.000000000000002665, -66.53867513459482552 ) ) ;
#14236 = CARTESIAN_POINT ( 'NONE',  ( -3.608439182435115633, 6.249999999999965361, -79.80801270189226670 ) ) ;
#14237 = DIRECTION ( 'NONE',  ( -7.147005652999508048E-36, 5.642372883946980038E-36, 1.000000000000000000 ) ) ;
#14238 = CARTESIAN_POINT ( 'NONE',  ( 5.196152422706629359, -2.999999999999988898, -113.2886751345948397 ) ) ;
#14239 =( BOUNDED_CURVE ( )  B_SPLINE_CURVE ( 2, ( #10345, #2953, #19706, #28744, #1102, #7863, #17275, #5704, #28592 ),
 .UNSPECIFIED., .F., .F. ) 
 B_SPLINE_CURVE_WITH_KNOTS ( ( 3, 2, 2, 2, 3 ),
 ( 0.9083333333333333259, 0.9092592592592592116, 0.9111111111111110938, 0.9129629629629629761, 0.9138888888888888618 ),
 .UNSPECIFIED. ) 
 CURVE ( )  GEOMETRIC_REPRESENTATION_ITEM ( )  RATIONAL_B_SPLINE_CURVE ( ( 0.9330127018922194093, 0.9330127018922194093, 1.000000000000000000, 0.8660254037844388186, 1.000000000000000000, 0.8660254037844388186, 1.000000000000000000, 0.9330127018922234061, 0.9330127018922194093 ) ) 
 REPRESENTATION_ITEM ( '' )  );
#14240 = CARTESIAN_POINT ( 'NONE',  ( 105.6247167782375271, 1.849990392679495832, 0.000000000000000000 ) ) ;
#14241 = CARTESIAN_POINT ( 'NONE',  ( 120.0627832217621602, -0.7662911109077388261, -1.849990392679291551 ) ) ;
#14242 = CARTESIAN_POINT ( 'NONE',  ( 4.763139720814407951, -2.749999999999988454, -147.5000000000000284 ) ) ;
#14243 = DIRECTION ( 'NONE',  ( -7.147005652999508048E-36, 5.642372883946980038E-36, 1.000000000000000000 ) ) ;
#14244 = CARTESIAN_POINT ( 'NONE',  ( 3.608439182435180470, -6.249999999999997335, -160.0580127018921814 ) ) ;
#14245 = CARTESIAN_POINT ( 'NONE',  ( -1.285375204280330350E-15, -10.49588505988223375, 1.184433945098074864E-34 ) ) ;
#14246 = CARTESIAN_POINT ( 'NONE',  ( 0.000000000000000000, 5.499999999999991118, -79.50000000000001421 ) ) ;
#14247 = CARTESIAN_POINT ( 'NONE',  ( 6.350852961086080661, -9.614813431917819062E-14, -61.87500000000000711 ) ) ;
#14248 = CARTESIAN_POINT ( 'NONE',  ( -5.999999999999962697, 3.323446944526963260E-14, -156.8363248654052313 ) ) ;
#14249 = CARTESIAN_POINT ( 'NONE',  ( 143.4523502691896510, 0.000000000000000000, 5.000000000000004441 ) ) ;
#14250 = DIRECTION ( 'NONE',  ( 0.000000000000000000, 1.000000000000000000, -0.000000000000000000 ) ) ;
#14251 = CARTESIAN_POINT ( 'NONE',  ( 159.8437500000000284, -6.000000000000005329, -2.485281374238556218 ) ) ;
#14252 = FACE_OUTER_BOUND ( 'NONE', #14543, .T. ) ;
#14253 = DIRECTION ( 'NONE',  ( 1.000000000000000000, -0.000000000000000000, -0.000000000000000000 ) ) ;
#14254 = EDGE_CURVE ( 'NONE', #22647, #26264, #2132, .T. ) ;
#14255 = AXIS2_PLACEMENT_3D ( 'NONE', #15025, #420, #19339 ) ;
#14256 = DIRECTION ( 'NONE',  ( -7.147005652999508048E-36, 5.642372883946980038E-36, 1.000000000000000000 ) ) ;
#14257 = CARTESIAN_POINT ( 'NONE',  ( 117.1247167782376408, -1.849990392679579099, 1.110223024625156540E-13 ) ) ;
#14258 = CARTESIAN_POINT ( 'NONE',  ( 3.464101615137852974, 5.999999999999884537, -82.33632486540524553 ) ) ;
#14259 = ORIENTED_EDGE ( 'NONE', *, *, #3779, .T. ) ;
#14260 = AXIS2_PLACEMENT_3D ( 'NONE', #19966, #15864, #10613 ) ;
#14261 = CARTESIAN_POINT ( 'NONE',  ( 152.1562500000000284, -6.000000000000005329, 2.485281374238555774 ) ) ;
#14262 = COLOUR_RGB ( '', 0.72549020, 0.75294118, 0.79215686) ;
#14263 = ORIENTED_EDGE ( 'NONE', *, *, #22715, .T. ) ;
#14264 = ADVANCED_FACE ( 'NONE', ( #21546 ), #2631, .T. ) ;
#14265 = CARTESIAN_POINT ( 'NONE',  ( 22.93749999999996447, 1.999999999999971800, -0.8284271247462354770 ) ) ;
#14266 = CARTESIAN_POINT ( 'NONE',  ( -3.608439182435115633, 6.249999999999965361, -155.4419872981078186 ) ) ;
#14267 = ORIENTED_EDGE ( 'NONE', *, *, #20001, .T. ) ;
#14268 = CARTESIAN_POINT ( 'NONE',  ( 4.763139720814407951, 2.750000000000002665, -85.75000000000000000 ) ) ;
#14269 = CARTESIAN_POINT ( 'NONE',  ( -7.216878364870328078, 0.000000000000000000, -102.0580127018922383 ) ) ;
#14270 = ORIENTED_EDGE ( 'NONE', *, *, #2285, .T. ) ;
#14271 = CARTESIAN_POINT ( 'NONE',  ( 157.8601497308104058, -3.535533905932725318, -3.535533905932725318 ) ) ;
#14272 = CARTESIAN_POINT ( 'NONE',  ( 159.2738248654052029, -3.889087296526011706, 3.889087296526011706 ) ) ;
#14273 = AXIS2_PLACEMENT_3D ( 'NONE', #838, #4205, #20210 ) ;
#14274 = CARTESIAN_POINT ( 'NONE',  ( 135.8007686613932208, -8.946933464891957399, 7.999999999999145572 ) ) ;
#14275 = CARTESIAN_POINT ( 'NONE',  ( 4.763139720814407951, 2.750000000000002665, -175.7500000000000284 ) ) ;
#14276 = CARTESIAN_POINT ( 'NONE',  ( -5.196152422706601826, 2.999999999999975131, -161.4613248654052029 ) ) ;
#14277 = CARTESIAN_POINT ( 'NONE',  ( 4.763139720814407951, 2.750000000000002665, -156.2500000000000000 ) ) ;
#14278 = CARTESIAN_POINT ( 'NONE',  ( 110.4374999999997442, -2.500000000000024425, 1.035533905932809473 ) ) ;
#14279 = CARTESIAN_POINT ( 'NONE',  ( -3.175426480542816066, -5.500000000000057732, -99.87500000000000000 ) ) ;
#14280 = FILL_AREA_STYLE_COLOUR ( '', #13455 ) ;
#14281 = CARTESIAN_POINT ( 'NONE',  ( 115.2886751345946550, 2.000000000000112799, 3.330669073875469621E-13 ) ) ;
#14283 = CARTESIAN_POINT ( 'NONE',  ( 6.350852961086080661, -9.614813431917819062E-14, -90.37500000000000000 ) ) ;
#14282 = CARTESIAN_POINT ( 'NONE',  ( 3.175426480543072749, -5.500000000000105693, -155.1250000000000000 ) ) ;
#14284 =( BOUNDED_SURFACE ( )  B_SPLINE_SURFACE ( 3, 2, ( 
 ( #30016, #14098, #4519 ),
 ( #20821, #23287, #13784 ),
 ( #28002, #4665, #16244 ),
 ( #13625, #13473, #20505 ),
 ( #13941, #16092, #30169 ),
 ( #9133, #2228, #2377 ),
 ( #6819, #21122, #60 ),
 ( #6356, #15790, #1757 ) ),
 .UNSPECIFIED., .F., .F., .F. ) 
 B_SPLINE_SURFACE_WITH_KNOTS ( ( 4, 2, 2, 4 ),
 ( 3, 3 ),
 ( 0.0005074624230801699385, 0.001406250641872334528, 0.001855644751268416878, 0.002305038860664499010 ),
 ( 0.000000000000000000, 1.000000000000000000 ),
 .UNSPECIFIED. ) 
 GEOMETRIC_REPRESENTATION_ITEM ( )  RATIONAL_B_SPLINE_SURFACE ( (
 ( 1.000000000000000000, 0.7071067811865475727, 1.000000000000000000),
 ( 1.000000000000000000, 0.7582538634876517802, 1.000000000000000000),
 ( 1.000000000000000000, 0.8074746405292959617, 1.000000000000000000),
 ( 1.000000000000000000, 0.8664425519722945834, 1.000000000000000000),
 ( 1.000000000000000000, 0.8838341264643537754, 1.000000000000000000),
 ( 1.000000000000000000, 0.9091211823109212053, 1.000000000000000000),
 ( 1.000000000000000000, 0.9165811874549500970, 1.000000000000000000),
 ( 1.000000000000000000, 0.9165151389911680990, 1.000000000000000000) ) ) 
 REPRESENTATION_ITEM ( '' )  SURFACE ( )  );
#14285 = CARTESIAN_POINT ( 'NONE',  ( 156.2961002691897079, 2.071067811865468400, -4.999999999999989342 ) ) ;
#14286 = FACE_OUTER_BOUND ( 'NONE', #5202, .T. ) ;
#14287 = ORIENTED_EDGE ( 'NONE', *, *, #20882, .F. ) ;
#14288 = UNCERTAINTY_MEASURE_WITH_UNIT (LENGTH_MEASURE( 1.000000000000000082E-05 ), #29826, 'distance_accuracy_value', 'NONE');
#14289 = CARTESIAN_POINT ( 'NONE',  ( 112.1249999999998437, 1.767766952966293159, 1.767766952966431937 ) ) ;
#14290 = CARTESIAN_POINT ( 'NONE',  ( 140.0000000000000284, 0.000000000000000000, 0.000000000000000000 ) ) ;
#14291 = EDGE_CURVE ( 'NONE', #25175, #3090, #22511, .T. ) ;
#14292 = CARTESIAN_POINT ( 'NONE',  ( 106.8127832217621602, -1.849990392679441875, 0.7662911109078888172 ) ) ;
#14293 = CARTESIAN_POINT ( 'NONE',  ( 153.0863248654052313, 0.000000000000000000, 5.500000000000005329 ) ) ;
#14294 = EDGE_CURVE ( 'NONE', #15655, #3485, #5245, .T. ) ;
#14295 = ORIENTED_EDGE ( 'NONE', *, *, #11513, .T. ) ;
#14296 = CARTESIAN_POINT ( 'NONE',  ( 15.27382486540527040, -2.499999999999844569, -1.035533905932809473 ) ) ;
#14297 = CARTESIAN_POINT ( 'NONE',  ( -2.081668171172168020E-16, -5.204170427930420051E-17, 2.499999999999999112 ) ) ;
#14298 = CARTESIAN_POINT ( 'NONE',  ( 106.9997167782376550, -1.308140751793612777, 1.308140751793640533 ) ) ;
#14299 = VERTEX_POINT ( 'NONE', #23402 ) ;
#14300 = CARTESIAN_POINT ( 'NONE',  ( -5.196152422706573404, -3.000000000000002665, -53.21132486540525264 ) ) ;
#14301 = VECTOR ( 'NONE', #16342, 1000.000000000000000 ) ;
#14302 = CARTESIAN_POINT ( 'NONE',  ( 152.6250000000000284, 0.000000000000000000, -6.000000000000005329 ) ) ;
#14303 = VERTEX_POINT ( 'NONE', #2348 ) ;
#14304 = CARTESIAN_POINT ( 'NONE',  ( -4.763139720814407951, -2.750000000000016431, -114.9999999999999858 ) ) ;
#14305 = CARTESIAN_POINT ( 'NONE',  ( 23.50000000000013145, 1.873492889145011997, 1.873492889144734441 ) ) ;
#14306 = CARTESIAN_POINT ( 'NONE',  ( 2.775557561562891351E-14, -6.250000000000061284, -124.1830127018922525 ) ) ;
#14307 = ORIENTED_EDGE ( 'NONE', *, *, #15085, .F. ) ;
#14308 = CARTESIAN_POINT ( 'NONE',  ( -7.216878364870328078, 0.000000000000000000, -170.1919872981078186 ) ) ;
#14309 = CARTESIAN_POINT ( 'NONE',  ( 109.7499999999999147, 5.551115123125782702E-14, -2.499999999999835687 ) ) ;
#14310 = PRESENTATION_STYLE_ASSIGNMENT (( #14166 ) ) ;
#14311 = ORIENTED_EDGE ( 'NONE', *, *, #1432, .T. ) ;
#14312 = CARTESIAN_POINT ( 'NONE',  ( 2.027308962376910273, 5.280605156494750929, -179.9999999999999716 ) ) ;
#14313 = CARTESIAN_POINT ( 'NONE',  ( 0.000000000000000000, 0.000000000000000000, 0.000000000000000000 ) ) ;
#14314 = CARTESIAN_POINT ( 'NONE',  ( 4.763139720814407951, -2.749999999999988454, -180.5000000000000000 ) ) ;
#14315 = CARTESIAN_POINT ( 'NONE',  ( 109.8127832217621034, -1.849990392679501827, 0.7662911109077686911 ) ) ;
#14316 = CARTESIAN_POINT ( 'NONE',  ( 3.608439182435180470, -6.249999999999997335, -175.0580127018922383 ) ) ;
#14317 = CARTESIAN_POINT ( 'NONE',  ( 6.000000000000000888, 7.762456499804235646E-14, -139.5863248654051745 ) ) ;
#14318 = LINE ( 'NONE', #21206, #9882 ) ;
#14319 = CIRCLE ( 'NONE', #2496, 13.00000000000000178 ) ;
#14320 = CARTESIAN_POINT ( 'NONE',  ( 159.2599382550154985, -11.07692307692306777, -4.615384615384606093 ) ) ;
#14321 = UNCERTAINTY_MEASURE_WITH_UNIT (LENGTH_MEASURE( 1.000000000000000082E-05 ), #24252, 'distance_accuracy_value', 'NONE');
#14322 = CARTESIAN_POINT ( 'NONE',  ( 0.000000000000000000, 5.499999999999991118, -115.5000000000000426 ) ) ;
#14323 = CARTESIAN_POINT ( 'NONE',  ( 135.0000000000000568, -8.453200966450170384, -7.964396152078529134 ) ) ;
#14324 = CARTESIAN_POINT ( 'NONE',  ( 6.000000000000000888, 1.607695154586715303, -146.0966878364870354 ) ) ;
#14325 = AXIS2_PLACEMENT_3D ( 'NONE', #855, #10554, #15341 ) ;
#14326 = VERTEX_POINT ( 'NONE', #21095 ) ;
#14327 = CARTESIAN_POINT ( 'NONE',  ( 17.93750000000014921, -1.097466725451439196, 2.649519052838178457 ) ) ;
#14328 = CARTESIAN_POINT ( 'NONE',  ( -0.07769256095283699759, -15.23231281889969679, -7.500000000000007105 ) ) ;
#14329 = CARTESIAN_POINT ( 'NONE',  ( -5.999999999999919176, 1.607695154586804565, -108.9033121635129930 ) ) ;
#14330 = CARTESIAN_POINT ( 'NONE',  ( 5.196152422706629359, 3.000000000000002665, -155.9613248654052597 ) ) ;
#14331 = ADVANCED_FACE ( 'NONE', ( #9410 ), #9717, .F. ) ;
#14332 = ORIENTED_EDGE ( 'NONE', *, *, #1895, .T. ) ;
#14333 = CARTESIAN_POINT ( 'NONE',  ( -3.175426480542816066, 5.499999999999865885, -178.3750000000000568 ) ) ;
#14334 =( BOUNDED_CURVE ( )  B_SPLINE_CURVE ( 2, ( #728, #24368, #24512, #1015, #21785, #863, #2875, #29113, #23937 ),
 .UNSPECIFIED., .F., .F. ) 
 B_SPLINE_CURVE_WITH_KNOTS ( ( 3, 2, 2, 2, 3 ),
 ( 0.5194444444444444864, 0.5203703703703703720, 0.5222222222222222543, 0.5240740740740740256, 0.5249999999999999112 ),
 .UNSPECIFIED. ) 
 CURVE ( )  GEOMETRIC_REPRESENTATION_ITEM ( )  RATIONAL_B_SPLINE_CURVE ( ( 0.9330127018922194093, 0.9330127018922234061, 1.000000000000000000, 0.8660254037844388186, 1.000000000000000000, 0.8660254037844388186, 1.000000000000000000, 0.9330127018922234061, 0.9330127018922194093 ) ) 
 REPRESENTATION_ITEM ( '' )  );
#14335 = CYLINDRICAL_SURFACE ( 'NONE', #30305, 6.000000000000000888 ) ;
#14336 = CARTESIAN_POINT ( 'NONE',  ( 156.7574251345948539, -2.278174593051826236, 5.500000000000198064 ) ) ;
#14337 = ORIENTED_EDGE ( 'NONE', *, *, #2686, .F. ) ;
#14338 = ORIENTED_EDGE ( 'NONE', *, *, #27746, .F. ) ;
#14339 = CARTESIAN_POINT ( 'NONE',  ( 137.8125000000000284, 4.242640687119298093, -4.242640687119298093 ) ) ;
#14340 = AXIS2_PLACEMENT_3D ( 'NONE', #27505, #20006, #1567 ) ;
#14341 = VERTEX_POINT ( 'NONE', #22290 ) ;
#14342 = CARTESIAN_POINT ( 'NONE',  ( 2.775557561562891351E-14, -6.250000000000061284, -141.3169872981078186 ) ) ;
#14343 = SURFACE_SIDE_STYLE ('',( #4914 ) ) ;
#14344 = VECTOR ( 'NONE', #22167, 1000.000000000000000 ) ;
#14345 = CARTESIAN_POINT ( 'NONE',  ( 10.00000000000003730, -1.873492889144789952, -1.873492889145123019 ) ) ;
#14346 = CARTESIAN_POINT ( 'NONE',  ( 6.000000000000000888, 7.762456499804234384E-14, -129.6636751345948255 ) ) ;
#14347 = CARTESIAN_POINT ( 'NONE',  ( 18.31249999999999289, -0.8284271247460552878, 2.000000000000031530 ) ) ;
#14348 = CARTESIAN_POINT ( 'NONE',  ( 117.3363248654050892, -1.414213562373256572, -1.414213562372923505 ) ) ;
#14349 = CARTESIAN_POINT ( 'NONE',  ( 137.5163997308104058, 4.999999999999989342, 2.071067811865468400 ) ) ;
#14350 = CARTESIAN_POINT ( 'NONE',  ( 5.999999999999949374, 1.607695154586804565, -99.59668783648702117 ) ) ;
#14351 = CARTESIAN_POINT ( 'NONE',  ( 0.000000000000000000, -5.999999999999991118, -70.03867513459482552 ) ) ;
#14352 = VECTOR ( 'NONE', #14468, 1000.000000000000000 ) ;
#14353 = ADVANCED_FACE ( 'NONE', ( #21838 ), #5824, .T. ) ;
#14354 = CARTESIAN_POINT ( 'NONE',  ( 156.1011751345948255, 3.889087296526011706, -3.889087296526011706 ) ) ;
#14355 = FILL_AREA_STYLE_COLOUR ( '', #4318 ) ;
#14356 = CARTESIAN_POINT ( 'NONE',  ( 107.5624999999998153, -2.499999999999874767, -1.035533905932629173 ) ) ;
#14357 = CARTESIAN_POINT ( 'NONE',  ( -6.000000000000000888, 1.067854986875958443E-15, 7.560779664488942560E-35 ) ) ;
#14358 = STYLED_ITEM ( 'NONE', ( #14892 ), #3422 ) ;
#14359 =( NAMED_UNIT ( * ) PLANE_ANGLE_UNIT ( ) SI_UNIT ( $, .RADIAN. ) );
#14360 =( NAMED_UNIT ( * ) SI_UNIT ( $, .STERADIAN. ) SOLID_ANGLE_UNIT ( ) );
#14361 = ORIENTED_EDGE ( 'NONE', *, *, #1090, .F. ) ;
#14362 = CARTESIAN_POINT ( 'NONE',  ( -3.464101615137757051, -5.999999999999979572, -107.0863248654051461 ) ) ;
#14363 = CARTESIAN_POINT ( 'NONE',  ( -3.464101615137725076, 5.999999999999979572, -52.66367513459479710 ) ) ;
#14364 = CARTESIAN_POINT ( 'NONE',  ( -5.999999999999964473, 9.063946212346262433E-15, -173.3363248654052597 ) ) ;
#14365 = CARTESIAN_POINT ( 'NONE',  ( -5.196152422706573404, -3.000000000000002665, -179.2113248654052597 ) ) ;
#14366 = ORIENTED_EDGE ( 'NONE', *, *, #19654, .T. ) ;
#14367 = CARTESIAN_POINT ( 'NONE',  ( 118.4997167782374135, 1.308140751793696044, -1.308140751793640533 ) ) ;
#14368 = CARTESIAN_POINT ( 'NONE',  ( 141.9375000000000284, -4.242640687119298093, -4.242640687119298093 ) ) ;
#14369 = CARTESIAN_POINT ( 'NONE',  ( 7.216878364870455975, -6.409875621278545621E-14, -103.4419872981078328 ) ) ;
#14370 = CARTESIAN_POINT ( 'NONE',  ( 138.5550748654052313, -5.500000000000012434, -2.278174593052012309 ) ) ;
#14371 =( BOUNDED_CURVE ( )  B_SPLINE_CURVE ( 2, ( #7304, #522, #9915, #9763, #21288, #16708, #4977, #28615, #19138 ),
 .UNSPECIFIED., .F., .T. ) 
 B_SPLINE_CURVE_WITH_KNOTS ( ( 3, 2, 2, 2, 3 ),
 ( 0.8235294117647058432, 0.8308823529411764053, 0.8382352941176470784, 0.8455882352941176405, 0.8529411764705882026 ),
 .UNSPECIFIED. ) 
 CURVE ( )  GEOMETRIC_REPRESENTATION_ITEM ( )  RATIONAL_B_SPLINE_CURVE ( ( 1.000000000000000000, 0.9238795325112867385, 1.000000000000000000, 0.9238795325112867385, 1.000000000000000000, 0.9238795325112867385, 1.000000000000000000, 0.9238795325112867385, 1.000000000000000000 ) ) 
 REPRESENTATION_ITEM ( '' )  );
#14372 = CARTESIAN_POINT ( 'NONE',  ( 161.1413997308104058, 2.071067811865468400, -4.999999999999989342 ) ) ;
#14373 = CARTESIAN_POINT ( 'NONE',  ( 116.7499999999997584, 1.665334536937734811E-13, -2.499999999999724665 ) ) ;
#14374 = VECTOR ( 'NONE', #2589, 1000.000000000000000 ) ;
#14375 = CARTESIAN_POINT ( 'NONE',  ( 4.763139720814407951, 2.750000000000002665, -127.7500000000000284 ) ) ;
#14376 = ORIENTED_EDGE ( 'NONE', *, *, #28341, .T. ) ;
#14377 = EDGE_LOOP ( 'NONE', ( #22574, #28735, #1325 ) ) ;
#14378 = CARTESIAN_POINT ( 'NONE',  ( 5.999999999999949374, 1.607695154586804565, -81.59668783648703538 ) ) ;
#14379 = CARTESIAN_POINT ( 'NONE',  ( 3.175426480543072749, -5.500000000000105693, -60.62500000000000000 ) ) ;
#14380 = CARTESIAN_POINT ( 'NONE',  ( 135.0000000000000284, 0.000000000000000000, 0.000000000000000000 ) ) ;
#14381 = CARTESIAN_POINT ( 'NONE',  ( 109.2261751345945697, 2.000000000000122125, -0.8284271247459952248 ) ) ;
#14382 = CARTESIAN_POINT ( 'NONE',  ( 2.775557561562891351E-14, 6.250000000000033751, -79.93301270189223828 ) ) ;
#14383 = PRODUCT_DEFINITION_CONTEXT ( 'detailed design', #21649, 'design' ) ;
#14384 = DIRECTION ( 'NONE',  ( 0.000000000000000000, 0.000000000000000000, 1.000000000000000000 ) ) ;
#14385 = CIRCLE ( 'NONE', #5856, 6.000000000000000888 ) ;
#14386 = EDGE_CURVE ( 'NONE', #21660, #5195, #8391, .T. ) ;
#14387 = CARTESIAN_POINT ( 'NONE',  ( 106.9372167782374703, -0.7662911109076785410, 1.849990392679772278 ) ) ;
#14388 = FACE_OUTER_BOUND ( 'NONE', #15010, .T. ) ;
#14389 = CARTESIAN_POINT ( 'NONE',  ( 113.6252832217621460, 1.665334536937734811E-13, 1.849990392679745632 ) ) ;
#14390 = CARTESIAN_POINT ( 'NONE',  ( -2.775557561562891351E-14, -5.500000000000115463, -137.2499999999999716 ) ) ;
#14391 = CARTESIAN_POINT ( 'NONE',  ( 6.000000000000000888, 1.743066579297358182E-13, -57.08632486540521001 ) ) ;
#14392 = CARTESIAN_POINT ( 'NONE',  ( -3.608439182435052128, -6.250000000000110134, -151.3080127018922099 ) ) ;
#14393 = CARTESIAN_POINT ( 'NONE',  ( -3.464101615137725076, 5.999999999999979572, -116.5863248654052171 ) ) ;
#14394 = CARTESIAN_POINT ( 'NONE',  ( -5.999999999999963585, 1.780251999655701777E-13, -89.33632486540523132 ) ) ;
#14395 = CARTESIAN_POINT ( 'NONE',  ( 3.175426480543072749, -5.500000000000105693, -77.12500000000001421 ) ) ;
#14396 = CARTESIAN_POINT ( 'NONE',  ( -5.999999999999971578, 1.607695154586715303, -113.9806624327025872 ) ) ;
#14397 = CARTESIAN_POINT ( 'NONE',  ( -5.999999999999964473, 9.063946212346262433E-15, -173.3363248654052597 ) ) ;
#14398 = EDGE_CURVE ( 'NONE', #3651, #10998, #1930, .T. ) ;
#14399 = CARTESIAN_POINT ( 'NONE',  ( -3.175426480542816510, 5.499999999999865885, -64.37500000000001421 ) ) ;
#14400 = EDGE_CURVE ( 'NONE', #14144, #2147, #11587, .T. ) ;
#14401 = LINE ( 'NONE', #21131, #4507 ) ;
#14402 = CARTESIAN_POINT ( 'NONE',  ( 145.6086002691897079, -2.071067811865468400, -4.999999999999989342 ) ) ;
#14403 = CARTESIAN_POINT ( 'NONE',  ( 104.9999999999998863, -0.4876318259229017738, -1.939643060551943243 ) ) ;
#14404 = CARTESIAN_POINT ( 'NONE',  ( 159.5625000000000284, -4.242640687119298093, 4.242640687119298093 ) ) ;
#14405 = DIRECTION ( 'NONE',  ( -8.326672684688675286E-17, -2.081668171172168821E-17, 1.000000000000000000 ) ) ;
#14406 = CARTESIAN_POINT ( 'NONE',  ( -5.196152422706573404, -3.000000000000002665, -50.21132486540524553 ) ) ;
#14407 = CARTESIAN_POINT ( 'NONE',  ( 0.000000000000000000, 0.000000000000000000, 0.000000000000000000 ) ) ;
#14408 = CARTESIAN_POINT ( 'NONE',  ( 115.5622167782373850, 1.849990392679532247, -0.7662911109075883909 ) ) ;
#14409 = CARTESIAN_POINT ( 'NONE',  ( -5.999999999999919176, 1.607695154586804565, -81.90331216351300725 ) ) ;
#14410 = ORIENTED_EDGE ( 'NONE', *, *, #13583, .F. ) ;
#14411 = CARTESIAN_POINT ( 'NONE',  ( 149.1562500000000284, -6.000000000000005329, 2.485281374238555774 ) ) ;
#14412 = CARTESIAN_POINT ( 'NONE',  ( 114.8127832217620465, -1.849990392679591977, 0.7662911109078888172 ) ) ;
#14413 = FACE_OUTER_BOUND ( 'NONE', #19832, .T. ) ;
#14414 = CARTESIAN_POINT ( 'NONE',  ( 20.81250000000013856, 0.8284271247461753029, -2.000000000000091926 ) ) ;
#14415 = ORIENTED_EDGE ( 'NONE', *, *, #22680, .F. ) ;
#14416 = CARTESIAN_POINT ( 'NONE',  ( 6.350852961086080661, -9.614813431917819062E-14, -87.37500000000007105 ) ) ;
#14417 = CARTESIAN_POINT ( 'NONE',  ( 5.412658773652712085, -3.125000000000086153, -101.4330127018922525 ) ) ;
#14418 = CARTESIAN_POINT ( 'NONE',  ( -6.000000000000000888, 1.067854986875958443E-15, 7.560779664488942560E-35 ) ) ;
#14419 = CARTESIAN_POINT ( 'NONE',  ( 153.6413997308104342, 2.071067811865468400, -4.999999999999989342 ) ) ;
#14420 = EDGE_CURVE ( 'NONE', #12934, #22336, #29827, .T. ) ;
#14421 = CARTESIAN_POINT ( 'NONE',  ( 110.7886751345946834, -1.999999999999946265, 0.000000000000000000 ) ) ;
#14422 = CARTESIAN_POINT ( 'NONE',  ( -5.196152422706601826, 2.999999999999975131, -58.53867513459481842 ) ) ;
#14423 = CARTESIAN_POINT ( 'NONE',  ( 135.6059727065548941, -8.864963804575562989, 8.000000000000007105 ) ) ;
#14424 = SURFACE_STYLE_FILL_AREA ( #25751 ) ;
#14425 = AXIS2_PLACEMENT_3D ( 'NONE', #14205, #5369, #28417 ) ;
#14426 = CARTESIAN_POINT ( 'NONE',  ( -3.175426480542816066, -5.500000000000057732, -162.8750000000000568 ) ) ;
#14427 = CARTESIAN_POINT ( 'NONE',  ( -5.196152422706601826, 2.999999999999975131, -57.96132486540523132 ) ) ;
#14428 = CARTESIAN_POINT ( 'NONE',  ( 3.175426480543072749, -5.500000000000105693, -155.1250000000000000 ) ) ;
#14429 = CARTESIAN_POINT ( 'NONE',  ( 113.6249999999998721, -1.767766952966376426, -1.767766952966431937 ) ) ;
#14430 = CARTESIAN_POINT ( 'NONE',  ( -3.175426480542816066, -5.500000000000057732, -102.8750000000000142 ) ) ;
#14431 = CARTESIAN_POINT ( 'NONE',  ( 142.4925748654052313, 2.278174593052074925, 5.499999999999950262 ) ) ;
#14432 = CARTESIAN_POINT ( 'NONE',  ( 6.000000000000000888, 7.762456499804235646E-14, -121.5863248654052455 ) ) ;
#14433 = ADVANCED_FACE ( 'NONE', ( #3523 ), #28717, .T. ) ;
#14434 = CARTESIAN_POINT ( 'NONE',  ( 3.175426480543072749, 5.499999999999865885, -90.12500000000001421 ) ) ;
#14435 = CARTESIAN_POINT ( 'NONE',  ( 156.9523502691896510, 0.000000000000000000, 5.000000000000004441 ) ) ;
#14436 = CARTESIAN_POINT ( 'NONE',  ( 141.6636751345948255, 0.000000000000000000, 5.500000000000005329 ) ) ;
#14437 = CARTESIAN_POINT ( 'NONE',  ( 109.5238248654049471, 0.8284271247463257382, -1.999999999999791278 ) ) ;
#14438 = CARTESIAN_POINT ( 'NONE',  ( 112.5624999999998010, -2.499999999999994671, -1.035533905932689347 ) ) ;
#14439 = CARTESIAN_POINT ( 'NONE',  ( -3.464101615137757051, -5.999999999999979572, -66.58632486540523132 ) ) ;
#14440 = CARTESIAN_POINT ( 'NONE',  ( 106.7502832217622597, -1.308140751793529510, 1.308140751793973600 ) ) ;
#14441 = CARTESIAN_POINT ( 'NONE',  ( -5.999999999999919176, 1.607695154586804565, -77.98066243270260145 ) ) ;
#14442 = ORIENTED_EDGE ( 'NONE', *, *, #7435, .F. ) ;
#14443 = DIRECTION ( 'NONE',  ( 1.000000000000000000, -5.551115123125773458E-17, -1.260129944081490338E-35 ) ) ;
#14444 = CARTESIAN_POINT ( 'NONE',  ( 107.2497167782375129, -1.308140751793585022, -1.308140751793640533 ) ) ;
#14445 = AXIS2_PLACEMENT_3D ( 'NONE', #28194, #25277, #23910 ) ;
#14446 = CARTESIAN_POINT ( 'NONE',  ( 146.0625000000000284, -4.242640687119298093, 4.242640687119298093 ) ) ;
#14447 = CARTESIAN_POINT ( 'NONE',  ( 4.763139720814407951, -2.749999999999988454, -114.5000000000000426 ) ) ;
#14448 = CARTESIAN_POINT ( 'NONE',  ( 17.37500000000000000, 2.649519052838500421, 0.000000000000000000 ) ) ;
#14449 = CARTESIAN_POINT ( 'NONE',  ( -7.216878364870328078, 0.000000000000000000, -120.0580127018922525 ) ) ;
#14450 = ORIENTED_EDGE ( 'NONE', *, *, #19695, .T. ) ;
#14451 = CARTESIAN_POINT ( 'NONE',  ( 158.4300748654052313, 2.278174593051857766, -5.500000000000166978 ) ) ;
#14452 = CARTESIAN_POINT ( 'NONE',  ( 2.775557561562891351E-14, -6.250000000000061284, -163.8169872981078470 ) ) ;
#14453 = CARTESIAN_POINT ( 'NONE',  ( 108.6249999999999289, -1.767766952966320915, -1.767766952966320915 ) ) ;
#14454 = ADVANCED_FACE ( 'NONE', ( #5375 ), #15082, .F. ) ;
#14455 = EDGE_LOOP ( 'NONE', ( #3722, #26999, #14916, #24475 ) ) ;
#14456 = CARTESIAN_POINT ( 'NONE',  ( 0.2071745301884423129, -15.61907693555130905, -7.893511971080271472 ) ) ;
#14457 = EDGE_CURVE ( 'NONE', #26998, #27478, #18661, .T. ) ;
#14458 =( BOUNDED_CURVE ( )  B_SPLINE_CURVE ( 2, ( #19842, #24289, #7709, #24756, #12663, #13126, #29043, #17116, #22464 ),
 .UNSPECIFIED., .F., .T. ) 
 B_SPLINE_CURVE_WITH_KNOTS ( ( 3, 2, 2, 2, 3 ),
 ( 0.6805555555555555802, 0.6814814814814814659, 0.6833333333333333481, 0.6851851851851851194, 0.6861111111111111160 ),
 .UNSPECIFIED. ) 
 CURVE ( )  GEOMETRIC_REPRESENTATION_ITEM ( )  RATIONAL_B_SPLINE_CURVE ( ( 0.9330127018922194093, 0.9330127018922234061, 1.000000000000000000, 0.8660254037844388186, 1.000000000000000000, 0.8660254037844388186, 1.000000000000000000, 0.9330127018922194093, 0.9330127018922194093 ) ) 
 REPRESENTATION_ITEM ( '' )  );
#14459 = DIRECTION ( 'NONE',  ( 1.000000000000000000, -5.551115123125773458E-17, -1.260129944081490338E-35 ) ) ;
#14460 = CYLINDRICAL_SURFACE ( 'NONE', #12878, 6.000000000000000888 ) ;
#14461 = CARTESIAN_POINT ( 'NONE',  ( 0.000000000000000000, 5.499999999999991118, -180.0000000000000568 ) ) ;
#14462 = CARTESIAN_POINT ( 'NONE',  ( 106.1252832217622171, -5.551115123125782702E-14, -1.849990392679523588 ) ) ;
#14463 = CARTESIAN_POINT ( 'NONE',  ( 15.00000000000000000, 0.000000000000000000, 0.000000000000000000 ) ) ;
#14464 = CARTESIAN_POINT ( 'NONE',  ( 7.216878364870455975, -6.409875621278545621E-14, -177.8080127018922667 ) ) ;
#14465 = CARTESIAN_POINT ( 'NONE',  ( 116.0000000000000142, 6.735557395310442023E-16, 5.500000000000000000 ) ) ;
#14466 = SURFACE_STYLE_USAGE ( .BOTH. , #289 ) ;
#14467 = CARTESIAN_POINT ( 'NONE',  ( 6.350852961086080661, -9.614813431917819062E-14, -124.8749999999999858 ) ) ;
#14468 = DIRECTION ( 'NONE',  ( -1.000000000000000000, 0.000000000000000000, 0.000000000000000000 ) ) ;
#14469 = CARTESIAN_POINT ( 'NONE',  ( 0.000000000000000000, 5.499999999999991118, -117.0000000000000000 ) ) ;
#14470 = DIRECTION ( 'NONE',  ( -7.147005652999508048E-36, 5.642372883946980038E-36, 1.000000000000000000 ) ) ;
#14471 = ORIENTED_EDGE ( 'NONE', *, *, #1400, .T. ) ;
#14472 = CARTESIAN_POINT ( 'NONE',  ( 16.75000000000001421, 1.873492889145011997, 1.873492889144845464 ) ) ;
#14473 = CARTESIAN_POINT ( 'NONE',  ( 6.000000000000000000, 2.951592740943527306E-14, -150.6636751345948539 ) ) ;
#14474 = CARTESIAN_POINT ( 'NONE',  ( 5.196152422706629359, -2.999999999999988898, -136.7113248654052029 ) ) ;
#14475 = CARTESIAN_POINT ( 'NONE',  ( -5.196152422706601826, 2.999999999999975131, -155.4613248654052029 ) ) ;
#14476 = CARTESIAN_POINT ( 'NONE',  ( 5.999999999999949374, 1.607695154586804565, -87.01933756729741276 ) ) ;
#14477 = EDGE_LOOP ( 'NONE', ( #8582, #22886, #7448, #8139 ) ) ;
#14478 = CARTESIAN_POINT ( 'NONE',  ( 3.464101615137757051, -5.999999999999979572, -126.3363248654051887 ) ) ;
#14479 = CARTESIAN_POINT ( 'NONE',  ( -3.175426480542417718, 5.500000000000556000, -179.8750000000000853 ) ) ;
#14480 = CARTESIAN_POINT ( 'NONE',  ( 0.000000000000000000, 0.000000000000000000, 0.000000000000000000 ) ) ;
#14481 = EDGE_LOOP ( 'NONE', ( #2464, #27267, #23750, #22037 ) ) ;
#14482 = CARTESIAN_POINT ( 'NONE',  ( 5.196152422706629359, -2.999999999999988898, -125.2886751345948539 ) ) ;
#14483 = ORIENTED_EDGE ( 'NONE', *, *, #17047, .T. ) ;
#14484 = VERTEX_POINT ( 'NONE', #18157 ) ;
#14485 = CARTESIAN_POINT ( 'NONE',  ( 21.03867513459492500, 1.665334536937734811E-13, -2.500000000000002220 ) ) ;
#14486 = CARTESIAN_POINT ( 'NONE',  ( 134.6398502691896510, -3.535533905932752852, 3.535533905932725318 ) ) ;
#14487 = VERTEX_POINT ( 'NONE', #13560 ) ;
#14488 = CARTESIAN_POINT ( 'NONE',  ( 3.608439182435180470, 6.249999999999982236, -139.1919872981078470 ) ) ;
#14489 = CARTESIAN_POINT ( 'NONE',  ( 24.02382486540523487, -1.035533905932689347, 2.499999999999964473 ) ) ;
#14490 = CARTESIAN_POINT ( 'NONE',  ( -5.196152422706601826, 2.999999999999975131, -174.9613248654052313 ) ) ;
#14491 = CARTESIAN_POINT ( 'NONE',  ( -5.999999999999971578, 1.607695154586715303, -128.9806624327026441 ) ) ;
#14492 = EDGE_LOOP ( 'NONE', ( #12361, #24782, #8854, #9871 ) ) ;
#14493 = CARTESIAN_POINT ( 'NONE',  ( 19.43750000000013145, -1.999999999999851674, 0.8284271247462354770 ) ) ;
#14494 = LINE ( 'NONE', #28410, #12769 ) ;
#14495 = CARTESIAN_POINT ( 'NONE',  ( -5.999999999999963585, -1.487416814333745711E-14, -66.83632486540523132 ) ) ;
#14496 = EDGE_CURVE ( 'NONE', #8469, #16412, #1755, .T. ) ;
#14497 = CARTESIAN_POINT ( 'NONE',  ( 140.5163997308104342, 4.999999999999989342, 2.071067811865468400 ) ) ;
#14498 = LINE ( 'NONE', #22237, #24133 ) ;
#14499 = CARTESIAN_POINT ( 'NONE',  ( 12.27382486540534146, -2.499999999999784173, -1.035533905932809473 ) ) ;
#14500 = CARTESIAN_POINT ( 'NONE',  ( -5.999999999999971578, 1.607695154586715303, -59.98066243270260856 ) ) ;
#14501 = CARTESIAN_POINT ( 'NONE',  ( 106.3124999999997584, -1.035533905932659149, 2.500000000000205169 ) ) ;
#14502 = CYLINDRICAL_SURFACE ( 'NONE', #18598, 0.5000000000000000000 ) ;
#14503 = VERTEX_POINT ( 'NONE', #13260 ) ;
#14504 = CARTESIAN_POINT ( 'NONE',  ( -4.763139720814407951, -2.750000000000016431, -49.00000000000004263 ) ) ;
#14505 = CARTESIAN_POINT ( 'NONE',  ( 6.000000000000000888, 1.607695154586715303, -79.51933756729744118 ) ) ;
#14506 = ORIENTED_EDGE ( 'NONE', *, *, #16711, .T. ) ;
#14507 = CARTESIAN_POINT ( 'NONE',  ( 118.5622167782375698, 1.849990392679621953, -0.7662911109077087390 ) ) ;
#14508 =( NAMED_UNIT ( * ) PLANE_ANGLE_UNIT ( ) SI_UNIT ( $, .RADIAN. ) );
#14509 = CARTESIAN_POINT ( 'NONE',  ( -7.216878364870328078, 0.000000000000000000, -107.1919872981078612 ) ) ;
#14510 = CARTESIAN_POINT ( 'NONE',  ( -5.999999999999956479, -1.607695154586745057, -50.84668783648707091 ) ) ;
#14511 = CARTESIAN_POINT ( 'NONE',  ( 133.7812500000000284, 2.485281374238585972, 6.000000000000005329 ) ) ;
#14512 = CARTESIAN_POINT ( 'NONE',  ( 117.3750000000000142, -1.767766952966320915, 1.767766952966431937 ) ) ;
#14513 = ADVANCED_FACE ( 'NONE', ( #1534 ), #15720, .F. ) ;
#14514 = CARTESIAN_POINT ( 'NONE',  ( 4.763139720814407951, 2.750000000000002665, -132.2500000000000284 ) ) ;
#14515 = ORIENTED_EDGE ( 'NONE', *, *, #24632, .T. ) ;
#14516 = AXIS2_PLACEMENT_3D ( 'NONE', #8685, #23292, #25099 ) ;
#14517 = VERTEX_POINT ( 'NONE', #29641 ) ;
#14518 = CARTESIAN_POINT ( 'NONE',  ( -3.464101615137725076, 5.999999999999979572, -96.16367513459479710 ) ) ;
#14519 = CIRCLE ( 'NONE', #9584, 17.50000000000000355 ) ;
#14520 = CARTESIAN_POINT ( 'NONE',  ( 6.350852961086080661, -9.614813431917819062E-14, -60.37500000000000000 ) ) ;
#14521 = CARTESIAN_POINT ( 'NONE',  ( -5.196152422706601826, 2.999999999999975131, -115.5386751345948113 ) ) ;
#14522 = CARTESIAN_POINT ( 'NONE',  ( 160.0000000000000568, -12.58734212865233459, -3.130219457110984926 ) ) ;
#14523 = CARTESIAN_POINT ( 'NONE',  ( -7.216878364870328078, 0.000000000000000000, -81.05801270189220986 ) ) ;
#14524 = ADVANCED_FACE ( 'NONE', ( #20294 ), #8606, .T. ) ;
#14525 = CARTESIAN_POINT ( 'NONE',  ( 3.464101615137852974, 5.999999999999884537, -149.8363248654051176 ) ) ;
#14526 = CARTESIAN_POINT ( 'NONE',  ( 105.3122167782374277, -0.7662911109076785410, -1.849990392679231599 ) ) ;
#14527 = CARTESIAN_POINT ( 'NONE',  ( 113.7502832217623023, -1.308140751793585022, 1.308140751793640533 ) ) ;
#14528 = CARTESIAN_POINT ( 'NONE',  ( 4.763139720814407951, 2.750000000000002665, -138.2499999999999716 ) ) ;
#14529 = CARTESIAN_POINT ( 'NONE',  ( 139.9468100150023702, -9.635049468574379716, 7.732362477259529854 ) ) ;
#14530 = CARTESIAN_POINT ( 'NONE',  ( 2.775557561562891351E-14, 6.250000000000033751, -150.4330127018922383 ) ) ;
#14531 = CARTESIAN_POINT ( 'NONE',  ( -3.175426480542816066, -5.500000000000057732, -69.87500000000004263 ) ) ;
#14532 = CARTESIAN_POINT ( 'NONE',  ( 144.9300748654052029, 2.278174593051733421, -5.500000000000292211 ) ) ;
#14533 = CARTESIAN_POINT ( 'NONE',  ( 3.175426480543072749, -5.500000000000105693, -68.12500000000002842 ) ) ;
#14534 =( BOUNDED_CURVE ( )  B_SPLINE_CURVE ( 2, ( #5286, #12262, #16012, #385, #16164, #6746, #27769, #14557, #19154 ),
 .UNSPECIFIED., .F., .T. ) 
 B_SPLINE_CURVE_WITH_KNOTS ( ( 3, 2, 2, 2, 3 ),
 ( 0.9416666666666666519, 0.9425925925925925375, 0.9444444444444444198, 0.9462962962962963021, 0.9472222222222221877 ),
 .UNSPECIFIED. ) 
 CURVE ( )  GEOMETRIC_REPRESENTATION_ITEM ( )  RATIONAL_B_SPLINE_CURVE ( ( 0.9330127018922194093, 0.9330127018922194093, 1.000000000000000000, 0.8660254037844388186, 1.000000000000000000, 0.8660254037844388186, 1.000000000000000000, 0.9330127018922234061, 0.9330127018922194093 ) ) 
 REPRESENTATION_ITEM ( '' )  );
#14535 = CARTESIAN_POINT ( 'NONE',  ( 144.0148502691896510, -3.535533905932725318, -3.535533905932725318 ) ) ;
#14536 = CARTESIAN_POINT ( 'NONE',  ( 108.4136751345946692, 1.414213562373201061, 1.414213562373256572 ) ) ;
#14537 = CARTESIAN_POINT ( 'NONE',  ( 150.7500000000000284, -6.000000000000005329, 0.000000000000000000 ) ) ;
#14538 = CARTESIAN_POINT ( 'NONE',  ( -5.999999999999963585, -1.487416814333745711E-14, -133.4136751345948255 ) ) ;
#14539 = CARTESIAN_POINT ( 'NONE',  ( 18.12500000000000355, 1.414213562373090038, 1.414213562373090038 ) ) ;
#14540 = COLOUR_RGB ( '', 0.31764706, 0.68627451, 0.89019608) ;
#14541 = CARTESIAN_POINT ( 'NONE',  ( 5.196152422706629359, -2.999999999999988898, -147.2113248654052313 ) ) ;
#14542 = CARTESIAN_POINT ( 'NONE',  ( 116.0000000000000142, 0.000000000000000000, 0.000000000000000000 ) ) ;
#14543 = EDGE_LOOP ( 'NONE', ( #20912, #23921, #30406, #10118 ) ) ;
#14544 = CARTESIAN_POINT ( 'NONE',  ( 150.9375000000000284, -4.242640687119298093, -4.242640687119298093 ) ) ;
#14545 = CARTESIAN_POINT ( 'NONE',  ( 112.8752832217622029, -1.849990392679384810, 0.000000000000000000 ) ) ;
#14546 = EDGE_CURVE ( 'NONE', #23883, #19083, #15876, .T. ) ;
#14547 = CARTESIAN_POINT ( 'NONE',  ( 5.196152422706629359, -2.999999999999988898, -102.2113248654051887 ) ) ;
#14548 = CARTESIAN_POINT ( 'NONE',  ( -4.763139720814407951, 2.749999999999946709, -179.7500000000000284 ) ) ;
#14549 = CARTESIAN_POINT ( 'NONE',  ( 21.93750000000006395, 2.000000000000212275, -0.8284271247462955401 ) ) ;
#14550 = CARTESIAN_POINT ( 'NONE',  ( -5.412658773652684552, -3.125000000000099920, -152.0669872981078470 ) ) ;
#14551 = VERTEX_POINT ( 'NONE', #292 ) ;
#14552 = CARTESIAN_POINT ( 'NONE',  ( 0.000000000000000000, 5.499999999999991118, -81.00000000000001421 ) ) ;
#14553 = EDGE_CURVE ( 'NONE', #1699, #12019, #28085, .T. ) ;
#14554 = CARTESIAN_POINT ( 'NONE',  ( -5.412658773652739619, 3.124999999999975131, -99.18301270189222407 ) ) ;
#14555 = ORIENTED_EDGE ( 'NONE', *, *, #11178, .F. ) ;
#14556 = CARTESIAN_POINT ( 'NONE',  ( 107.7261751345945839, -1.999999999999941602, 0.8284271247462955401 ) ) ;
#14557 = CARTESIAN_POINT ( 'NONE',  ( -5.999999999999919176, 1.607695154586804565, -53.98066243270259434 ) ) ;
#14558 = CARTESIAN_POINT ( 'NONE',  ( 3.464101615137852974, 5.999999999999884537, -58.91367513459482552 ) ) ;
#14559 = DIRECTION ( 'NONE',  ( -1.000000000000000000, -5.551115123125765446E-17, -2.220446049250314560E-16 ) ) ;
#14560 = FACE_OUTER_BOUND ( 'NONE', #4021, .T. ) ;
#14561 = CARTESIAN_POINT ( 'NONE',  ( -3.175426480542816066, -5.500000000000057732, -167.3750000000000568 ) ) ;
#14562 = CARTESIAN_POINT ( 'NONE',  ( -6.350852961085760029, -1.281975124255709124E-13, -155.6249999999999716 ) ) ;
#14563 = DIRECTION ( 'NONE',  ( 0.000000000000000000, 1.000000000000000000, 0.000000000000000000 ) ) ;
#14564 = CARTESIAN_POINT ( 'NONE',  ( -6.350852961085760029, -1.281975124255709124E-13, -97.12500000000004263 ) ) ;
#14565 = CARTESIAN_POINT ( 'NONE',  ( 3.175426480543072749, 5.499999999999865885, -91.62500000000001421 ) ) ;
#14566 = CARTESIAN_POINT ( 'NONE',  ( 156.2023502691896510, 0.000000000000000000, -5.000000000000004441 ) ) ;
#14567 = CARTESIAN_POINT ( 'NONE',  ( 6.000000000000000888, -1.859271017917181981E-14, -135.6636751345948255 ) ) ;
#14568 = CARTESIAN_POINT ( 'NONE',  ( 23.56250000000009948, -1.999999999999851674, -0.8284271247462354770 ) ) ;
#14569 = CARTESIAN_POINT ( 'NONE',  ( 113.3124999999997300, -1.035533905932598975, 2.500000000000144773 ) ) ;
#14570 = CARTESIAN_POINT ( 'NONE',  ( 0.000000000000000000, 0.000000000000000000, 0.000000000000000000 ) ) ;
#14571 = CARTESIAN_POINT ( 'NONE',  ( 20.41367513459496763, 1.767766952966487448, 1.767766952966209892 ) ) ;
#14572 = ORIENTED_EDGE ( 'NONE', *, *, #19622, .T. ) ;
#14573 = SURFACE_SIDE_STYLE ('',( #12284 ) ) ;
#14574 = FACE_OUTER_BOUND ( 'NONE', #2633, .T. ) ;
#14575 = CARTESIAN_POINT ( 'NONE',  ( 104.5622167782374703, 1.849990392679501827, -0.7662911109076485650 ) ) ;
#14576 = EDGE_CURVE ( 'NONE', #7022, #28218, #5039, .T. ) ;
#14577 = ORIENTED_EDGE ( 'NONE', *, *, #9039, .F. ) ;
#14578 = CARTESIAN_POINT ( 'NONE',  ( 146.4375000000000284, -4.242640687119298093, -4.242640687119298093 ) ) ;
#14579 = CARTESIAN_POINT ( 'NONE',  ( 4.763139720814407951, 2.750000000000002665, -108.2500000000000142 ) ) ;
#14580 =( GEOMETRIC_REPRESENTATION_CONTEXT ( 3 ) GLOBAL_UNCERTAINTY_ASSIGNED_CONTEXT ( ( #14685 ) ) GLOBAL_UNIT_ASSIGNED_CONTEXT ( ( #5563, #5414, #24020 ) ) REPRESENTATION_CONTEXT ( 'NONE', 'WORKASPACE' ) );
#14581 = CARTESIAN_POINT ( 'NONE',  ( 18.87500000000011369, -2.649519052838111843, 0.000000000000000000 ) ) ;
#14582 = EDGE_CURVE ( 'NONE', #26402, #15213, #9037, .T. ) ;
#14583 = CARTESIAN_POINT ( 'NONE',  ( 3.608439182435180470, -6.249999999999997335, -122.5580127018922667 ) ) ;
#14584 = UNCERTAINTY_MEASURE_WITH_UNIT (LENGTH_MEASURE( 1.000000000000000082E-05 ), #913, 'distance_accuracy_value', 'NONE');
#14585 = VERTEX_POINT ( 'NONE', #19069 ) ;
#14586 = CARTESIAN_POINT ( 'NONE',  ( 6.000000000000000888, -1.859271017917181981E-14, -68.16367513459481131 ) ) ;
#14587 = CARTESIAN_POINT ( 'NONE',  ( 3.608439182435180470, -6.249999999999997335, -162.1919872981078754 ) ) ;
#14588 = CARTESIAN_POINT ( 'NONE',  ( 109.4999999999998579, -2.499999999999891198, 2.220446049250313081E-13 ) ) ;
#14589 = AXIS2_PLACEMENT_3D ( 'NONE', #6472, #29512, #13897 ) ;
#14590 = CARTESIAN_POINT ( 'NONE',  ( 0.000000000000000000, -9.500000000000008882, 5.000000000000004441 ) ) ;
#14591 = CARTESIAN_POINT ( 'NONE',  ( 2.775557561562891351E-14, 6.250000000000033751, -63.43301270189222407 ) ) ;
#14592 = ORIENTED_EDGE ( 'NONE', *, *, #647, .T. ) ;
#14593 = CARTESIAN_POINT ( 'NONE',  ( 15.46132486540530238, 1.110223024625156540E-13, -2.500000000000057732 ) ) ;
#14594 = FACE_OUTER_BOUND ( 'NONE', #8060, .T. ) ;
#14595 = CARTESIAN_POINT ( 'NONE',  ( 4.763139720814407951, -2.749999999999988454, -179.0000000000000568 ) ) ;
#14596 = CARTESIAN_POINT ( 'NONE',  ( 106.6877832217621602, -0.7662911109076785410, 1.849990392679712103 ) ) ;
#14597 = CARTESIAN_POINT ( 'NONE',  ( 0.000000000000000000, -5.999999999999991118, -169.0386751345947971 ) ) ;
#14598 = CARTESIAN_POINT ( 'NONE',  ( 7.216878364870455975, -6.409875621278545621E-14, -179.3080127018922667 ) ) ;
#14599 = DIRECTION ( 'NONE',  ( 1.000000000000000000, -0.000000000000000000, -0.000000000000000000 ) ) ;
#14600 = CARTESIAN_POINT ( 'NONE',  ( 6.000000000000000888, 1.743066579297358182E-13, -48.08632486540521711 ) ) ;
#14601 = CARTESIAN_POINT ( 'NONE',  ( 0.000000000000000000, 5.499999999999991118, -115.5000000000000426 ) ) ;
#14602 = CARTESIAN_POINT ( 'NONE',  ( 5.196152422706629359, 3.000000000000002665, -84.53867513459483973 ) ) ;
#14603 = CARTESIAN_POINT ( 'NONE',  ( 3.175426480543072749, 5.499999999999865885, -109.6249999999999716 ) ) ;
#14604 = DIRECTION ( 'NONE',  ( 1.000000000000000000, 0.000000000000000000, 0.000000000000000000 ) ) ;
#14605 = ORIENTED_EDGE ( 'NONE', *, *, #5819, .F. ) ;
#14606 = CARTESIAN_POINT ( 'NONE',  ( 19.12500000000003197, -2.649519052838111843, -5.551115123125782702E-14 ) ) ;
#14607 = DIRECTION ( 'NONE',  ( -5.551115123125774074E-17, -1.000000000000000000, -6.394689268473234689E-36 ) ) ;
#14608 = FACE_OUTER_BOUND ( 'NONE', #25934, .T. ) ;
#14609 = AXIS2_PLACEMENT_3D ( 'NONE', #9758, #11956, #2671 ) ;
#14610 = ORIENTED_EDGE ( 'NONE', *, *, #17486, .F. ) ;
#14611 = CARTESIAN_POINT ( 'NONE',  ( 119.9999999999997868, -5.999999999999873879, 1.056932319443148900E-13 ) ) ;
#14612 = CARTESIAN_POINT ( 'NONE',  ( 23.53867513459495342, 1.665334536937734811E-13, 2.499999999999835687 ) ) ;
#14613 = EDGE_CURVE ( 'NONE', #9799, #452, #10773, .T. ) ;
#14614 = ORIENTED_EDGE ( 'NONE', *, *, #28734, .T. ) ;
#14615 = CARTESIAN_POINT ( 'NONE',  ( 156.9449251345948539, -5.500000000000012434, 2.278174593052012309 ) ) ;
#14616 =( BOUNDED_CURVE ( )  B_SPLINE_CURVE ( 2, ( #29406, #8377, #22064, #29575, #29097, #10250, #6073, #17787, #26787 ),
 .UNSPECIFIED., .F., .F. ) 
 B_SPLINE_CURVE_WITH_KNOTS ( ( 3, 2, 2, 2, 3 ),
 ( 0.4194444444444444531, 0.4203703703703703942, 0.4222222222222222210, 0.4240740740740740478, 0.4249999999999999889 ),
 .UNSPECIFIED. ) 
 CURVE ( )  GEOMETRIC_REPRESENTATION_ITEM ( )  RATIONAL_B_SPLINE_CURVE ( ( 0.9330127018922194093, 0.9330127018922194093, 1.000000000000000000, 0.8660254037844388186, 1.000000000000000000, 0.8660254037844388186, 1.000000000000000000, 0.9330127018922194093, 0.9330127018922194093 ) ) 
 REPRESENTATION_ITEM ( '' )  );
#14617 = ADVANCED_FACE ( 'NONE', ( #2738 ), #28832, .T. ) ;
#14618 = ORIENTED_EDGE ( 'NONE', *, *, #16877, .T. ) ;
#14619 = ORIENTED_EDGE ( 'NONE', *, *, #26811, .F. ) ;
#14620 = DIRECTION ( 'NONE',  ( 1.000000000000000000, 0.000000000000000000, 0.000000000000000000 ) ) ;
#14621 = CARTESIAN_POINT ( 'NONE',  ( 161.7187500000000000, 2.485281374238555774, -6.000000000000005329 ) ) ;
#14622 =( BOUNDED_CURVE ( )  B_SPLINE_CURVE ( 2, ( #23814, #26399, #2753, #12324, #26548, #21668, #604, #9990, #19366 ),
 .UNSPECIFIED., .F., .F. ) 
 B_SPLINE_CURVE_WITH_KNOTS ( ( 3, 2, 2, 2, 3 ),
 ( 0.1093750000000000000, 0.1171875000000000000, 0.1250000000000000000, 0.1328125000000000000, 0.1406250000000000000 ),
 .UNSPECIFIED. ) 
 CURVE ( )  GEOMETRIC_REPRESENTATION_ITEM ( )  RATIONAL_B_SPLINE_CURVE ( ( 1.000000000000000000, 0.9238795325112867385, 1.000000000000000000, 0.9238795325112867385, 1.000000000000000000, 0.9238795325112867385, 1.000000000000000000, 0.9238795325112867385, 1.000000000000000000 ) ) 
 REPRESENTATION_ITEM ( '' )  );
#14623 = VERTEX_POINT ( 'NONE', #7213 ) ;
#14624 = CARTESIAN_POINT ( 'NONE',  ( -5.412658773652684552, -3.125000000000099920, -129.5669872981078470 ) ) ;
#14625 = DIRECTION ( 'NONE',  ( 1.000000000000000000, 1.734723475976843579E-16, 0.000000000000000000 ) ) ;
#14626 = CARTESIAN_POINT ( 'NONE',  ( 11.00000000000009237, -1.873492889144900975, -1.873492889145123019 ) ) ;
#14627 = CARTESIAN_POINT ( 'NONE',  ( 19.33632486540532014, -1.767766952966265404, -1.767766952966487448 ) ) ;
#14628 = EDGE_LOOP ( 'NONE', ( #8756, #28178, #14229, #19180 ) ) ;
#14629 = VECTOR ( 'NONE', #17473, 1000.000000000000000 ) ;
#14630 = CARTESIAN_POINT ( 'NONE',  ( 20.37500000000017053, -1.414213562372979016, 1.414213562373034527 ) ) ;
#14631 = LINE ( 'NONE', #16499, #3390 ) ;
#14632 = DIRECTION ( 'NONE',  ( 0.000000000000000000, -1.000000000000000000, -0.000000000000000000 ) ) ;
#14633 = CARTESIAN_POINT ( 'NONE',  ( 135.4538997308104058, -2.071067811865468400, -4.999999999999989342 ) ) ;
#14634 = CARTESIAN_POINT ( 'NONE',  ( -6.000000000000007105, -1.607695154586655129, -99.76933756729744118 ) ) ;
#14635 = CARTESIAN_POINT ( 'NONE',  ( -6.000000000000000888, 1.067854986875958443E-15, 7.560779664488942560E-35 ) ) ;
#14636 = DIRECTION ( 'NONE',  ( -1.000000000000000000, -1.665334536937731113E-16, 1.526556658859586792E-16 ) ) ;
#14637 = CARTESIAN_POINT ( 'NONE',  ( 161.0000000000000284, 0.000000000000000000, 0.000000000000000000 ) ) ;
#14638 = CARTESIAN_POINT ( 'NONE',  ( 6.000000000000000888, 1.743066579297358182E-13, -111.6636751345948255 ) ) ;
#14639 = CARTESIAN_POINT ( 'NONE',  ( 4.763139720814407951, 2.750000000000002665, -136.7500000000000284 ) ) ;
#14640 = CARTESIAN_POINT ( 'NONE',  ( 108.2113248654050892, -1.999999999999946265, 0.000000000000000000 ) ) ;
#14641 = VERTEX_POINT ( 'NONE', #2598 ) ;
#14642 = CARTESIAN_POINT ( 'NONE',  ( -2.775557561562891351E-14, -5.500000000000115463, -47.25000000000001421 ) ) ;
#14643 = CARTESIAN_POINT ( 'NONE',  ( 118.2886751345946976, 2.000000000000085265, 0.000000000000000000 ) ) ;
#14644 = VERTEX_POINT ( 'NONE', #21802 ) ;
#14645 = CARTESIAN_POINT ( 'NONE',  ( 118.3122167782374561, -0.7662911109076485650, -1.849990392679411677 ) ) ;
#14646 = CARTESIAN_POINT ( 'NONE',  ( 136.7812500000000568, 2.485281374238585972, 6.000000000000005329 ) ) ;
#14647 = CARTESIAN_POINT ( 'NONE',  ( 11.62499999999999645, -1.414213562373090038, -1.414213562373090038 ) ) ;
#14648 = CARTESIAN_POINT ( 'NONE',  ( 5.412658773652712085, -3.125000000000086153, -96.06698729810780435 ) ) ;
#14649 = EDGE_CURVE ( 'NONE', #2895, #8039, #11774, .T. ) ;
#14650 = PRESENTATION_STYLE_ASSIGNMENT (( #26722 ) ) ;
#14651 = EDGE_CURVE ( 'NONE', #29880, #22647, #15345, .T. ) ;
#14652 = CARTESIAN_POINT ( 'NONE',  ( 11.14882486540523843, -2.499999999999964473, 1.035533905932749299 ) ) ;
#14653 = CARTESIAN_POINT ( 'NONE',  ( 118.7499999999997868, -1.665334536937734811E-13, -2.500000000000057732 ) ) ;
#14654 = CARTESIAN_POINT ( 'NONE',  ( 3.464101615137852974, 5.999999999999884537, -77.83632486540520290 ) ) ;
#14655 = CARTESIAN_POINT ( 'NONE',  ( 6.350852961086080661, -9.614813431917819062E-14, -126.3749999999999858 ) ) ;
#14656 = VERTEX_POINT ( 'NONE', #7652 ) ;
#14657 = LINE ( 'NONE', #21712, #26784 ) ;
#14658 = CARTESIAN_POINT ( 'NONE',  ( 3.175426480543072749, -5.500000000000105693, -57.62500000000004974 ) ) ;
#14659 = CARTESIAN_POINT ( 'NONE',  ( 0.000000000000000000, -5.999999999999991118, -179.5386751345948255 ) ) ;
#14660 = CARTESIAN_POINT ( 'NONE',  ( 2.081668171172167281E-16, 3.582034040661430693E-16, -2.499999999999999112 ) ) ;
#14661 = CARTESIAN_POINT ( 'NONE',  ( 6.000000000000000888, 1.607695154586715303, -68.09668783648703538 ) ) ;
#14662 = CARTESIAN_POINT ( 'NONE',  ( 5.412658773652712085, -3.125000000000086153, -84.93301270189223828 ) ) ;
#14663 = CARTESIAN_POINT ( 'NONE',  ( 2.775557561562891351E-14, 20.00000000000001776, -31.00000000000002487 ) ) ;
#14664 = CARTESIAN_POINT ( 'NONE',  ( 6.000000000000000888, 1.743066579297358182E-13, -48.08632486540521711 ) ) ;
#14665 = LINE ( 'NONE', #17124, #22968 ) ;
#14666 = CARTESIAN_POINT ( 'NONE',  ( 116.0627832217622029, -0.7662911109076785410, -1.849990392679291551 ) ) ;
#14667 = CARTESIAN_POINT ( 'NONE',  ( -4.763139720814407951, 2.749999999999946709, -137.7500000000000284 ) ) ;
#14668 = CARTESIAN_POINT ( 'NONE',  ( -14.99999999999999289, -25.00000000000007816, -7.500000000000007105 ) ) ;
#14669 = CARTESIAN_POINT ( 'NONE',  ( 2.775557561562891351E-14, 6.250000000000033751, -154.9330127018922383 ) ) ;
#14670 = CARTESIAN_POINT ( 'NONE',  ( 116.0000000000000142, 0.000000000000000000, -5.500000000000000000 ) ) ;
#14671 = CARTESIAN_POINT ( 'NONE',  ( 146.7113248654052313, 5.500000000000005329, 0.000000000000000000 ) ) ;
#14672 = ADVANCED_FACE ( 'NONE', ( #17060 ), #5639, .T. ) ;
#14673 = CARTESIAN_POINT ( 'NONE',  ( -2.775557561562891351E-14, -5.500000000000115463, -69.75000000000002842 ) ) ;
#14674 = CARTESIAN_POINT ( 'NONE',  ( 0.000000000000000000, 5.499999999999991118, -66.00000000000000000 ) ) ;
#14675 = CARTESIAN_POINT ( 'NONE',  ( -4.000000000000000000, 7.119033245839722951E-16, -200.0000000000000000 ) ) ;
#14676 = CARTESIAN_POINT ( 'NONE',  ( 145.5148502691896510, -3.535533905932725318, -3.535533905932725318 ) ) ;
#14677 = CARTESIAN_POINT ( 'NONE',  ( 150.1875000000000284, 4.242640687119269671, 4.242640687119298093 ) ) ;
#14678 = FACE_BOUND ( 'NONE', #16746, .T. ) ;
#14679 = CARTESIAN_POINT ( 'NONE',  ( 17.87500000000008527, 1.414213562373312083, -1.414213562373145550 ) ) ;
#14680 = CARTESIAN_POINT ( 'NONE',  ( 3.464101615137757051, -5.999999999999979572, -98.41367513459481131 ) ) ;
#14681 = CARTESIAN_POINT ( 'NONE',  ( 0.000000000000000000, 5.999999999999977796, -82.21132486540521711 ) ) ;
#14682 = EDGE_CURVE ( 'NONE', #20580, #29780, #1578, .T. ) ;
#14683 = VERTEX_POINT ( 'NONE', #18270 ) ;
#14684 = CARTESIAN_POINT ( 'NONE',  ( 151.2187500000000284, 2.485281374238555774, -6.000000000000005329 ) ) ;
#14685 = UNCERTAINTY_MEASURE_WITH_UNIT (LENGTH_MEASURE( 1.000000000000000082E-05 ), #5563, 'distance_accuracy_value', 'NONE');
#14686 = CARTESIAN_POINT ( 'NONE',  ( 6.000000000000000888, 1.743066579297358182E-13, -64.58632486540520290 ) ) ;
#14687 = CARTESIAN_POINT ( 'NONE',  ( -4.763139720814407951, 2.749999999999946709, -178.2500000000000284 ) ) ;
#14688 = CARTESIAN_POINT ( 'NONE',  ( 21.62500000000017053, -1.414213562372979016, -1.414213562373090038 ) ) ;
#14689 = ORIENTED_EDGE ( 'NONE', *, *, #88, .T. ) ;
#14690 = CARTESIAN_POINT ( 'NONE',  ( 2.775557561562891351E-14, -6.250000000000061284, -154.8169872981078470 ) ) ;
#14691 = ORIENTED_EDGE ( 'NONE', *, *, #9815, .T. ) ;
#14692 = CARTESIAN_POINT ( 'NONE',  ( -3.175426480542816510, -5.500000000000057732, -84.87500000000004263 ) ) ;
#14693 = ORIENTED_EDGE ( 'NONE', *, *, #16069, .T. ) ;
#14694 = CARTESIAN_POINT ( 'NONE',  ( 119.9999999999998437, 0.8621349163126781345, 2.008502556958250640 ) ) ;
#14695 = FILL_AREA_STYLE ('',( #26335 ) ) ;
#14696 = FACE_OUTER_BOUND ( 'NONE', #4265, .T. ) ;
#14697 =( BOUNDED_CURVE ( )  B_SPLINE_CURVE ( 2, ( #3945, #14000, #25290, #23340, #13374, #4414, #22717, #18278, #17029 ),
 .UNSPECIFIED., .F., .T. ) 
 B_SPLINE_CURVE_WITH_KNOTS ( ( 3, 2, 2, 2, 3 ),
 ( 0.9138888888888888618, 0.9148148148148148584, 0.9166666666666666297, 0.9185185185185185119, 0.9194444444444443976 ),
 .UNSPECIFIED. ) 
 CURVE ( )  GEOMETRIC_REPRESENTATION_ITEM ( )  RATIONAL_B_SPLINE_CURVE ( ( 0.9330127018922194093, 0.9330127018922154125, 1.000000000000000000, 0.8660254037844388186, 1.000000000000000000, 0.8660254037844388186, 1.000000000000000000, 0.9330127018922234061, 0.9330127018922194093 ) ) 
 REPRESENTATION_ITEM ( '' )  );
#14698 = CARTESIAN_POINT ( 'NONE',  ( 3.175426480543072749, -5.500000000000105693, -161.1250000000000284 ) ) ;
#14699 = CARTESIAN_POINT ( 'NONE',  ( 160.9878691019586654, 3.688149050334593504, 4.090025542717429907 ) ) ;
#14700 = CARTESIAN_POINT ( 'NONE',  ( -3.175426480542816510, -5.500000000000057732, -147.8750000000000284 ) ) ;
#14701 = EDGE_CURVE ( 'NONE', #2318, #15772, #29288, .T. ) ;
#14702 = CYLINDRICAL_SURFACE ( 'NONE', #4645, 6.000000000000000888 ) ;
#14703 = DIRECTION ( 'NONE',  ( -1.000000000000000000, -1.665334536937736783E-16, -2.220446049250315546E-16 ) ) ;
#14704 = EDGE_CURVE ( 'NONE', #15998, #341, #2918, .T. ) ;
#14705 = VECTOR ( 'NONE', #8228, 1000.000000000000000 ) ;
#14706 = CARTESIAN_POINT ( 'NONE',  ( 6.350852961086080661, -9.614813431917819062E-14, -97.87499999999998579 ) ) ;
#14707 = FACE_OUTER_BOUND ( 'NONE', #22114, .T. ) ;
#14708 = CARTESIAN_POINT ( 'NONE',  ( -4.763139720814407951, -2.750000000000016431, -92.50000000000002842 ) ) ;
#14709 = AXIS2_PLACEMENT_3D ( 'NONE', #15070, #22127, #2768 ) ;
#14710 = DIRECTION ( 'NONE',  ( 1.000000000000000000, 0.000000000000000000, 0.000000000000000000 ) ) ;
#14711 = CARTESIAN_POINT ( 'NONE',  ( 157.8898502691896510, 3.535533905932725318, -3.535533905932725318 ) ) ;
#14712 = CARTESIAN_POINT ( 'NONE',  ( -3.464101615137725076, 5.999999999999979572, -64.66367513459478289 ) ) ;
#14713 = DIRECTION ( 'NONE',  ( 1.000000000000000000, -5.551115123125773458E-17, -1.260129944081490338E-35 ) ) ;
#14714 = CARTESIAN_POINT ( 'NONE',  ( 22.75000000000015987, 1.110223024625156540E-13, -2.000000000000168310 ) ) ;
#14715 = CARTESIAN_POINT ( 'NONE',  ( 109.5624999999997158, -2.499999999999994671, -1.035533905932508825 ) ) ;
#14716 = CARTESIAN_POINT ( 'NONE',  ( 145.4136751345948539, 0.000000000000000000, -5.500000000000005329 ) ) ;
#14717 = ADVANCED_FACE ( 'NONE', ( #10903 ), #4395, .T. ) ;
#14718 = CARTESIAN_POINT ( 'NONE',  ( 0.7669223171414829565, -14.69693845669908860, -7.500000000000007105 ) ) ;
#14719 = EDGE_CURVE ( 'NONE', #4838, #9581, #21589, .T. ) ;
#14720 = ORIENTED_EDGE ( 'NONE', *, *, #23147, .F. ) ;
#14721 = CARTESIAN_POINT ( 'NONE',  ( 5.999999999999993783, 1.607695154586726627, -179.0966878364870638 ) ) ;
#14722 = CARTESIAN_POINT ( 'NONE',  ( -6.000000000000000888, 1.067854986875958443E-15, 7.560779664488942560E-35 ) ) ;
#14723 = CARTESIAN_POINT ( 'NONE',  ( 104.1247167782375556, -1.849990392679468076, 0.000000000000000000 ) ) ;
#14724 = EDGE_LOOP ( 'NONE', ( #8457, #15960, #30272, #28909, #20595 ) ) ;
#14725 = CARTESIAN_POINT ( 'NONE',  ( -3.175426480542816510, 5.499999999999865885, -103.3750000000000142 ) ) ;
#14726 = CARTESIAN_POINT ( 'NONE',  ( 17.43750000000003908, 2.649519052838358757, 1.097466725451379244 ) ) ;
#14727 = CARTESIAN_POINT ( 'NONE',  ( 7.216878364870455975, -6.409875621278545621E-14, -122.3080127018922099 ) ) ;
#14728 = ORIENTED_EDGE ( 'NONE', *, *, #14576, .F. ) ;
#14729 = CARTESIAN_POINT ( 'NONE',  ( 6.000000000000000888, -1.859271017917181981E-14, -110.1636751345948397 ) ) ;
#14730 = MECHANICAL_DESIGN_GEOMETRIC_PRESENTATION_REPRESENTATION (  '', ( #1477 ), #13287 ) ;
#14731 = CARTESIAN_POINT ( 'NONE',  ( -7.216878364870328078, 0.000000000000000000, -162.6919872981078754 ) ) ;
#14732 = DIRECTION ( 'NONE',  ( 0.000000000000000000, 0.000000000000000000, 1.000000000000000000 ) ) ;
#14733 = CARTESIAN_POINT ( 'NONE',  ( 131.7976497308104058, 0.000000000000000000, 5.000000000000004441 ) ) ;
#14734 = CARTESIAN_POINT ( 'NONE',  ( -3.608439182435052128, -6.250000000000110134, -59.80801270189223118 ) ) ;
#14735 = ORIENTED_EDGE ( 'NONE', *, *, #15046, .T. ) ;
#14736 = CARTESIAN_POINT ( 'NONE',  ( 0.8346751507289797978, -15.41336419498994026, -8.287310550375268647 ) ) ;
#14737 = DIRECTION ( 'NONE',  ( 1.000000000000000000, -0.000000000000000000, -0.000000000000000000 ) ) ;
#14738 = CARTESIAN_POINT ( 'NONE',  ( -5.999999999999962697, 3.323446944526963260E-14, -150.8363248654052029 ) ) ;
#14739 = CARTESIAN_POINT ( 'NONE',  ( 119.3749999999998863, -1.767766952966209892, 1.767766952966542959 ) ) ;
#14740 = CARTESIAN_POINT ( 'NONE',  ( -4.999999999999886313, -10.50000000000000888, 8.000000000000007105 ) ) ;
#14742 = MANIFOLD_SOLID_BREP ( 'Cut-Sweep2', #17882 ) ;
#14741 = CARTESIAN_POINT ( 'NONE',  ( -3.608439182435115633, 6.249999999999965361, -168.3080127018922383 ) ) ;
#14743 = CARTESIAN_POINT ( 'NONE',  ( 113.6011751345946124, -0.8284271247461753029, 2.000000000000271783 ) ) ;
#14744 = EDGE_CURVE ( 'NONE', #19344, #11694, #21600, .T. ) ;
#14745 = FACE_OUTER_BOUND ( 'NONE', #6878, .T. ) ;
#14746 = DIRECTION ( 'NONE',  ( 0.000000000000000000, 1.000000000000000000, -0.000000000000000000 ) ) ;
#14747 = CARTESIAN_POINT ( 'NONE',  ( -4.763139720814407951, 2.749999999999946709, -115.2500000000000142 ) ) ;
#14748 = DIRECTION ( 'NONE',  ( 0.000000000000000000, 0.000000000000000000, -1.000000000000000000 ) ) ;
#14749 = CARTESIAN_POINT ( 'NONE',  ( -6.000000000000000888, 1.067854986875958443E-15, 7.560779664488942560E-35 ) ) ;
#14750 = VERTEX_POINT ( 'NONE', #24341 ) ;
#14751 = CARTESIAN_POINT ( 'NONE',  ( 18.50000000000004263, 1.873492889145123019, -1.873492889144956486 ) ) ;
#14752 = CYLINDRICAL_SURFACE ( 'NONE', #27039, 6.000000000000001776 ) ;
#14753 = AXIS2_PLACEMENT_3D ( 'NONE', #14767, #12331, #14625 ) ;
#14754 = CARTESIAN_POINT ( 'NONE',  ( -6.000000000000007105, -1.607695154586655129, -56.26933756729747671 ) ) ;
#14755 = EDGE_CURVE ( 'NONE', #12840, #10564, #13201, .T. ) ;
#14756 = COLOUR_RGB ( '', 0.09019608, 0.27058824, 0.51372549) ;
#14757 = ORIENTED_EDGE ( 'NONE', *, *, #9919, .F. ) ;
#14758 = CARTESIAN_POINT ( 'NONE',  ( 0.000000000000000000, 0.000000000000000000, -16.50000000000000355 ) ) ;
#14759 = CARTESIAN_POINT ( 'NONE',  ( 17.41367513459490723, 1.767766952966542959, 1.767766952966320915 ) ) ;
#14760 =( LENGTH_UNIT ( ) NAMED_UNIT ( * ) SI_UNIT ( .MILLI., .METRE. ) );
#14761 = ORIENTED_EDGE ( 'NONE', *, *, #1691, .T. ) ;
#14762 = CARTESIAN_POINT ( 'NONE',  ( 157.2261751345948539, -3.889087296526011706, -3.889087296526011706 ) ) ;
#14763 = ORIENTED_EDGE ( 'NONE', *, *, #18299, .T. ) ;
#14764 = FACE_OUTER_BOUND ( 'NONE', #20567, .T. ) ;
#14765 = CARTESIAN_POINT ( 'NONE',  ( 160.2187500000000000, 2.485281374238555774, -6.000000000000005329 ) ) ;
#14766 = CARTESIAN_POINT ( 'NONE',  ( -5.412658773652739619, 3.124999999999975131, -134.3169872981078186 ) ) ;
#14767 = CARTESIAN_POINT ( 'NONE',  ( 0.000000000000000000, 10.00000000000000888, 4.000000000000003553 ) ) ;
#14768 = CARTESIAN_POINT ( 'NONE',  ( -5.999999999999944933, 1.607695154586759934, -130.4806624327025872 ) ) ;
#14769 = CARTESIAN_POINT ( 'NONE',  ( 5.196152422706629359, -2.999999999999988898, -116.2886751345948397 ) ) ;
#14770 = STYLED_ITEM ( 'NONE', ( #13392 ), #27710 ) ;
#14771 = ORIENTED_EDGE ( 'NONE', *, *, #2050, .F. ) ;
#14772 = CARTESIAN_POINT ( 'NONE',  ( 17.31250000000004263, -0.8284271247461152399, 2.000000000000091926 ) ) ;
#14773 = CARTESIAN_POINT ( 'NONE',  ( -0.04610858258174108104, -15.28214019190275330, -7.207076054451203362 ) ) ;
#14774 = CARTESIAN_POINT ( 'NONE',  ( 0.000000000000000000, -15.50000000000001421, 5.656854249492387687 ) ) ;
#14775 = VECTOR ( 'NONE', #23075, 1000.000000000000000 ) ;
#14776 = CARTESIAN_POINT ( 'NONE',  ( 136.5788997308104058, -4.999999999999989342, 2.071067811865468400 ) ) ;
#14777 = CARTESIAN_POINT ( 'NONE',  ( 101.5358983848621932, 0.000000000000000000, 0.000000000000000000 ) ) ;
#14778 = STYLED_ITEM ( 'NONE', ( #17056 ), #328 ) ;
#14779 = CARTESIAN_POINT ( 'NONE',  ( 3.464101615137757051, -5.999999999999979572, -69.33632486540518869 ) ) ;
#14780 = CARTESIAN_POINT ( 'NONE',  ( 104.7499999999998295, 5.551115123125782702E-14, -2.499999999999835687 ) ) ;
#14781 = EDGE_CURVE ( 'NONE', #28335, #14937, #6060, .T. ) ;
#14782 = CARTESIAN_POINT ( 'NONE',  ( -5.999999999999982236, -1.607695154586700426, -115.3466878364870638 ) ) ;
#14783 = CARTESIAN_POINT ( 'NONE',  ( 3.175426480543072749, 5.499999999999865885, -135.1250000000000000 ) ) ;
#14784 = VECTOR ( 'NONE', #23696, 1000.000000000000000 ) ;
#14785 = SURFACE_STYLE_FILL_AREA ( #19824 ) ;
#14786 = ORIENTED_EDGE ( 'NONE', *, *, #565, .F. ) ;
#14787 = CARTESIAN_POINT ( 'NONE',  ( 108.0386751345947687, 5.551115123125782702E-14, -2.000000000000001776 ) ) ;
#14788 = EDGE_CURVE ( 'NONE', #28360, #23232, #5866, .T. ) ;
#14789 = CARTESIAN_POINT ( 'NONE',  ( 117.9761751345946408, -0.8284271247461453269, -1.999999999999851674 ) ) ;
#14790 =( BOUNDED_CURVE ( )  B_SPLINE_CURVE ( 2, ( #22827, #11019, #25249, #6687, #3907, #2088, #1926, #18234, #4222 ),
 .UNSPECIFIED., .F., .F. ) 
 B_SPLINE_CURVE_WITH_KNOTS ( ( 3, 2, 2, 2, 3 ),
 ( 0.06388888888888888395, 0.06481481481481476958, 0.06666666666666665186, 0.06851851851851853414, 0.06944444444444441977 ),
 .UNSPECIFIED. ) 
 CURVE ( )  GEOMETRIC_REPRESENTATION_ITEM ( )  RATIONAL_B_SPLINE_CURVE ( ( 0.9330127018922194093, 0.9330127018922194093, 1.000000000000000000, 0.8660254037844388186, 1.000000000000000000, 0.8660254037844388186, 1.000000000000000000, 0.9330127018922234061, 0.9330127018922194093 ) ) 
 REPRESENTATION_ITEM ( '' )  );
#14791 = ORIENTED_EDGE ( 'NONE', *, *, #20411, .T. ) ;
#14792 = CARTESIAN_POINT ( 'NONE',  ( 116.1247167782375556, -1.849990392679468076, 1.110223024625156540E-13 ) ) ;
#14793 = CARTESIAN_POINT ( 'NONE',  ( -4.999999999999990230, -55.00000000000002132, -4.000000000000003553 ) ) ;
#14794 = APPLICATION_CONTEXT ( 'automotive_design' ) ;
#14795 = CARTESIAN_POINT ( 'NONE',  ( -5.412658773652684552, -3.125000000000099920, -92.06698729810780435 ) ) ;
#14796 = PRESENTATION_LAYER_ASSIGNMENT (  '', '', ( #9878 ) ) ;
#14797 =( NAMED_UNIT ( * ) SI_UNIT ( $, .STERADIAN. ) SOLID_ANGLE_UNIT ( ) );
#14798 =( BOUNDED_CURVE ( )  B_SPLINE_CURVE ( 2, ( #27343, #6002, #11101, #27191, #15255, #22301, #22459, #29342, #15579 ),
 .UNSPECIFIED., .F., .T. ) 
 B_SPLINE_CURVE_WITH_KNOTS ( ( 3, 2, 2, 2, 3 ),
 ( 0.05833333333333332732, 0.05925925925925926152, 0.06111111111111110911, 0.06296296296296295669, 0.06388888888888888395 ),
 .UNSPECIFIED. ) 
 CURVE ( )  GEOMETRIC_REPRESENTATION_ITEM ( )  RATIONAL_B_SPLINE_CURVE ( ( 0.9330127018922194093, 0.9330127018922189652, 1.000000000000000000, 0.8660254037844388186, 1.000000000000000000, 0.8660254037844388186, 1.000000000000000000, 0.9330127018922194093, 0.9330127018922194093 ) ) 
 REPRESENTATION_ITEM ( '' )  );
#14799 = CARTESIAN_POINT ( 'NONE',  ( 140.5000000000000284, 0.000000000000000000, 0.000000000000000000 ) ) ;
#14800 = CARTESIAN_POINT ( 'NONE',  ( 118.6874999999998295, -1.035533905932719101, -2.499999999999844569 ) ) ;
#14801 = CARTESIAN_POINT ( 'NONE',  ( -4.763139720814407951, 2.749999999999946709, -133.2500000000000284 ) ) ;
#14802 = VERTEX_POINT ( 'NONE', #1763 ) ;
#14803 = PRESENTATION_LAYER_ASSIGNMENT (  '', '', ( #28011 ) ) ;
#14804 = ORIENTED_EDGE ( 'NONE', *, *, #2081, .T. ) ;
#14805 = CARTESIAN_POINT ( 'NONE',  ( -3.464101615137757051, -5.999999999999979572, -83.08632486540517448 ) ) ;
#14806 = CARTESIAN_POINT ( 'NONE',  ( 0.000000000000000000, 5.499999999999991118, -55.49999999999999289 ) ) ;
#14807 = CARTESIAN_POINT ( 'NONE',  ( 0.000000000000000000, -5.999999999999991118, -62.53867513459482552 ) ) ;
#14808 =( LENGTH_UNIT ( ) NAMED_UNIT ( * ) SI_UNIT ( .MILLI., .METRE. ) );
#14809 = CARTESIAN_POINT ( 'NONE',  ( -3.608439182435052128, -6.250000000000110134, -76.30801270189225249 ) ) ;
#14810 = CARTESIAN_POINT ( 'NONE',  ( 0.000000000000000000, 0.000000000000000000, -183.0000000000000000 ) ) ;
#14811 = LINE ( 'NONE', #12230, #27998 ) ;
#14812 = CARTESIAN_POINT ( 'NONE',  ( 0.000000000000000000, -5.999999999999991118, -168.4613248654052029 ) ) ;
#14813 = SURFACE_STYLE_USAGE ( .BOTH. , #28748 ) ;
#14814 = VECTOR ( 'NONE', #21689, 1000.000000000000000 ) ;
#14815 = EDGE_CURVE ( 'NONE', #29310, #27213, #29244, .T. ) ;
#14816 = DIRECTION ( 'NONE',  ( -7.147005652999508048E-36, 5.642372883946980038E-36, 1.000000000000000000 ) ) ;
#14817 = CARTESIAN_POINT ( 'NONE',  ( 116.6252832217622313, 0.000000000000000000, 1.849990392679523588 ) ) ;
#14818 = EDGE_CURVE ( 'NONE', #30239, #12335, #28030, .T. ) ;
#14819 = CARTESIAN_POINT ( 'NONE',  ( -3.175426480542816066, -5.500000000000057732, -141.8750000000000568 ) ) ;
#14820 = CARTESIAN_POINT ( 'NONE',  ( 139.8009670889181564, -8.830838033386935848, 8.125417887732853117 ) ) ;
#14821 = CARTESIAN_POINT ( 'NONE',  ( 139.7886751345948539, 5.500000000000005329, 0.000000000000000000 ) ) ;
#14822 = SURFACE_SIDE_STYLE ('',( #21728 ) ) ;
#14823 = CARTESIAN_POINT ( 'NONE',  ( -4.763139720814407951, 2.749999999999946709, -67.25000000000002842 ) ) ;
#14824 = CARTESIAN_POINT ( 'NONE',  ( -2.775557561562891351E-14, -5.500000000000115463, -60.75000000000002842 ) ) ;
#14825 = CARTESIAN_POINT ( 'NONE',  ( -10.00000000000000178, -19.99999999999998934, -4.000000000000003553 ) ) ;
#14826 = VERTEX_POINT ( 'NONE', #1301 ) ;
#14827 = CARTESIAN_POINT ( 'NONE',  ( 146.7336002691897079, -4.999999999999989342, 2.071067811865468400 ) ) ;
#14828 = PRESENTATION_LAYER_ASSIGNMENT (  '', '', ( #28035 ) ) ;
#14829 = CARTESIAN_POINT ( 'NONE',  ( 151.9687500000000284, -2.485281374238585972, 6.000000000000005329 ) ) ;
#14830 = FACE_OUTER_BOUND ( 'NONE', #24248, .T. ) ;
#14831 = CARTESIAN_POINT ( 'NONE',  ( 0.000000000000000000, 0.000000000000000000, 0.000000000000000000 ) ) ;
#14832 = ORIENTED_EDGE ( 'NONE', *, *, #24184, .T. ) ;
#14833 = CARTESIAN_POINT ( 'NONE',  ( 142.4062500000000568, 6.000000000000005329, -2.485281374238555774 ) ) ;
#14834 = CIRCLE ( 'NONE', #20228, 0.4999999999999993894 ) ;
#14835 = CARTESIAN_POINT ( 'NONE',  ( 104.8954487758440877, 0.3872062312935020123, 1.908582334821284254 ) ) ;
#14836 = CARTESIAN_POINT ( 'NONE',  ( -6.350852961085760029, -1.281975124255709124E-13, -178.1250000000000568 ) ) ;
#14837 = CARTESIAN_POINT ( 'NONE',  ( 15.75000000000006928, 2.775557561562891351E-13, -2.000000000000057288 ) ) ;
#14838 = CARTESIAN_POINT ( 'NONE',  ( 5.412658773652712085, -3.125000000000086153, -156.0669872981078754 ) ) ;
#14839 = ORIENTED_EDGE ( 'NONE', *, *, #19363, .T. ) ;
#14840 = CARTESIAN_POINT ( 'NONE',  ( 6.350852961086080661, -9.614813431917819062E-14, -78.37500000000001421 ) ) ;
#14841 = CARTESIAN_POINT ( 'NONE',  ( 2.775557561562891351E-14, -6.250000000000061284, -103.1830127018922241 ) ) ;
#14842 = ORIENTED_EDGE ( 'NONE', *, *, #14781, .T. ) ;
#14843 = CARTESIAN_POINT ( 'NONE',  ( -5.999999999999964473, 1.607695154586726405, -175.4806624327026441 ) ) ;
#14844 = CIRCLE ( 'NONE', #9449, 1.000000000000000888 ) ;
#14845 = CARTESIAN_POINT ( 'NONE',  ( -38.99999999999998579, -59.99999999999980105, 4.000000000000003553 ) ) ;
#14846 = CARTESIAN_POINT ( 'NONE',  ( 5.608370619328757023, -9.463293048187454204, -22.85879529262368237 ) ) ;
#14847 = EDGE_CURVE ( 'NONE', #12257, #691, #16347, .T. ) ;
#14848 = CARTESIAN_POINT ( 'NONE',  ( 4.763139720814407951, 2.750000000000002665, -166.7500000000000000 ) ) ;
#14849 = CARTESIAN_POINT ( 'NONE',  ( 143.8050748654052313, 5.500000000000012434, 2.278174593052012309 ) ) ;
#14850 = CARTESIAN_POINT ( 'NONE',  ( 0.000000000000000000, 5.499999999999991118, -147.0000000000000284 ) ) ;
#14851 = LINE ( 'NONE', #24195, #5122 ) ;
#14852 = B_SPLINE_CURVE_WITH_KNOTS ( 'NONE', 3,
 ( #6769, #18473, #4312, #18327, #22762, #20307, #8620, #27944 ),
 .UNSPECIFIED., .F., .F.,
 ( 4, 2, 2, 4 ),
 ( 0.000000000000000000, 0.0006652843935019894924, 0.0009979265902529841845, 0.001330568787003978985 ),
 .UNSPECIFIED. ) ;
#14853 = CARTESIAN_POINT ( 'NONE',  ( -6.350852961085760029, -1.281975124255709124E-13, -95.62500000000004263 ) ) ;
#14854 = CARTESIAN_POINT ( 'NONE',  ( -2.775557561562891351E-14, -5.500000000000115463, -80.25000000000004263 ) ) ;
#14855 = CARTESIAN_POINT ( 'NONE',  ( -5.999999999999963585, 1.780251999655701777E-13, -72.83632486540523132 ) ) ;
#14856 = CARTESIAN_POINT ( 'NONE',  ( 6.000000000000000888, 1.607695154586715303, -144.0193375672974696 ) ) ;
#14857 = CARTESIAN_POINT ( 'NONE',  ( 23.31250000000007461, -0.8284271247460552878, 2.000000000000091926 ) ) ;
#14858 = CARTESIAN_POINT ( 'NONE',  ( -5.999999999999963585, 8.134310703387671600E-14, -125.9136751345948397 ) ) ;
#14859 = PRESENTATION_STYLE_ASSIGNMENT (( #12574 ) ) ;
#14860 = CARTESIAN_POINT ( 'NONE',  ( 20.10117513459495342, 1.035533905932869425, -2.499999999999964473 ) ) ;
#14861 = EDGE_LOOP ( 'NONE', ( #10882, #29101, #10880, #18779 ) ) ;
#14862 = CARTESIAN_POINT ( 'NONE',  ( 161.0625000000000284, -4.242640687119298093, 4.242640687119298093 ) ) ;
#14863 = CARTESIAN_POINT ( 'NONE',  ( 116.0000000000000142, 0.000000000000000000, -5.500000000000000000 ) ) ;
#14864 = CARTESIAN_POINT ( 'NONE',  ( 3.464101615137852974, 5.999999999999884537, -80.83632486540523132 ) ) ;
#14865 = CARTESIAN_POINT ( 'NONE',  ( 120.6252832217622881, 2.775557561562891351E-14, 1.849990392679523588 ) ) ;
#14866 = VERTEX_POINT ( 'NONE', #27103 ) ;
#14867 = ORIENTED_EDGE ( 'NONE', *, *, #15356, .F. ) ;
#14868 = ADVANCED_FACE ( 'NONE', ( #5903 ), #3440, .T. ) ;
#14869 = CARTESIAN_POINT ( 'NONE',  ( 6.350852961086080661, -9.614813431917819062E-14, -106.8750000000000142 ) ) ;
#14870 = CARTESIAN_POINT ( 'NONE',  ( 19.31250000000007105, 2.649519052838419153, -1.097466725451559322 ) ) ;
#14871 =( BOUNDED_CURVE ( )  B_SPLINE_CURVE ( 2, ( #24335, #28789, #12715, #21615, #249, #546, #7602, #9632, #19026 ),
 .UNSPECIFIED., .F., .T. ) 
 B_SPLINE_CURVE_WITH_KNOTS ( ( 3, 2, 2, 2, 3 ),
 ( 0.4249999999999999334, 0.4259259259259259300, 0.4277777777777778123, 0.4296296296296295836, 0.4305555555555555802 ),
 .UNSPECIFIED. ) 
 CURVE ( )  GEOMETRIC_REPRESENTATION_ITEM ( )  RATIONAL_B_SPLINE_CURVE ( ( 0.9330127018922194093, 0.9330127018922154125, 1.000000000000000000, 0.8660254037844388186, 1.000000000000000000, 0.8660254037844388186, 1.000000000000000000, 0.9330127018922154125, 0.9330127018922194093 ) ) 
 REPRESENTATION_ITEM ( '' )  );
#14872 = CARTESIAN_POINT ( 'NONE',  ( 5.412658773652739619, 3.124999999999988898, -125.1830127018922525 ) ) ;
#14873 =( GEOMETRIC_REPRESENTATION_CONTEXT ( 3 ) GLOBAL_UNCERTAINTY_ASSIGNED_CONTEXT ( ( #28353 ) ) GLOBAL_UNIT_ASSIGNED_CONTEXT ( ( #21236, #5071, #26418 ) ) REPRESENTATION_CONTEXT ( 'NONE', 'WORKASPACE' ) );
#14874 = VERTEX_POINT ( 'NONE', #22212 ) ;
#14875 = CARTESIAN_POINT ( 'NONE',  ( 0.000000000000000000, -5.999999999999991118, -61.03867513459482552 ) ) ;
#14876 = CARTESIAN_POINT ( 'NONE',  ( -3.608439182435052128, -6.250000000000110134, -162.4419872981077901 ) ) ;
#14877 = DIRECTION ( 'NONE',  ( 1.000000000000000000, 0.000000000000000000, 0.000000000000000000 ) ) ;
#14878 = CARTESIAN_POINT ( 'NONE',  ( -3.464101615137725076, 5.999999999999979572, -63.16367513459483973 ) ) ;
#14879 = CARTESIAN_POINT ( 'NONE',  ( 3.608439182435180470, 6.249999999999982236, -63.55801270189224539 ) ) ;
#14880 = ORIENTED_EDGE ( 'NONE', *, *, #4768, .T. ) ;
#14881 = CARTESIAN_POINT ( 'NONE',  ( 0.000000000000000000, 0.000000000000000000, 0.000000000000000000 ) ) ;
#14882 = EDGE_CURVE ( 'NONE', #4876, #15344, #18479, .T. ) ;
#14883 = CARTESIAN_POINT ( 'NONE',  ( 2.799076333356274106E-14, 11.00000000000000000, -19.00000000000002132 ) ) ;
#14884 = CARTESIAN_POINT ( 'NONE',  ( 4.763139720814407951, 2.750000000000002665, -168.2500000000000000 ) ) ;
#14885 = CARTESIAN_POINT ( 'NONE',  ( 105.1252832217623023, -5.551115123125782702E-14, -1.849990392679523588 ) ) ;
#14886 = CARTESIAN_POINT ( 'NONE',  ( 136.0000000000000284, 0.000000000000000000, 0.000000000000000000 ) ) ;
#14887 = CARTESIAN_POINT ( 'NONE',  ( -5.412658773652739619, 3.124999999999975131, -171.1830127018922383 ) ) ;
#14888 = FACE_OUTER_BOUND ( 'NONE', #13725, .T. ) ;
#14889 = CARTESIAN_POINT ( 'NONE',  ( 24.62500000000012079, -1.414213562372923505, -1.414213562373145550 ) ) ;
#14890 = CARTESIAN_POINT ( 'NONE',  ( -4.763139720814407951, 2.749999999999946709, -118.2500000000000284 ) ) ;
#14891 = CARTESIAN_POINT ( 'NONE',  ( 4.763139720814407951, -2.749999999999988454, -114.5000000000000426 ) ) ;
#14892 = PRESENTATION_STYLE_ASSIGNMENT (( #19785 ) ) ;
#14893 = DIRECTION ( 'NONE',  ( -7.147005652999508048E-36, 5.642372883946980038E-36, 1.000000000000000000 ) ) ;
#14894 = ORIENTED_EDGE ( 'NONE', *, *, #11622, .T. ) ;
#14895 = CARTESIAN_POINT ( 'NONE',  ( 19.25000000000009948, -1.873492889144845464, -1.873492889145011997 ) ) ;
#14896 = CARTESIAN_POINT ( 'NONE',  ( 120.4374999999997442, -2.499999999999964473, 1.035533905932989551 ) ) ;
#14897 = CARTESIAN_POINT ( 'NONE',  ( -5.999999999999962697, 3.323446944526963891E-14, -162.8363248654052313 ) ) ;
#14898 = AXIS2_PLACEMENT_3D ( 'NONE', #12133, #24202, #556 ) ;
#14899 = ORIENTED_EDGE ( 'NONE', *, *, #21946, .F. ) ;
#14900 = CARTESIAN_POINT ( 'NONE',  ( -5.196152422706573404, -3.000000000000002665, -127.2886751345948539 ) ) ;
#14901 = AXIS2_PLACEMENT_3D ( 'NONE', #19861, #29678, #20017 ) ;
#14902 = CARTESIAN_POINT ( 'NONE',  ( 5.412658773652712085, -3.125000000000086153, -82.56698729810784698 ) ) ;
#14903 = CARTESIAN_POINT ( 'NONE',  ( 5.196152422706629359, 3.000000000000002665, -110.0386751345948682 ) ) ;
#14904 = ORIENTED_EDGE ( 'NONE', *, *, #15605, .T. ) ;
#14905 = CARTESIAN_POINT ( 'NONE',  ( 6.000000000000000888, 7.762456499804235646E-14, -138.6636751345948255 ) ) ;
#14906 = PRODUCT_DEFINITION_FORMATION_WITH_SPECIFIED_SOURCE ( 'ANY', '', #6474, .NOT_KNOWN. ) ;
#14907 = VERTEX_POINT ( 'NONE', #22672 ) ;
#14908 = ORIENTED_EDGE ( 'NONE', *, *, #27420, .F. ) ;
#14909 = CARTESIAN_POINT ( 'NONE',  ( 159.6562500000000568, -6.000000000000005329, 2.485281374238555774 ) ) ;
#14910 = EDGE_CURVE ( 'NONE', #9387, #4270, #24028, .T. ) ;
#14911 = ORIENTED_EDGE ( 'NONE', *, *, #8067, .T. ) ;
#14912 = CARTESIAN_POINT ( 'NONE',  ( 2.775557561562891351E-14, -6.250000000000061284, -129.3169872981078186 ) ) ;
#14913 = CARTESIAN_POINT ( 'NONE',  ( -6.000000000000060396, -1.607695154586566089, -135.7693375672974412 ) ) ;
#14914 = CARTESIAN_POINT ( 'NONE',  ( 0.000000000000000000, 0.000000000000000000, 0.000000000000000000 ) ) ;
#14915 = CARTESIAN_POINT ( 'NONE',  ( 19.21132486540538764, -2.499999999999835687, -1.110223024625156540E-13 ) ) ;
#14916 = ORIENTED_EDGE ( 'NONE', *, *, #18744, .F. ) ;
#14917 = CARTESIAN_POINT ( 'NONE',  ( 14.50000000000012434, -1.999999999999779732, -5.551115123125782702E-14 ) ) ;
#14918 = DIRECTION ( 'NONE',  ( -6.938893903907221278E-15, 1.000000000000000000, 0.000000000000000000 ) ) ;
#14919 = EDGE_CURVE ( 'NONE', #28771, #29814, #1940, .T. ) ;
#14920 = CARTESIAN_POINT ( 'NONE',  ( 0.000000000000000000, -5.999999999999991118, -91.96132486540520290 ) ) ;
#14921 = CARTESIAN_POINT ( 'NONE',  ( -5.196152422706601826, 2.999999999999975131, -56.46132486540522422 ) ) ;
#14922 = CARTESIAN_POINT ( 'NONE',  ( 140.7976497308104058, 0.000000000000000000, 5.000000000000004441 ) ) ;
#14923 = CARTESIAN_POINT ( 'NONE',  ( 5.196152422706629359, -2.999999999999988898, -99.21132486540523132 ) ) ;
#14924 = CARTESIAN_POINT ( 'NONE',  ( 6.000000000000000888, -1.859271017917181981E-14, -46.58632486540520290 ) ) ;
#14925 = AXIS2_PLACEMENT_3D ( 'NONE', #16365, #4181, #11753 ) ;
#14926 = SURFACE_SIDE_STYLE ('',( #24419 ) ) ;
#14927 = DIRECTION ( 'NONE',  ( 1.000000000000000000, -5.551115123125773458E-17, -1.260129944081490338E-35 ) ) ;
#14928 = CARTESIAN_POINT ( 'NONE',  ( 107.7499999999998579, 5.551115123125782702E-14, -2.499999999999946709 ) ) ;
#14929 = CARTESIAN_POINT ( 'NONE',  ( -5.999999999999963585, -2.788906526875773208E-15, -176.9136751345948539 ) ) ;
#14930 = CARTESIAN_POINT ( 'NONE',  ( 6.350852961086080661, -9.614813431917819062E-14, -136.8750000000000568 ) ) ;
#14931 = VERTEX_POINT ( 'NONE', #25406 ) ;
#14932 = CARTESIAN_POINT ( 'NONE',  ( 13.21132486540532724, -2.499999999999891198, -1.110223024625156540E-13 ) ) ;
#14933 = CARTESIAN_POINT ( 'NONE',  ( 6.350852961086080661, -9.614813431917819062E-14, -46.87500000000000000 ) ) ;
#14934 = DIRECTION ( 'NONE',  ( 0.000000000000000000, 0.000000000000000000, 1.000000000000000000 ) ) ;
#14935 = CARTESIAN_POINT ( 'NONE',  ( 112.6636751345946976, -1.414213562373062283, 1.414213562373034527 ) ) ;
#14936 = CARTESIAN_POINT ( 'NONE',  ( -5.999999999999956479, -1.607695154586745057, -164.2693375672974412 ) ) ;
#14937 = VERTEX_POINT ( 'NONE', #11327 ) ;
#14938 = CARTESIAN_POINT ( 'NONE',  ( 118.1872167782374845, -1.849990392679472073, -0.7662911109076485650 ) ) ;
#14939 = CARTESIAN_POINT ( 'NONE',  ( 136.5937500000000853, 6.000000000000005329, 2.485281374238585972 ) ) ;
#14940 = CARTESIAN_POINT ( 'NONE',  ( 10.81250000000001243, 0.8284271247461753029, -2.000000000000091926 ) ) ;
#14941 = CARTESIAN_POINT ( 'NONE',  ( -3.608439182435115633, 6.249999999999965361, -96.94198729810781856 ) ) ;
#14942 = CARTESIAN_POINT ( 'NONE',  ( -39.00000000000000000, -20.00000000000001776, -4.000000000000003553 ) ) ;
#14943 = CARTESIAN_POINT ( 'NONE',  ( 112.6249999999998437, -1.767766952966431937, -1.767766952966320915 ) ) ;
#14944 = DIRECTION ( 'NONE',  ( 0.000000000000000000, -1.000000000000000000, -0.000000000000000000 ) ) ;
#14945 = CARTESIAN_POINT ( 'NONE',  ( 0.000000000000000000, 0.000000000000000000, 0.000000000000000000 ) ) ;
#14946 = EDGE_CURVE ( 'NONE', #29963, #3655, #27547, .T. ) ;
#14947 = ORIENTED_EDGE ( 'NONE', *, *, #29597, .F. ) ;
#14948 = CARTESIAN_POINT ( 'NONE',  ( 159.2576787659436661, -11.08176058204349523, 4.603822987175699488 ) ) ;
#14949 = CARTESIAN_POINT ( 'NONE',  ( 4.763139720814407951, 2.750000000000002665, -57.25000000000002132 ) ) ;
#14950 = CARTESIAN_POINT ( 'NONE',  ( 159.2886751345948255, 5.500000000000005329, 0.000000000000000000 ) ) ;
#14951 = CARTESIAN_POINT ( 'NONE',  ( 3.464101615137757051, -5.999999999999979572, -62.41367513459483973 ) ) ;
#14952 = EDGE_CURVE ( 'NONE', #22988, #371, #28164, .T. ) ;
#14953 = CARTESIAN_POINT ( 'NONE',  ( -5.196152422706601826, 2.999999999999975131, -67.53867513459482552 ) ) ;
#14954 = CARTESIAN_POINT ( 'NONE',  ( -3.608439182435115633, 6.249999999999965361, -72.30801270189222407 ) ) ;
#14955 = CARTESIAN_POINT ( 'NONE',  ( 0.000000000000000000, -9.500000000000008882, 7.500000000000007105 ) ) ;
#14956 = CARTESIAN_POINT ( 'NONE',  ( 158.7976497308104342, 0.000000000000000000, 5.000000000000004441 ) ) ;
#14957 = CARTESIAN_POINT ( 'NONE',  ( -5.196152422706601826, 2.999999999999975131, -149.4613248654052029 ) ) ;
#14958 = CARTESIAN_POINT ( 'NONE',  ( -5.196152422706573404, -3.000000000000002665, -168.7113248654051745 ) ) ;
#14959 =( BOUNDED_CURVE ( )  B_SPLINE_CURVE ( 2, ( #8570, #27290, #119, #13839, #14149, #7028, #13680, #4572, #25772 ),
 .UNSPECIFIED., .F., .T. ) 
 B_SPLINE_CURVE_WITH_KNOTS ( ( 3, 2, 2, 2, 3 ),
 ( 0.8593750000000000000, 0.8671875000000000000, 0.8750000000000000000, 0.8828125000000000000, 0.8906250000000000000 ),
 .UNSPECIFIED. ) 
 CURVE ( )  GEOMETRIC_REPRESENTATION_ITEM ( )  RATIONAL_B_SPLINE_CURVE ( ( 1.000000000000000000, 0.9238795325112867385, 1.000000000000000000, 0.9238795325112867385, 1.000000000000000000, 0.9238795325112867385, 1.000000000000000000, 0.9238795325112867385, 1.000000000000000000 ) ) 
 REPRESENTATION_ITEM ( '' )  );
#14960 = CARTESIAN_POINT ( 'NONE',  ( 4.763139720814407951, -2.749999999999988454, -141.5000000000000284 ) ) ;
#14961 = CARTESIAN_POINT ( 'NONE',  ( -3.608439182435052128, -6.250000000000110134, -154.3080127018922383 ) ) ;
#14962 = DIRECTION ( 'NONE',  ( 0.000000000000000000, 1.224646799147351482E-16, 1.000000000000000000 ) ) ;
#14963 = CARTESIAN_POINT ( 'NONE',  ( 146.3363248654052029, 0.000000000000000000, -5.500000000000005329 ) ) ;
#14964 = CARTESIAN_POINT ( 'NONE',  ( -2.775557561562891351E-14, -5.500000000000115463, -72.75000000000004263 ) ) ;
#14965 = CARTESIAN_POINT ( 'NONE',  ( 3.175426480543072749, -5.500000000000105693, -56.12500000000004263 ) ) ;
#14966 =( BOUNDED_CURVE ( )  B_SPLINE_CURVE ( 2, ( #3306, #22687, #5915, #15496, #24505, #12733, #29259, #22072, #10407 ),
 .UNSPECIFIED., .F., .F. ) 
 B_SPLINE_CURVE_WITH_KNOTS ( ( 3, 2, 2, 2, 3 ),
 ( 0.5138888888888888395, 0.5148148148148148362, 0.5166666666666666075, 0.5185185185185186008, 0.5194444444444444864 ),
 .UNSPECIFIED. ) 
 CURVE ( )  GEOMETRIC_REPRESENTATION_ITEM ( )  RATIONAL_B_SPLINE_CURVE ( ( 0.9330127018922194093, 0.9330127018922154125, 1.000000000000000000, 0.8660254037844388186, 1.000000000000000000, 0.8660254037844388186, 1.000000000000000000, 0.9330127018922194093, 0.9330127018922194093 ) ) 
 REPRESENTATION_ITEM ( '' )  );
#14967 = ORIENTED_EDGE ( 'NONE', *, *, #10438, .T. ) ;
#14968 = CARTESIAN_POINT ( 'NONE',  ( 139.9836002691896510, 4.999999999999989342, -2.071067811865468400 ) ) ;
#14969 = CARTESIAN_POINT ( 'NONE',  ( 150.3750000000000284, 0.000000000000000000, 6.000000000000005329 ) ) ;
#14970 = CARTESIAN_POINT ( 'NONE',  ( -5.999999999999971578, 1.607695154586715303, -126.9033121635129930 ) ) ;
#14971 = CARTESIAN_POINT ( 'NONE',  ( 115.0238248654049329, -0.8284271247460852639, 2.000000000000212275 ) ) ;
#14972 = CARTESIAN_POINT ( 'NONE',  ( 114.4997167782375413, 1.308140751793696044, -1.308140751793640533 ) ) ;
#14973 = VERTEX_POINT ( 'NONE', #23294 ) ;
#14974 = CARTESIAN_POINT ( 'NONE',  ( 141.5625000000000284, -4.242640687119298093, 4.242640687119298093 ) ) ;
#14975 = DIRECTION ( 'NONE',  ( 1.000000000000000000, 0.000000000000000000, 0.000000000000000000 ) ) ;
#14976 = AXIS2_PLACEMENT_3D ( 'NONE', #8375, #27104, #4368 ) ;
#14977 = EDGE_CURVE ( 'NONE', #16308, #8939, #4528, .T. ) ;
#14978 = EDGE_CURVE ( 'NONE', #26678, #23883, #21776, .T. ) ;
#14979 = CARTESIAN_POINT ( 'NONE',  ( -5.999999999999968026, -1.607695154586722186, -158.8466878364870070 ) ) ;
#14980 = CARTESIAN_POINT ( 'NONE',  ( 15.49999999999998579, -1.999999999999835243, 0.000000000000000000 ) ) ;
#14981 = CARTESIAN_POINT ( 'NONE',  ( -3.608439182435052128, -6.250000000000110134, -148.9419872981078186 ) ) ;
#14982 = CARTESIAN_POINT ( 'NONE',  ( -4.763139720814407951, -2.750000000000016431, -85.00000000000001421 ) ) ;
#14983 = B_SPLINE_CURVE_WITH_KNOTS ( 'NONE', 3,
 ( #18379, #3895, #25095, #20215, #22357, #1293, #29563, #5895, #1607, #6215, #20051, #15322, #8681, #17776, #13326, #20506 ),
 .UNSPECIFIED., .F., .F.,
 ( 4, 2, 2, 2, 2, 2, 2, 4 ),
 ( 0.000000000000000000, 0.001747794382750394527, 0.002621691574125591898, 0.003495588765500789487, 0.004369485956875987509, 0.005243383148251184664, 0.006117280339626383553, 0.006991177531001582443 ),
 .UNSPECIFIED. ) ;
#14984 = CARTESIAN_POINT ( 'NONE',  ( 13.43750000000000355, 2.649519052838419153, 1.097466725451559322 ) ) ;
#14985 = CARTESIAN_POINT ( 'NONE',  ( 5.412658773652739619, 3.124999999999988898, -95.18301270189222407 ) ) ;
#14986 = AXIS2_PLACEMENT_3D ( 'NONE', #23998, #8006, #12358 ) ;
#14987 = CARTESIAN_POINT ( 'NONE',  ( 119.9999999999998579, 1.752251084798616354, 1.505035388670107999 ) ) ;
#14988 = FILL_AREA_STYLE ('',( #5583 ) ) ;
#14989 = FACE_OUTER_BOUND ( 'NONE', #1122, .T. ) ;
#14990 = SURFACE_STYLE_FILL_AREA ( #23759 ) ;
#14991 = CARTESIAN_POINT ( 'NONE',  ( 135.1771402107524693, -8.419396982537390883, 8.000000000000008882 ) ) ;
#14992 = CARTESIAN_POINT ( 'NONE',  ( 6.350852961086080661, -9.614813431917819062E-14, -162.3750000000000284 ) ) ;
#14993 = CARTESIAN_POINT ( 'NONE',  ( 136.7738248654052313, -3.889087296526011706, 3.889087296526011706 ) ) ;
#14994 = CARTESIAN_POINT ( 'NONE',  ( -4.763139720814407951, 2.749999999999946709, -149.7500000000000568 ) ) ;
#14995 = CARTESIAN_POINT ( 'NONE',  ( 19.89882486540532724, 1.035533905932809473, 2.499999999999964473 ) ) ;
#14996 = CARTESIAN_POINT ( 'NONE',  ( -4.763139720814407951, 2.749999999999946709, -95.75000000000000000 ) ) ;
#14997 = DIRECTION ( 'NONE',  ( -1.000000000000000000, -1.665334536937731113E-16, 1.526556658859586792E-16 ) ) ;
#14998 = CARTESIAN_POINT ( 'NONE',  ( -5.999999999999904965, -1.607695154586834541, -131.2693375672974412 ) ) ;
#14999 = CARTESIAN_POINT ( 'NONE',  ( 6.350852961086080661, -9.614813431917819062E-14, -81.37500000000004263 ) ) ;
#15000 = CARTESIAN_POINT ( 'NONE',  ( 154.8898502691896795, 3.535533905932725318, -3.535533905932725318 ) ) ;
#15001 = CARTESIAN_POINT ( 'NONE',  ( 141.4761751345948255, 3.889087296526011706, 3.889087296526011706 ) ) ;
#15002 = DIRECTION ( 'NONE',  ( 7.147005652999508048E-36, -5.642372883946980038E-36, -1.000000000000000000 ) ) ;
#15003 =( BOUNDED_CURVE ( )  B_SPLINE_CURVE ( 2, ( #21592, #22032, #14547, #23888, #7886, #3270, #5278, #29072, #5425 ),
 .UNSPECIFIED., .F., .F. ) 
 B_SPLINE_CURVE_WITH_KNOTS ( ( 3, 2, 2, 2, 3 ),
 ( 0.4138888888888888618, 0.4148148148148148584, 0.4166666666666666297, 0.4185185185185185119, 0.4194444444444445086 ),
 .UNSPECIFIED. ) 
 CURVE ( )  GEOMETRIC_REPRESENTATION_ITEM ( )  RATIONAL_B_SPLINE_CURVE ( ( 0.9330127018922194093, 0.9330127018922154125, 1.000000000000000000, 0.8660254037844388186, 1.000000000000000000, 0.8660254037844388186, 1.000000000000000000, 0.9330127018922154125, 0.9330127018922194093 ) ) 
 REPRESENTATION_ITEM ( '' )  );
#15004 = CARTESIAN_POINT ( 'NONE',  ( 1.000000000000000888, -15.13429681935021165, 8.790437860111675050 ) ) ;
#15005 = CARTESIAN_POINT ( 'NONE',  ( 22.06250000000015632, 2.000000000000212275, 0.8284271247461753029 ) ) ;
#15006 =( BOUNDED_CURVE ( )  B_SPLINE_CURVE ( 2, ( #25516, #9559, #16654, #9094, #23245, #13745, #8952, #6935, #30132 ),
 .UNSPECIFIED., .F., .F. ) 
 B_SPLINE_CURVE_WITH_KNOTS ( ( 3, 2, 2, 2, 3 ),
 ( 0.7972222222222222765, 0.7981481481481481621, 0.8000000000000000444, 0.8018518518518518157, 0.8027777777777777013 ),
 .UNSPECIFIED. ) 
 CURVE ( )  GEOMETRIC_REPRESENTATION_ITEM ( )  RATIONAL_B_SPLINE_CURVE ( ( 0.9330127018922194093, 0.9330127018922234061, 1.000000000000000000, 0.8660254037844388186, 1.000000000000000000, 0.8660254037844388186, 1.000000000000000000, 0.9330127018922234061, 0.9330127018922194093 ) ) 
 REPRESENTATION_ITEM ( '' )  );
#15007 = CARTESIAN_POINT ( 'NONE',  ( 0.000000000000000000, 5.999999999999977796, -128.7113248654052029 ) ) ;
#15008 = DIRECTION ( 'NONE',  ( 1.000000000000000000, 0.000000000000000000, 0.000000000000000000 ) ) ;
#15009 = CARTESIAN_POINT ( 'NONE',  ( 149.3363248654052029, 0.000000000000000000, -5.500000000000005329 ) ) ;
#15010 = EDGE_LOOP ( 'NONE', ( #6303, #16717, #16563, #11565 ) ) ;
#15011 = AXIS2_PLACEMENT_3D ( 'NONE', #29616, #29916, #22721 ) ;
#15012 = SURFACE_SIDE_STYLE ('',( #20233 ) ) ;
#15013 = CARTESIAN_POINT ( 'NONE',  ( 0.000000000000000000, -15.50000000000001421, -5.656854249492387687 ) ) ;
#15014 = CARTESIAN_POINT ( 'NONE',  ( 146.1636751345948255, 0.000000000000000000, 5.500000000000005329 ) ) ;
#15015 = CARTESIAN_POINT ( 'NONE',  ( 119.8127832217621460, -1.849990392679381701, 0.7662911109078287542 ) ) ;
#15016 = CARTESIAN_POINT ( 'NONE',  ( 24.95223159194603468, 1.828742805381509795, -0.9313548736353307600 ) ) ;
#15017 = VERTEX_POINT ( 'NONE', #4671 ) ;
#15018 = EDGE_CURVE ( 'NONE', #15083, #9807, #8197, .T. ) ;
#15019 = CARTESIAN_POINT ( 'NONE',  ( 146.8125000000000284, 4.242640687119298093, -4.242640687119298093 ) ) ;
#15020 = ORIENTED_EDGE ( 'NONE', *, *, #24154, .F. ) ;
#15021 = AXIS2_PLACEMENT_3D ( 'NONE', #2195, #16213, #9411 ) ;
#15022 = CARTESIAN_POINT ( 'NONE',  ( 4.763139720814407951, -2.749999999999988454, -105.5000000000000426 ) ) ;
#15023 = CARTESIAN_POINT ( 'NONE',  ( 3.608439182435180470, -6.249999999999997335, -115.0580127018922383 ) ) ;
#15024 = ORIENTED_EDGE ( 'NONE', *, *, #46, .F. ) ;
#15025 = CARTESIAN_POINT ( 'NONE',  ( 0.000000000000000000, 0.000000000000000000, 0.000000000000000000 ) ) ;
#15026 = CARTESIAN_POINT ( 'NONE',  ( -5.412658773652684552, -3.125000000000099920, -161.0669872981078754 ) ) ;
#15027 = CARTESIAN_POINT ( 'NONE',  ( 106.2499999999999716, -2.775557561562891351E-14, 2.499999999999946709 ) ) ;
#15028 = CARTESIAN_POINT ( 'NONE',  ( 2.775557561562891351E-14, 6.250000000000033751, -58.93301270189221697 ) ) ;
#15029 = ORIENTED_EDGE ( 'NONE', *, *, #10090, .F. ) ;
#15030 = DIRECTION ( 'NONE',  ( -1.000000000000000000, -1.665334536937731113E-16, 1.526556658859586792E-16 ) ) ;
#15031 = CARTESIAN_POINT ( 'NONE',  ( -4.754775042825807319, 9.920200456738779593, -21.33539821540184889 ) ) ;
#15032 = CYLINDRICAL_SURFACE ( 'NONE', #24584, 2.499999999999999112 ) ;
#15033 = CARTESIAN_POINT ( 'NONE',  ( -2.775557561562891351E-14, -5.500000000000115463, -174.7500000000000284 ) ) ;
#15034 = CARTESIAN_POINT ( 'NONE',  ( 119.4999999999999289, -2.499999999999919176, 0.000000000000000000 ) ) ;
#15035 = CARTESIAN_POINT ( 'NONE',  ( 152.8988248654052313, 3.889087296526011706, 3.889087296526011706 ) ) ;
#15036 = CARTESIAN_POINT ( 'NONE',  ( 2.775557561562891351E-14, -6.250000000000061284, -167.6830127018922383 ) ) ;
#15037 = CARTESIAN_POINT ( 'NONE',  ( 154.7738248654052029, -3.889087296526011706, 3.889087296526011706 ) ) ;
#15038 = DIRECTION ( 'NONE',  ( -7.147005652999508048E-36, 5.642372883946980038E-36, 1.000000000000000000 ) ) ;
#15039 = CARTESIAN_POINT ( 'NONE',  ( -4.763139720814407951, -2.750000000000016431, -118.0000000000000000 ) ) ;
#15040 = CYLINDRICAL_SURFACE ( 'NONE', #24701, 2.000000000000012879 ) ;
#15042 = CARTESIAN_POINT ( 'NONE',  ( 6.350852961086080661, -9.614813431917819062E-14, -103.8750000000000000 ) ) ;
#15041 = CIRCLE ( 'NONE', #4718, 16.50000000000000355 ) ;
#15043 = CARTESIAN_POINT ( 'NONE',  ( -5.999999999999982236, -1.607695154586700426, -131.8466878364870354 ) ) ;
#15044 = ORIENTED_EDGE ( 'NONE', *, *, #2331, .F. ) ;
#15045 = CARTESIAN_POINT ( 'NONE',  ( 13.62500000000002665, 2.649519052838444910, -5.551115123125782702E-14 ) ) ;
#15046 = EDGE_CURVE ( 'NONE', #1053, #24844, #11488, .T. ) ;
#15047 = CARTESIAN_POINT ( 'NONE',  ( 119.6874999999998010, -1.035533905932809473, -2.499999999999784173 ) ) ;
#15048 = CARTESIAN_POINT ( 'NONE',  ( 0.000000000000000000, -5.999999999999991118, -76.03867513459483973 ) ) ;
#15049 = ORIENTED_EDGE ( 'NONE', *, *, #6689, .F. ) ;
#15050 = CARTESIAN_POINT ( 'NONE',  ( 139.0238248654052029, 3.889087296526011706, -3.889087296526011706 ) ) ;
#15051 = COLOUR_RGB ( '', 0.31764706, 0.68627451, 0.89019608) ;
#15052 = CARTESIAN_POINT ( 'NONE',  ( 2.775557561562891351E-14, -6.250000000000061284, -84.31698729810783277 ) ) ;
#15053 = DIRECTION ( 'NONE',  ( 1.000000000000000000, -5.551115123125773458E-17, -1.260129944081490338E-35 ) ) ;
#15054 = VERTEX_POINT ( 'NONE', #13794 ) ;
#15055 = PRESENTATION_LAYER_ASSIGNMENT (  '', '', ( #25329 ) ) ;
#15056 = CARTESIAN_POINT ( 'NONE',  ( -6.000000000000000888, 1.067854986875958443E-15, 7.560779664488942560E-35 ) ) ;
#15057 =( BOUNDED_CURVE ( )  B_SPLINE_CURVE ( 2, ( #15825, #26810, #13510, #27129, #22701, #15510, #11039, #8401, #15667 ),
 .UNSPECIFIED., .F., .T. ) 
 B_SPLINE_CURVE_WITH_KNOTS ( ( 3, 2, 2, 2, 3 ),
 ( 0.8916666666666666075, 0.8925925925925926041, 0.8944444444444444864, 0.8962962962962962576, 0.8972222222222222543 ),
 .UNSPECIFIED. ) 
 CURVE ( )  GEOMETRIC_REPRESENTATION_ITEM ( )  RATIONAL_B_SPLINE_CURVE ( ( 0.9330127018922194093, 0.9330127018922154125, 1.000000000000000000, 0.8660254037844388186, 1.000000000000000000, 0.8660254037844388186, 1.000000000000000000, 0.9330127018922154125, 0.9330127018922194093 ) ) 
 REPRESENTATION_ITEM ( '' )  );
#15058 = EDGE_CURVE ( 'NONE', #22104, #9807, #13634, .T. ) ;
#15059 = VERTEX_POINT ( 'NONE', #20673 ) ;
#15060 = CIRCLE ( 'NONE', #1792, 1.000000000000000888 ) ;
#15061 = CARTESIAN_POINT ( 'NONE',  ( 135.8586002691897079, 2.071067811865468400, 4.999999999999989342 ) ) ;
#15062 = ORIENTED_EDGE ( 'NONE', *, *, #6087, .T. ) ;
#15063 = CARTESIAN_POINT ( 'NONE',  ( 2.775557561562891351E-14, -6.250000000000061284, -135.3169872981078186 ) ) ;
#15064 = FACE_OUTER_BOUND ( 'NONE', #20553, .T. ) ;
#15065 = CARTESIAN_POINT ( 'NONE',  ( 3.464101615137852974, 5.999999999999884537, -83.83632486540517448 ) ) ;
#15066 = CARTESIAN_POINT ( 'NONE',  ( 3.464101615137852974, 5.999999999999884537, -47.83632486540520290 ) ) ;
#15067 = EDGE_LOOP ( 'NONE', ( #24899, #265, #7041, #16521 ) ) ;
#15068 = CARTESIAN_POINT ( 'NONE',  ( 14.37500000000016520, -1.414213562373034527, 1.414213562372979016 ) ) ;
#15069 = CARTESIAN_POINT ( 'NONE',  ( 0.9867988441837158842, -16.18254354104136539, -6.670981548062425048 ) ) ;
#15070 = CARTESIAN_POINT ( 'NONE',  ( 161.0000000000000284, 0.000000000000000000, 0.000000000000000000 ) ) ;
#15071 = CARTESIAN_POINT ( 'NONE',  ( -3.464101615137725076, 5.999999999999979572, -56.58632486540519579 ) ) ;
#15072 = CARTESIAN_POINT ( 'NONE',  ( 134.9851497308104058, -3.535533905932725318, 3.535533905932725318 ) ) ;
#15073 = CARTESIAN_POINT ( 'NONE',  ( -4.999999999999990230, -55.00000000000002132, 7.500000000000007105 ) ) ;
#15074 = LINE ( 'NONE', #13252, #30073 ) ;
#15075 = CARTESIAN_POINT ( 'NONE',  ( -5.412658773652739619, 3.124999999999975131, -66.81698729810780435 ) ) ;
#15076 = CARTESIAN_POINT ( 'NONE',  ( 2.775557561562891351E-14, 6.250000000000033751, -52.06698729810782567 ) ) ;
#15077 = CARTESIAN_POINT ( 'NONE',  ( 6.000000000000000000, 2.951592740943527306E-14, -152.1636751345948255 ) ) ;
#15078 = CARTESIAN_POINT ( 'NONE',  ( -5.999999999999963585, 1.780251999655701777E-13, -102.8363248654052313 ) ) ;
#15079 = CARTESIAN_POINT ( 'NONE',  ( -40.00000000000000000, -20.00000000000021316, 4.000000000000003553 ) ) ;
#15080 = VECTOR ( 'NONE', #27222, 1000.000000000000000 ) ;
#15081 = CARTESIAN_POINT ( 'NONE',  ( 3.175426480543072749, 5.499999999999865885, -130.6250000000000284 ) ) ;
#15082 = CYLINDRICAL_SURFACE ( 'NONE', #7782, 5.500000000000000000 ) ;
#15083 = VERTEX_POINT ( 'NONE', #20829 ) ;
#15084 = CARTESIAN_POINT ( 'NONE',  ( 13.02382486540521001, -1.035533905932629173, 2.499999999999964473 ) ) ;
#15085 = EDGE_CURVE ( 'NONE', #25883, #27076, #1950, .T. ) ;
#15086 = CARTESIAN_POINT ( 'NONE',  ( 6.000000000000052403, 1.607695154586625819, -120.0193375672974412 ) ) ;
#15087 = CARTESIAN_POINT ( 'NONE',  ( 3.464101615137757051, -5.999999999999979572, -159.9136751345947971 ) ) ;
#15088 = DIRECTION ( 'NONE',  ( 0.000000000000000000, 0.000000000000000000, -1.000000000000000000 ) ) ;
#15089 = CARTESIAN_POINT ( 'NONE',  ( 108.6636751345948113, -1.414213562373062283, 1.414213562373256572 ) ) ;
#15090 = ORIENTED_EDGE ( 'NONE', *, *, #26937, .F. ) ;
#15091 = CIRCLE ( 'NONE', #17556, 15.00000000000000000 ) ;
#15092 = CARTESIAN_POINT ( 'NONE',  ( 113.6247167782374987, 1.849990392679551343, 0.000000000000000000 ) ) ;
#15093 = CARTESIAN_POINT ( 'NONE',  ( 118.7261751345945981, -1.999999999999941602, 0.8284271247463557142 ) ) ;
#15094 = CARTESIAN_POINT ( 'NONE',  ( 3.608439182435180470, 6.249999999999982236, -95.69198729810780435 ) ) ;
#15095 = FILL_AREA_STYLE_COLOUR ( '', #10702 ) ;
#15096 = ADVANCED_FACE ( 'NONE', ( #9296 ), #16401, .T. ) ;
#15097 = DIRECTION ( 'NONE',  ( -6.938893903907221278E-15, -1.000000000000000000, 0.000000000000000000 ) ) ;
#15098 = CARTESIAN_POINT ( 'NONE',  ( 113.6874999999998437, -1.035533905932749299, -2.499999999999904521 ) ) ;
#15099 = EDGE_CURVE ( 'NONE', #11502, #20769, #24491, .T. ) ;
#15100 = CARTESIAN_POINT ( 'NONE',  ( 152.1636751345948255, 0.000000000000000000, 5.500000000000005329 ) ) ;
#15101 = ORIENTED_EDGE ( 'NONE', *, *, #16372, .T. ) ;
#15102 = CARTESIAN_POINT ( 'NONE',  ( 140.6985356443576620, -11.69853564435969773, 4.029618091915731171 ) ) ;
#15103 = CIRCLE ( 'NONE', #1842, 1.000000000000000000 ) ;
#15104 = EDGE_LOOP ( 'NONE', ( #9615, #27350, #7490, #18551 ) ) ;
#15105 = CARTESIAN_POINT ( 'NONE',  ( 10.25000000000000888, 5.551115123125782702E-14, 2.000000000000001776 ) ) ;
#15106 = CARTESIAN_POINT ( 'NONE',  ( 0.000000000000000000, 5.999999999999977796, -81.28867513459481131 ) ) ;
#15107 = CARTESIAN_POINT ( 'NONE',  ( 4.763139720814407951, -2.749999999999988454, -48.49999999999998579 ) ) ;
#15108 =( BOUNDED_CURVE ( )  B_SPLINE_CURVE ( 2, ( #621, #29157, #12782, #7821, #21684, #3512, #26563, #22277, #21974 ),
 .UNSPECIFIED., .F., .F. ) 
 B_SPLINE_CURVE_WITH_KNOTS ( ( 3, 2, 2, 2, 3 ),
 ( 0.3416666666666666741, 0.3425925925925926152, 0.3444444444444444420, 0.3462962962962962687, 0.3472222222222222099 ),
 .UNSPECIFIED. ) 
 CURVE ( )  GEOMETRIC_REPRESENTATION_ITEM ( )  RATIONAL_B_SPLINE_CURVE ( ( 0.9330127018922194093, 0.9330127018922194093, 1.000000000000000000, 0.8660254037844388186, 1.000000000000000000, 0.8660254037844388186, 1.000000000000000000, 0.9330127018922194093, 0.9330127018922194093 ) ) 
 REPRESENTATION_ITEM ( '' )  );
#15109 = CARTESIAN_POINT ( 'NONE',  ( -5.999999999999963585, 1.780251999655701777E-13, -65.91367513459482552 ) ) ;
#15110 = CARTESIAN_POINT ( 'NONE',  ( 2.775557561562891351E-14, 6.250000000000033751, -75.43301270189223828 ) ) ;
#15111 = CARTESIAN_POINT ( 'NONE',  ( 124.9999999999999432, -71.00000000000001421, 5.000000000000004441 ) ) ;
#15112 = CARTESIAN_POINT ( 'NONE',  ( 157.1101497308104058, 3.535533905932725318, 3.535533905932725318 ) ) ;
#15113 = AXIS2_PLACEMENT_3D ( 'NONE', #1689, #11087, #20432 ) ;
#15114 = CARTESIAN_POINT ( 'NONE',  ( 152.9136751345948539, 0.000000000000000000, -5.500000000000005329 ) ) ;
#15115 = CARTESIAN_POINT ( 'NONE',  ( 105.7886751345946550, -1.999999999999946265, 0.000000000000000000 ) ) ;
#15116 = CARTESIAN_POINT ( 'NONE',  ( -4.763139720814407951, -2.750000000000016431, -134.5000000000000000 ) ) ;
#15117 = CARTESIAN_POINT ( 'NONE',  ( 3.464101615137757051, -5.999999999999979572, -177.3363248654052313 ) ) ;
#15118 = CARTESIAN_POINT ( 'NONE',  ( 10.46132486540518514, 5.551115123125782702E-14, -2.499999999999946709 ) ) ;
#15119 = CARTESIAN_POINT ( 'NONE',  ( -5.196152422706601826, 2.999999999999975131, -51.03867513459481131 ) ) ;
#15120 = EDGE_CURVE ( 'NONE', #18727, #22602, #29402, .T. ) ;
#15121 = CARTESIAN_POINT ( 'NONE',  ( 6.350852961086080661, -9.614813431917819062E-14, -66.37500000000002842 ) ) ;
#15122 = AXIS2_PLACEMENT_3D ( 'NONE', #19906, #6529, #20229 ) ;
#15123 = CARTESIAN_POINT ( 'NONE',  ( -6.350852961085760029, -1.281975124255709124E-13, -58.12500000000005684 ) ) ;
#15124 = CARTESIAN_POINT ( 'NONE',  ( 6.000000000000000888, -1.859271017917181981E-14, -124.5863248654052171 ) ) ;
#15125 = ORIENTED_EDGE ( 'NONE', *, *, #16980, .F. ) ;
#15126 = CARTESIAN_POINT ( 'NONE',  ( 151.6875000000000284, 4.242640687119269671, 4.242640687119298093 ) ) ;
#15127 = DIRECTION ( 'NONE',  ( -3.885780586188043947E-16, 0.8660254037844514752, 0.4999999999999777955 ) ) ;
#15128 = CARTESIAN_POINT ( 'NONE',  ( 14.06250000000011546, 2.000000000000151879, 0.8284271247461753029 ) ) ;
#15129 = ADVANCED_BREP_SHAPE_REPRESENTATION ( '', ( #14742, #18805 ), #1599 ) ;
#15130 = CARTESIAN_POINT ( 'NONE',  ( 113.5622167782373850, 1.849990392679621953, -0.7662911109075283278 ) ) ;
#15131 = EDGE_CURVE ( 'NONE', #20541, #8489, #29186, .T. ) ;
#15132 = EDGE_CURVE ( 'NONE', #3491, #16367, #12217, .T. ) ;
#15133 = ORIENTED_EDGE ( 'NONE', *, *, #25087, .T. ) ;
#15134 = CARTESIAN_POINT ( 'NONE',  ( 146.7187500000000284, 2.485281374238555774, -6.000000000000005329 ) ) ;
#15135 = CARTESIAN_POINT ( 'NONE',  ( 143.1488248654052029, -3.889087296526011706, -3.889087296526011706 ) ) ;
#15136 = AXIS2_PLACEMENT_3D ( 'NONE', #5527, #7990, #7836 ) ;
#15137 = CARTESIAN_POINT ( 'NONE',  ( 4.763139720814407951, -2.749999999999988454, -149.0000000000000284 ) ) ;
#15138 = CARTESIAN_POINT ( 'NONE',  ( 17.50000000000007105, -1.999999999999835243, -5.551115123125782702E-14 ) ) ;
#15139 = VERTEX_POINT ( 'NONE', #17724 ) ;
#15140 = CARTESIAN_POINT ( 'NONE',  ( 5.412658773652739619, 3.124999999999988898, -146.8169872981078186 ) ) ;
#15141 = CARTESIAN_POINT ( 'NONE',  ( 6.350852961086080661, -9.614813431917819062E-14, -82.87500000000004263 ) ) ;
#15142 =( BOUNDED_CURVE ( )  B_SPLINE_CURVE ( 2, ( #6869, #3001, #26491, #848, #17022, #3145, #10249, #14856, #19607 ),
 .UNSPECIFIED., .F., .T. ) 
 B_SPLINE_CURVE_WITH_KNOTS ( ( 3, 2, 2, 2, 3 ),
 ( 0.7194444444444444420, 0.7203703703703703276, 0.7222222222222222099, 0.7240740740740740922, 0.7249999999999999778 ),
 .UNSPECIFIED. ) 
 CURVE ( )  GEOMETRIC_REPRESENTATION_ITEM ( )  RATIONAL_B_SPLINE_CURVE ( ( 0.9330127018922194093, 0.9330127018922194093, 1.000000000000000000, 0.8660254037844388186, 1.000000000000000000, 0.8660254037844388186, 1.000000000000000000, 0.9330127018922194093, 0.9330127018922194093 ) ) 
 REPRESENTATION_ITEM ( '' )  );
#15143 = CARTESIAN_POINT ( 'NONE',  ( -3.608439182435052128, -6.250000000000110134, -97.30801270189220986 ) ) ;
#15144 = VERTEX_POINT ( 'NONE', #20623 ) ;
#15145 = CARTESIAN_POINT ( 'NONE',  ( -3.464101615137757051, -5.999999999999979572, -128.0863248654052029 ) ) ;
#15146 =( LENGTH_UNIT ( ) NAMED_UNIT ( * ) SI_UNIT ( .MILLI., .METRE. ) );
#15147 = CARTESIAN_POINT ( 'NONE',  ( 148.3988248654052313, 3.889087296526011706, 3.889087296526011706 ) ) ;
#15148 = DIRECTION ( 'NONE',  ( 0.000000000000000000, -0.8787878787878796727, 0.4772125984249564468 ) ) ;
#15149 = PRESENTATION_STYLE_ASSIGNMENT (( #5741 ) ) ;
#15150 = CARTESIAN_POINT ( 'NONE',  ( -3.175426480542816066, 5.499999999999865885, -154.3749999999999716 ) ) ;
#15151 = CARTESIAN_POINT ( 'NONE',  ( 118.0238248654050182, -0.8284271247461153509, 2.000000000000212275 ) ) ;
#15152 = CARTESIAN_POINT ( 'NONE',  ( -4.763139720814407951, 2.749999999999946709, -143.7500000000000568 ) ) ;
#15153 = PRESENTATION_STYLE_ASSIGNMENT (( #27819 ) ) ;
#15154 = EDGE_CURVE ( 'NONE', #4691, #6944, #11026, .T. ) ;
#15155 = CARTESIAN_POINT ( 'NONE',  ( -4.763139720814407951, -2.750000000000016431, -98.50000000000002842 ) ) ;
#15156 = CARTESIAN_POINT ( 'NONE',  ( 104.1247167782375556, -1.849990392679468076, 0.000000000000000000 ) ) ;
#15157 = CARTESIAN_POINT ( 'NONE',  ( 116.0000000000000142, 0.000000000000000000, 0.000000000000000000 ) ) ;
#15158 = CARTESIAN_POINT ( 'NONE',  ( -2.775557561562891351E-14, -5.500000000000115463, -78.74999999999998579 ) ) ;
#15159 = DIRECTION ( 'NONE',  ( -8.326672684688675286E-17, -2.081668171172168821E-17, 1.000000000000000000 ) ) ;
#15160 = CARTESIAN_POINT ( 'NONE',  ( 152.2648502691896510, 3.535533905932725318, 3.535533905932752852 ) ) ;
#15161 = CARTESIAN_POINT ( 'NONE',  ( 150.4761751345948255, 3.889087296526011706, 3.889087296526011706 ) ) ;
#15162 = CARTESIAN_POINT ( 'NONE',  ( 17.96132486540527751, 1.110223024625156540E-13, 2.499999999999946709 ) ) ;
#15163 = CARTESIAN_POINT ( 'NONE',  ( 6.000000000000000888, 7.762456499804234384E-14, -129.0863248654052029 ) ) ;
#15164 = CARTESIAN_POINT ( 'NONE',  ( -3.464101615137725076, 5.999999999999979572, -72.16367513459481131 ) ) ;
#15165 = ADVANCED_FACE ( 'NONE', ( #8796 ), #18182, .T. ) ;
#15166 = CARTESIAN_POINT ( 'NONE',  ( 6.000000000000000888, 1.743066579297358182E-13, -75.66367513459485394 ) ) ;
#15167 = ORIENTED_EDGE ( 'NONE', *, *, #24053, .T. ) ;
#15168 =( NAMED_UNIT ( * ) SI_UNIT ( $, .STERADIAN. ) SOLID_ANGLE_UNIT ( ) );
#15169 = CARTESIAN_POINT ( 'NONE',  ( -9.529120656610874963E-19, -15.46245447015412111, 5.965482872545659454 ) ) ;
#15170 = CARTESIAN_POINT ( 'NONE',  ( 0.000000000000000000, 5.999999999999977796, -80.71132486540521711 ) ) ;
#15171 = CARTESIAN_POINT ( 'NONE',  ( 104.4372167782374419, 0.7662911109077987781, -1.849990392679231599 ) ) ;
#15172 = EDGE_LOOP ( 'NONE', ( #29719, #3619, #24552, #16531, #29418, #6347, #20237, #18356, #25386 ) ) ;
#15173 = EDGE_LOOP ( 'NONE', ( #10690, #23155 ) ) ;
#15174 = CARTESIAN_POINT ( 'NONE',  ( 0.000000000000000000, 5.499999999999991118, -103.5000000000000426 ) ) ;
#15175 = CARTESIAN_POINT ( 'NONE',  ( 3.608439182435180470, 6.249999999999982236, -113.0580127018922241 ) ) ;
#15176 = ORIENTED_EDGE ( 'NONE', *, *, #28913, .F. ) ;
#15177 = FACE_OUTER_BOUND ( 'NONE', #633, .T. ) ;
#15178 = CARTESIAN_POINT ( 'NONE',  ( -5.412658773652684552, -3.125000000000099920, -156.5669872981078186 ) ) ;
#15179 = CARTESIAN_POINT ( 'NONE',  ( 105.3124999999998437, -1.035533905932598975, 2.500000000000265121 ) ) ;
#15180 = CARTESIAN_POINT ( 'NONE',  ( -0.5000000000000004441, -15.00000000000001421, 7.500000000000007105 ) ) ;
#15181 = CARTESIAN_POINT ( 'NONE',  ( 3.608439182435180470, -6.249999999999997335, -55.05801270189220276 ) ) ;
#15182 = MECHANICAL_DESIGN_GEOMETRIC_PRESENTATION_REPRESENTATION (  '', ( #11281 ), #18644 ) ;
#15183 = ORIENTED_EDGE ( 'NONE', *, *, #22620, .T. ) ;
#15184 = FACE_OUTER_BOUND ( 'NONE', #21486, .T. ) ;
#15185 = CARTESIAN_POINT ( 'NONE',  ( -6.000000000000000888, 1.067854986875958443E-15, 7.560779664488942560E-35 ) ) ;
#15186 = PRESENTATION_LAYER_ASSIGNMENT (  '', '', ( #18137 ) ) ;
#15187 = CARTESIAN_POINT ( 'NONE',  ( 146.4449251345949108, -5.500000000000012434, 2.278174593052012309 ) ) ;
#15188 = CARTESIAN_POINT ( 'NONE',  ( 119.1488248654049187, -1.999999999999941602, 0.8284271247464759513 ) ) ;
#15189 = CARTESIAN_POINT ( 'NONE',  ( 0.000000000000000000, 5.499999999999991118, -168.0000000000000284 ) ) ;
#15190 = CARTESIAN_POINT ( 'NONE',  ( 105.1877832217621176, 0.7662911109078588412, -1.849990392679291551 ) ) ;
#15191 =( REPRESENTATION_RELATIONSHIP ('NONE','NONE', #103, #4035 ) REPRESENTATION_RELATIONSHIP_WITH_TRANSFORMATION ( #19122 )SHAPE_REPRESENTATION_RELATIONSHIP( ) );
#15192 = CARTESIAN_POINT ( 'NONE',  ( 3.464101615137757051, -5.999999999999979572, -157.8363248654052029 ) ) ;
#15193 = CARTESIAN_POINT ( 'NONE',  ( 3.608439182435180470, 6.249999999999982236, -171.5580127018922667 ) ) ;
#15194 = CARTESIAN_POINT ( 'NONE',  ( -0.9018315097318243545, -9.098168490268061959, 4.000092554054210936 ) ) ;
#15195 = CARTESIAN_POINT ( 'NONE',  ( 25.00000000000013500, 2.000000000000279332, -5.551115123125782702E-14 ) ) ;
#15196 = EDGE_CURVE ( 'NONE', #17215, #19511, #27848, .T. ) ;
#15197 = CARTESIAN_POINT ( 'NONE',  ( 159.8511751345948539, -3.889087296526011706, 3.889087296526011706 ) ) ;
#15198 = ADVANCED_FACE ( 'NONE', ( #15589 ), #26941, .T. ) ;
#15199 = CARTESIAN_POINT ( 'NONE',  ( 4.763139720814407951, 2.750000000000002665, -105.2500000000000142 ) ) ;
#15200 = DIRECTION ( 'NONE',  ( 5.551115123125785167E-17, -1.000000000000000000, -8.881784197001256268E-16 ) ) ;
#15201 = SURFACE_STYLE_USAGE ( .BOTH. , #29604 ) ;
#15202 = CARTESIAN_POINT ( 'NONE',  ( 6.000000000000052403, 1.607695154586625819, -145.5193375672974128 ) ) ;
#15203 = ORIENTED_EDGE ( 'NONE', *, *, #24816, .T. ) ;
#15204 = CARTESIAN_POINT ( 'NONE',  ( 16.18750000000005684, -2.649519052838298805, -1.097466725451499370 ) ) ;
#15205 = CARTESIAN_POINT ( 'NONE',  ( 6.000000000000000888, 1.743066579297358182E-13, -90.08632486540521711 ) ) ;
#15206 = LINE ( 'NONE', #24394, #12513 ) ;
#15207 = EDGE_LOOP ( 'NONE', ( #9994, #3989, #19490, #5992 ) ) ;
#15208 = CARTESIAN_POINT ( 'NONE',  ( 3.175426480543072749, 5.499999999999865885, -159.1250000000000000 ) ) ;
#15209 = CARTESIAN_POINT ( 'NONE',  ( 3.464101615137852974, 5.999999999999884537, -156.4136751345947403 ) ) ;
#15210 = CARTESIAN_POINT ( 'NONE',  ( 5.412658773652712085, -3.125000000000086153, -78.06698729810779014 ) ) ;
#15211 = CONICAL_SURFACE ( 'NONE', #23562, 6.500000000000016875, 0.7419472680059175929 ) ;
#15212 = CARTESIAN_POINT ( 'NONE',  ( 136.0000000000000284, -9.165151389911669000, 8.000000000000007105 ) ) ;
#15213 = VERTEX_POINT ( 'NONE', #3853 ) ;
#15214 = VECTOR ( 'NONE', #1919, 1000.000000000000000 ) ;
#15215 = AXIS2_PLACEMENT_3D ( 'NONE', #8086, #1028, #26232 ) ;
#15216 = ORIENTED_EDGE ( 'NONE', *, *, #28548, .F. ) ;
#15217 = ORIENTED_EDGE ( 'NONE', *, *, #26541, .F. ) ;
#15218 = CARTESIAN_POINT ( 'NONE',  ( 157.1250000000000284, 0.000000000000000000, -6.000000000000005329 ) ) ;
#15219 = AXIS2_PLACEMENT_3D ( 'NONE', #5436, #242, #28339 ) ;
#15220 = CARTESIAN_POINT ( 'NONE',  ( -5.412658773652739619, 3.124999999999975131, -136.6830127018922099 ) ) ;
#15221 = CARTESIAN_POINT ( 'NONE',  ( 2.775557561562891351E-14, 6.250000000000033751, -130.0669872981078470 ) ) ;
#15222 = CARTESIAN_POINT ( 'NONE',  ( 2.775557561562891351E-14, 6.250000000000033751, -181.0669872981078186 ) ) ;
#15223 = CARTESIAN_POINT ( 'NONE',  ( 3.175426480543072749, -5.500000000000105693, -173.1250000000000284 ) ) ;
#15224 = FACE_OUTER_BOUND ( 'NONE', #18857, .T. ) ;
#15225 = CARTESIAN_POINT ( 'NONE',  ( 0.000000000000000000, 5.999999999999977796, -47.71132486540518869 ) ) ;
#15226 = ORIENTED_EDGE ( 'NONE', *, *, #28782, .F. ) ;
#15227 = CARTESIAN_POINT ( 'NONE',  ( 16.12500000000002842, 1.414213562373201061, 1.414213562373034527 ) ) ;
#15228 = CARTESIAN_POINT ( 'NONE',  ( 0.8616410392485300829, -15.74614809565155404, -7.643977401085323642 ) ) ;
#15229 = FACE_OUTER_BOUND ( 'NONE', #30087, .T. ) ;
#15230 = CYLINDRICAL_SURFACE ( 'NONE', #1459, 5.500000000000000000 ) ;
#15231 = CARTESIAN_POINT ( 'NONE',  ( -4.999999999999990230, -55.00000000000002132, 7.500000000000007105 ) ) ;
#15232 = CARTESIAN_POINT ( 'NONE',  ( 6.000000000000052403, -1.607695154586662678, -107.2306624327026157 ) ) ;
#15233 = CARTESIAN_POINT ( 'NONE',  ( 0.1092220458218999685, -15.15144499995605365, -8.760684001891156925 ) ) ;
#15234 = CARTESIAN_POINT ( 'NONE',  ( -5.412658773652739619, 3.124999999999975131, -69.81698729810781856 ) ) ;
#15235 = CARTESIAN_POINT ( 'NONE',  ( 5.412658773652739619, 3.124999999999988898, -56.81698729810780435 ) ) ;
#15236 = DIRECTION ( 'NONE',  ( 1.000000000000000000, 0.000000000000000000, 0.000000000000000000 ) ) ;
#15237 = CARTESIAN_POINT ( 'NONE',  ( 3.464101615137852974, 5.999999999999884537, -103.3363248654052171 ) ) ;
#15238 = CARTESIAN_POINT ( 'NONE',  ( -3.464101615137725076, 5.999999999999979572, -127.6636751345948113 ) ) ;
#15239 = AXIS2_PLACEMENT_3D ( 'NONE', #615, #19085, #9848 ) ;
#15240 = EDGE_CURVE ( 'NONE', #18697, #8808, #11301, .T. ) ;
#15241 = CARTESIAN_POINT ( 'NONE',  ( -3.175426480542816510, 5.499999999999865885, -130.3750000000000284 ) ) ;
#15242 = CARTESIAN_POINT ( 'NONE',  ( -5.999999999999971578, 1.607695154586715303, -166.4806624327026157 ) ) ;
#15243 = ORIENTED_EDGE ( 'NONE', *, *, #5834, .T. ) ;
#15244 = CARTESIAN_POINT ( 'NONE',  ( 24.37500000000006395, 1.110223024625156540E-13, -2.649519052838278377 ) ) ;
#15245 = CARTESIAN_POINT ( 'NONE',  ( -0.5000000000000004441, -9.500000000000008882, -5.000000000000004441 ) ) ;
#15246 = CARTESIAN_POINT ( 'NONE',  ( -5.999999999999963585, -1.487416814333745711E-14, -96.83632486540520290 ) ) ;
#15247 = CARTESIAN_POINT ( 'NONE',  ( -5.196152422706573404, -3.000000000000002665, -100.2886751345948255 ) ) ;
#15248 = DIRECTION ( 'NONE',  ( 1.000000000000000000, 0.000000000000000000, 0.000000000000000000 ) ) ;
#15249 =( BOUNDED_CURVE ( )  B_SPLINE_CURVE ( 2, ( #18871, #13670, #4705, #11519, #23173, #20860, #9488, #14139, #11362 ),
 .UNSPECIFIED., .F., .T. ) 
 B_SPLINE_CURVE_WITH_KNOTS ( ( 3, 2, 2, 2, 3 ),
 ( 0.8361111111111111382, 0.8370370370370370239, 0.8388888888888889062, 0.8407407407407407884, 0.8416666666666666741 ),
 .UNSPECIFIED. ) 
 CURVE ( )  GEOMETRIC_REPRESENTATION_ITEM ( )  RATIONAL_B_SPLINE_CURVE ( ( 0.9330127018922194093, 0.9330127018922194093, 1.000000000000000000, 0.8660254037844388186, 1.000000000000000000, 0.8660254037844388186, 1.000000000000000000, 0.9330127018922194093, 0.9330127018922194093 ) ) 
 REPRESENTATION_ITEM ( '' )  );
#15250 = ORIENTED_EDGE ( 'NONE', *, *, #1691, .F. ) ;
#15251 = CARTESIAN_POINT ( 'NONE',  ( 113.5622167782373850, 1.849990392679621953, -0.7662911109075283278 ) ) ;
#15252 = CARTESIAN_POINT ( 'NONE',  ( 0.000000000000000000, 5.999999999999977796, -71.71132486540521711 ) ) ;
#15253 = CARTESIAN_POINT ( 'NONE',  ( 10.25000000000000888, 5.551115123125782702E-14, 2.000000000000001776 ) ) ;
#15254 = CARTESIAN_POINT ( 'NONE',  ( 2.775557561562891351E-14, 6.250000000000033751, -94.06698729810780435 ) ) ;
#15255 = CARTESIAN_POINT ( 'NONE',  ( 0.000000000000000000, -5.999999999999991118, -173.5386751345948539 ) ) ;
#15256 = CARTESIAN_POINT ( 'NONE',  ( 106.2113248654051745, -1.999999999999946265, 0.000000000000000000 ) ) ;
#15257 = CARTESIAN_POINT ( 'NONE',  ( 112.3749999999999289, -1.767766952966320915, 1.767766952966431937 ) ) ;
#15258 = VERTEX_POINT ( 'NONE', #4011 ) ;
#15259 = CARTESIAN_POINT ( 'NONE',  ( 0.000000000000000000, 0.000000000000000000, 0.000000000000000000 ) ) ;
#15260 = AXIS2_PLACEMENT_3D ( 'NONE', #9203, #18142, #16718 ) ;
#15261 = AXIS2_PLACEMENT_3D ( 'NONE', #18029, #20448, #11423 ) ;
#15262 = ORIENTED_EDGE ( 'NONE', *, *, #29570, .F. ) ;
#15263 = CARTESIAN_POINT ( 'NONE',  ( 24.75000000000015987, -1.873492889144789952, 1.873492889144845464 ) ) ;
#15264 = CARTESIAN_POINT ( 'NONE',  ( 3.464101615137852974, 5.999999999999884537, -81.41367513459479710 ) ) ;
#15265 = EDGE_CURVE ( 'NONE', #18576, #19330, #30281, .T. ) ;
#15266 = LINE ( 'NONE', #11110, #25538 ) ;
#15267 = CARTESIAN_POINT ( 'NONE',  ( 137.1636751345948255, 0.000000000000000000, 5.500000000000005329 ) ) ;
#15268 = CARTESIAN_POINT ( 'NONE',  ( 5.412658773652739619, 3.124999999999988898, -72.68301270189225249 ) ) ;
#15269 = CARTESIAN_POINT ( 'NONE',  ( 5.196152422706629359, -2.999999999999988898, -172.7113248654052029 ) ) ;
#15270 = VECTOR ( 'NONE', #11882, 1000.000000000000000 ) ;
#15271 = CARTESIAN_POINT ( 'NONE',  ( 150.6413997308104342, 2.071067811865468400, -4.999999999999989342 ) ) ;
#15272 = CARTESIAN_POINT ( 'NONE',  ( 6.000000000000000888, -3.330669073875464691E-16, -7.560779664488942560E-35 ) ) ;
#15273 = CARTESIAN_POINT ( 'NONE',  ( 0.000000000000000000, 0.000000000000000000, 0.000000000000000000 ) ) ;
#15274 = CARTESIAN_POINT ( 'NONE',  ( 6.000000000000014211, -1.607695154586730180, -152.2306624327025588 ) ) ;
#15275 = CARTESIAN_POINT ( 'NONE',  ( 109.7886751345948255, -2.000000000000001776, 0.000000000000000000 ) ) ;
#15276 = ADVANCED_FACE ( 'NONE', ( #11585 ), #30390, .F. ) ;
#15277 = CARTESIAN_POINT ( 'NONE',  ( -2.775557561562891351E-14, -5.500000000000115463, -132.7500000000000284 ) ) ;
#15278 = CARTESIAN_POINT ( 'NONE',  ( 10.03867513459497118, 1.110223024625156540E-13, -2.500000000000113243 ) ) ;
#15279 = CARTESIAN_POINT ( 'NONE',  ( 0.000000000000000000, 0.000000000000000000, 0.000000000000000000 ) ) ;
#15280 = ORIENTED_EDGE ( 'NONE', *, *, #6999, .T. ) ;
#15281 = AXIS2_PLACEMENT_3D ( 'NONE', #20817, #14384, #16385 ) ;
#15282 = CARTESIAN_POINT ( 'NONE',  ( 6.350852961086080661, -9.614813431917819062E-14, -61.87500000000000711 ) ) ;
#15283 = CARTESIAN_POINT ( 'NONE',  ( 4.763139720814407951, -2.749999999999988454, -54.49999999999999289 ) ) ;
#15284 = AXIS2_PLACEMENT_3D ( 'NONE', #17019, #9787, #5295 ) ;
#15285 = CARTESIAN_POINT ( 'NONE',  ( 3.464101615137757051, -5.999999999999979572, -174.3363248654051461 ) ) ;
#15286 = VERTEX_POINT ( 'NONE', #16052 ) ;
#15287 = CIRCLE ( 'NONE', #2023, 1.000000000000000888 ) ;
#15288 = CARTESIAN_POINT ( 'NONE',  ( 148.9687500000000284, -2.485281374238585972, 6.000000000000005329 ) ) ;
#15289 = CARTESIAN_POINT ( 'NONE',  ( 141.0000000000000284, -54.99999999999989342, 5.000000000000004441 ) ) ;
#15290 = CARTESIAN_POINT ( 'NONE',  ( 14.75000000000009592, 2.220446049250313081E-13, -2.000000000000057288 ) ) ;
#15291 = AXIS2_PLACEMENT_3D ( 'NONE', #23364, #19199, #23799 ) ;
#15292 = CARTESIAN_POINT ( 'NONE',  ( -5.999999999999963585, 1.780251999655701777E-13, -89.33632486540523132 ) ) ;
#15293 = CARTESIAN_POINT ( 'NONE',  ( 110.9372167782374277, -0.7662911109077686911, 1.849990392679591977 ) ) ;
#15294 = VERTEX_POINT ( 'NONE', #16500 ) ;
#15295 = CARTESIAN_POINT ( 'NONE',  ( 144.7500000000000568, -6.000000000000005329, 0.000000000000000000 ) ) ;
#15296 = CARTESIAN_POINT ( 'NONE',  ( 161.2890952447136499, -5.450977163394726155, 1.974987045907475869 ) ) ;
#15297 = STYLED_ITEM ( 'NONE', ( #27055 ), #23960 ) ;
#15298 = ORIENTED_EDGE ( 'NONE', *, *, #8288, .F. ) ;
#15299 =( BOUNDED_CURVE ( )  B_SPLINE_CURVE ( 2, ( #16799, #21081, #16938, #11736, #23831, #9854, #25827, #28559, #23976 ),
 .UNSPECIFIED., .F., .F. ) 
 B_SPLINE_CURVE_WITH_KNOTS ( ( 3, 2, 2, 2, 3 ),
 ( 0.3805555555555555358, 0.3814814814814814770, 0.3833333333333333592, 0.3851851851851851860, 0.3861111111111111271 ),
 .UNSPECIFIED. ) 
 CURVE ( )  GEOMETRIC_REPRESENTATION_ITEM ( )  RATIONAL_B_SPLINE_CURVE ( ( 0.9330127018922194093, 0.9330127018922174109, 1.000000000000000000, 0.8660254037844388186, 1.000000000000000000, 0.8660254037844388186, 1.000000000000000000, 0.9330127018922174109, 0.9330127018922194093 ) ) 
 REPRESENTATION_ITEM ( '' )  );
#15300 = CARTESIAN_POINT ( 'NONE',  ( 3.175426480543072749, -5.500000000000105693, -146.1250000000000000 ) ) ;
#15301 = CARTESIAN_POINT ( 'NONE',  ( -7.216878364870328078, 0.000000000000000000, -48.69198729810783277 ) ) ;
#15302 = CARTESIAN_POINT ( 'NONE',  ( 17.12500000000005684, 1.414213562373090038, 1.414213562373201061 ) ) ;
#15303 = ORIENTED_EDGE ( 'NONE', *, *, #27396, .F. ) ;
#15304 = CARTESIAN_POINT ( 'NONE',  ( 3.608439182435180470, -6.249999999999997335, -150.1919872981078186 ) ) ;
#15305 = EDGE_CURVE ( 'NONE', #7046, #14487, #24898, .T. ) ;
#15306 = CARTESIAN_POINT ( 'NONE',  ( 3.175426480543072749, 5.499999999999865885, -70.62500000000004263 ) ) ;
#15307 = AXIS2_PLACEMENT_3D ( 'NONE', #25312, #9207, #18600 ) ;
#15308 = CARTESIAN_POINT ( 'NONE',  ( 15.25000000000001421, 1.873492889145067508, -1.873492889144956486 ) ) ;
#15309 = CARTESIAN_POINT ( 'NONE',  ( -3.608439182435115633, 6.249999999999965361, -93.30801270189219565 ) ) ;
#15310 = CARTESIAN_POINT ( 'NONE',  ( 0.000000000000000000, 5.499999999999991118, -153.0000000000000284 ) ) ;
#15311 = AXIS2_PLACEMENT_3D ( 'NONE', #27660, #1568, #20631 ) ;
#15312 = CARTESIAN_POINT ( 'NONE',  ( -3.199609099280245506, -10.52573284576702406, -30.07939160056616146 ) ) ;
#15313 = CARTESIAN_POINT ( 'NONE',  ( 116.0000000000000142, 0.000000000000000000, 0.000000000000000000 ) ) ;
#15314 = DIRECTION ( 'NONE',  ( -1.000000000000000000, -1.665334536937731113E-16, 1.526556658859586792E-16 ) ) ;
#15315 = CARTESIAN_POINT ( 'NONE',  ( 110.7886751345946834, -1.999999999999946265, 0.000000000000000000 ) ) ;
#15316 = EDGE_CURVE ( 'NONE', #16412, #17631, #24722, .T. ) ;
#15317 = EDGE_CURVE ( 'NONE', #9511, #24851, #4621, .T. ) ;
#15318 = CARTESIAN_POINT ( 'NONE',  ( -4.763139720814407951, -2.750000000000016431, -157.0000000000000284 ) ) ;
#15319 = CARTESIAN_POINT ( 'NONE',  ( 124.9999999999999432, -70.00000000000000000, -7.500000000000007105 ) ) ;
#15320 = AXIS2_PLACEMENT_3D ( 'NONE', #20600, #13880, #8927 ) ;
#15321 = CARTESIAN_POINT ( 'NONE',  ( 3.175426480543072749, -5.500000000000105693, -143.1250000000000000 ) ) ;
#15322 = CARTESIAN_POINT ( 'NONE',  ( -4.884531539219052476, 3.330387827114730914, -180.0000000000000284 ) ) ;
#15323 = CARTESIAN_POINT ( 'NONE',  ( 137.3511751345948255, -3.889087296526011706, 3.889087296526011706 ) ) ;
#15324 = CIRCLE ( 'NONE', #23162, 4.000000000000010658 ) ;
#15325 = UNCERTAINTY_MEASURE_WITH_UNIT (LENGTH_MEASURE( 1.000000000000000082E-05 ), #20636, 'distance_accuracy_value', 'NONE');
#15326 = CARTESIAN_POINT ( 'NONE',  ( 0.000000000000000000, 5.499999999999991118, -84.00000000000001421 ) ) ;
#15327 = FACE_OUTER_BOUND ( 'NONE', #2715, .T. ) ;
#15328 = CARTESIAN_POINT ( 'NONE',  ( 3.175426480543072749, -5.500000000000105693, -80.12500000000002842 ) ) ;
#15329 = CARTESIAN_POINT ( 'NONE',  ( 135.7425748654052029, -2.278174593052352925, -5.499999999999671374 ) ) ;
#15330 = VECTOR ( 'NONE', #24092, 1000.000000000000000 ) ;
#15331 = CARTESIAN_POINT ( 'NONE',  ( 3.464101615137852974, 5.999999999999884537, -164.8363248654052029 ) ) ;
#15332 = CARTESIAN_POINT ( 'NONE',  ( 13.99999999999999822, 0.000000000000000000, 0.000000000000000000 ) ) ;
#15333 = FACE_OUTER_BOUND ( 'NONE', #5651, .T. ) ;
#15334 = CARTESIAN_POINT ( 'NONE',  ( 6.000000000000001776, 5.345404176511898156E-15, -179.1636751345948539 ) ) ;
#15335 = CIRCLE ( 'NONE', #7934, 2.000000000000003109 ) ;
#15336 = CARTESIAN_POINT ( 'NONE',  ( -3.464101615137725076, 5.999999999999979572, -134.5863248654051745 ) ) ;
#15337 = CARTESIAN_POINT ( 'NONE',  ( 5.196152422706629359, 3.000000000000002665, -174.5386751345948539 ) ) ;
#15338 = VERTEX_POINT ( 'NONE', #9399 ) ;
#15339 = DIRECTION ( 'NONE',  ( 0.000000000000000000, 0.000000000000000000, 1.000000000000000000 ) ) ;
#15340 = CARTESIAN_POINT ( 'NONE',  ( 1.110223024625164183E-16, -2.000000000000012879, -1.776356839400262692E-15 ) ) ;
#15341 = DIRECTION ( 'NONE',  ( 1.000000000000000000, -5.551115123125774074E-17, -1.260129944081490338E-35 ) ) ;
#15342 = CARTESIAN_POINT ( 'NONE',  ( 117.1252832217621460, -5.551115123125782702E-14, -1.849990392679523588 ) ) ;
#15343 = CARTESIAN_POINT ( 'NONE',  ( 6.055081547227420202, 0.000000000000000000, 0.000000000000000000 ) ) ;
#15344 = VERTEX_POINT ( 'NONE', #21230 ) ;
#15345 =( BOUNDED_CURVE ( )  B_SPLINE_CURVE ( 2, ( #9826, #26677, #24534, #28533, #26240, #5193, #8093, #19357, #12760 ),
 .UNSPECIFIED., .F., .T. ) 
 B_SPLINE_CURVE_WITH_KNOTS ( ( 3, 2, 2, 2, 3 ),
 ( 0.5156250000000000000, 0.5234375000000000000, 0.5312500000000000000, 0.5390625000000000000, 0.5468750000000000000 ),
 .UNSPECIFIED. ) 
 CURVE ( )  GEOMETRIC_REPRESENTATION_ITEM ( )  RATIONAL_B_SPLINE_CURVE ( ( 1.000000000000000000, 0.9238795325112867385, 1.000000000000000000, 0.9238795325112867385, 1.000000000000000000, 0.9238795325112867385, 1.000000000000000000, 0.9238795325112867385, 1.000000000000000000 ) ) 
 REPRESENTATION_ITEM ( '' )  );
#15346 = AXIS2_PLACEMENT_3D ( 'NONE', #3049, #28249, #9987 ) ;
#15347 = VERTEX_POINT ( 'NONE', #12783 ) ;
#15348 = EDGE_CURVE ( 'NONE', #6076, #22729, #28706, .T. ) ;
#15349 = CARTESIAN_POINT ( 'NONE',  ( 4.763139720814407951, 2.750000000000002665, -94.75000000000000000 ) ) ;
#15350 = DIRECTION ( 'NONE',  ( -1.000000000000000000, -1.665334536937731113E-16, 1.526556658859586792E-16 ) ) ;
#15351 = CARTESIAN_POINT ( 'NONE',  ( 3.608439182435180470, 6.249999999999982236, -116.0580127018922383 ) ) ;
#15352 = DIRECTION ( 'NONE',  ( 0.000000000000000000, 0.8787878787878786735, 0.4772125984249585562 ) ) ;
#15353 = CARTESIAN_POINT ( 'NONE',  ( 104.5624999999997442, -2.499999999999934719, -1.035533905932689347 ) ) ;
#15354 = CARTESIAN_POINT ( 'NONE',  ( 3.608439182435180470, -6.249999999999997335, -49.05801270189224539 ) ) ;
#15355 = VERTEX_POINT ( 'NONE', #19670 ) ;
#15356 = EDGE_CURVE ( 'NONE', #19518, #18212, #12196, .T. ) ;
#15357 = CARTESIAN_POINT ( 'NONE',  ( 0.000000000000000000, -5.999999999999991118, -119.5386751345948255 ) ) ;
#15358 = LINE ( 'NONE', #24681, #26741 ) ;
#15359 = CARTESIAN_POINT ( 'NONE',  ( 155.4300748654052029, 2.278174593051818686, -5.500000000000204281 ) ) ;
#15360 = CARTESIAN_POINT ( 'NONE',  ( 4.763139720814407951, -2.749999999999988454, -170.0000000000000284 ) ) ;
#15361 = CARTESIAN_POINT ( 'NONE',  ( 105.9377832217620323, -1.849990392679441875, -0.7662911109074682647 ) ) ;
#15362 = CARTESIAN_POINT ( 'NONE',  ( -5.412658773652684552, -3.125000000000099920, -172.4330127018922667 ) ) ;
#15363 = FACE_OUTER_BOUND ( 'NONE', #9641, .T. ) ;
#15364 = CARTESIAN_POINT ( 'NONE',  ( 4.763139720814407951, 2.750000000000002665, -109.7500000000000142 ) ) ;
#15365 = FACE_OUTER_BOUND ( 'NONE', #1356, .T. ) ;
#15366 = CARTESIAN_POINT ( 'NONE',  ( -3.175426480542816510, 5.499999999999865885, -106.3750000000000284 ) ) ;
#15367 = CARTESIAN_POINT ( 'NONE',  ( 137.9136751345948539, 0.000000000000000000, -5.500000000000005329 ) ) ;
#15368 = FACE_OUTER_BOUND ( 'NONE', #25947, .T. ) ;
#15369 = CARTESIAN_POINT ( 'NONE',  ( 0.000000000000000000, 5.999999999999977796, -162.2886751345948824 ) ) ;
#15370 = CARTESIAN_POINT ( 'NONE',  ( 135.0000000000000284, -8.261054798780170572, 8.006597766721364806 ) ) ;
#15371 = ORIENTED_EDGE ( 'NONE', *, *, #15602, .F. ) ;
#15372 = CARTESIAN_POINT ( 'NONE',  ( 15.00000000000006928, -1.873492889144900975, 1.873492889144900975 ) ) ;
#15373 = DIRECTION ( 'NONE',  ( 0.000000000000000000, 0.000000000000000000, 1.000000000000000000 ) ) ;
#15374 = CARTESIAN_POINT ( 'NONE',  ( 112.0002832217622739, -1.308140751793557266, -1.308140751793640533 ) ) ;
#15375 = ORIENTED_EDGE ( 'NONE', *, *, #15927, .T. ) ;
#15376 = CARTESIAN_POINT ( 'NONE',  ( -7.216878364870328078, 0.000000000000000000, -80.19198729810784698 ) ) ;
#15377 = CARTESIAN_POINT ( 'NONE',  ( -5.999999999999963585, 1.780251999655701777E-13, -103.4136751345948255 ) ) ;
#15378 = ORIENTED_EDGE ( 'NONE', *, *, #19325, .F. ) ;
#15379 = DIRECTION ( 'NONE',  ( -7.147005652999508048E-36, 5.642372883946980038E-36, 1.000000000000000000 ) ) ;
#15380 = VECTOR ( 'NONE', #17241, 1000.000000000000000 ) ;
#15381 = ORIENTED_EDGE ( 'NONE', *, *, #907, .F. ) ;
#15382 = ORIENTED_EDGE ( 'NONE', *, *, #6846, .T. ) ;
#15383 = CARTESIAN_POINT ( 'NONE',  ( 159.0000000000000284, 6.000000000000005329, 0.000000000000000000 ) ) ;
#15384 = EDGE_CURVE ( 'NONE', #7800, #20811, #27936, .T. ) ;
#15385 = CARTESIAN_POINT ( 'NONE',  ( 3.175426480543072749, -5.500000000000105693, -131.1250000000000000 ) ) ;
#15386 = EDGE_CURVE ( 'NONE', #10812, #15497, #23832, .T. ) ;
#15387 = STYLED_ITEM ( 'NONE', ( #9627 ), #3017 ) ;
#15388 = CARTESIAN_POINT ( 'NONE',  ( -5.412658773652739619, 3.124999999999975131, -138.1830127018922667 ) ) ;
#15389 = ORIENTED_EDGE ( 'NONE', *, *, #22403, .T. ) ;
#15390 = CARTESIAN_POINT ( 'NONE',  ( 5.412658773652712085, -3.125000000000086153, -121.5669872981078328 ) ) ;
#15391 = SURFACE_SIDE_STYLE ('',( #8268 ) ) ;
#15392 = CARTESIAN_POINT ( 'NONE',  ( -4.763139720814407951, -2.750000000000016431, -169.0000000000000284 ) ) ;
#15393 = CARTESIAN_POINT ( 'NONE',  ( 6.000000000000000888, -1.859271017917181981E-14, -131.1636751345948539 ) ) ;
#15394 = CARTESIAN_POINT ( 'NONE',  ( 107.3511751345946266, 2.000000000000061728, 0.8284271247462955401 ) ) ;
#15395 = VERTEX_POINT ( 'NONE', #775 ) ;
#15396 = CARTESIAN_POINT ( 'NONE',  ( 16.43750000000008527, -1.999999999999851674, 0.8284271247461753029 ) ) ;
#15397 = CARTESIAN_POINT ( 'NONE',  ( 0.000000000000000000, 0.000000000000000000, 0.000000000000000000 ) ) ;
#15398 = CARTESIAN_POINT ( 'NONE',  ( 104.7401757384973280, 1.387249626875697306, 1.223929297688219897 ) ) ;
#15399 = CARTESIAN_POINT ( 'NONE',  ( 160.5164690628317317, -11.32153369091806461, -3.978831925134524106 ) ) ;
#15400 = CARTESIAN_POINT ( 'NONE',  ( 135.0000000000000284, 0.000000000000000000, -12.00000000000000178 ) ) ;
#15401 = CARTESIAN_POINT ( 'NONE',  ( 14.03867513459489125, 5.551115123125782702E-14, -2.500000000000057732 ) ) ;
#15402 = CARTESIAN_POINT ( 'NONE',  ( 114.0002832217621602, -1.308140751793585022, -1.308140751793640533 ) ) ;
#15403 = CARTESIAN_POINT ( 'NONE',  ( 5.412658773652739619, 3.124999999999988898, -64.31698729810780435 ) ) ;
#15404 = CARTESIAN_POINT ( 'NONE',  ( -3.608439182435115633, 6.249999999999965361, -53.44198729810779724 ) ) ;
#15405 = DIRECTION ( 'NONE',  ( -0.000000000000000000, -0.000000000000000000, -1.000000000000000000 ) ) ;
#15406 = CARTESIAN_POINT ( 'NONE',  ( 147.9449251345948539, -5.500000000000012434, 2.278174593052012309 ) ) ;
#15407 = DIRECTION ( 'NONE',  ( -1.000000000000000000, 3.469446951953694061E-16, -0.000000000000000000 ) ) ;
#15408 = CARTESIAN_POINT ( 'NONE',  ( -2.775557561562891351E-14, -5.500000000000115463, -126.7500000000000284 ) ) ;
#15409 = AXIS2_PLACEMENT_3D ( 'NONE', #21842, #28876, #789 ) ;
#15410 = ORIENTED_EDGE ( 'NONE', *, *, #8813, .F. ) ;
#15411 = CARTESIAN_POINT ( 'NONE',  ( 124.9999999999999432, -70.00000000000000000, 5.000000000000004441 ) ) ;
#15412 = CARTESIAN_POINT ( 'NONE',  ( 160.5863248654052597, 0.000000000000000000, 5.500000000000005329 ) ) ;
#15413 = CARTESIAN_POINT ( 'NONE',  ( 0.000000000000000000, -5.999999999999991118, -160.0386751345948539 ) ) ;
#15414 = CARTESIAN_POINT ( 'NONE',  ( 6.000000000000000888, -3.330669073875464691E-16, -7.560779664488942560E-35 ) ) ;
#15415 = CYLINDRICAL_SURFACE ( 'NONE', #250, 0.5000000000000004441 ) ;
#15416 = PRODUCT_DEFINITION_FORMATION_WITH_SPECIFIED_SOURCE ( 'ANY', '', #6978, .NOT_KNOWN. ) ;
#15417 = VERTEX_POINT ( 'NONE', #17383 ) ;
#15418 = CARTESIAN_POINT ( 'NONE',  ( 113.1247167782375556, -1.849990392679523588, 1.110223024625156540E-13 ) ) ;
#15419 = CARTESIAN_POINT ( 'NONE',  ( 5.412658773652739619, 3.124999999999988898, -118.3169872981078043 ) ) ;
#15420 = CARTESIAN_POINT ( 'NONE',  ( 5.196152422706629359, -2.999999999999988898, -54.21132486540525264 ) ) ;
#15421 = CARTESIAN_POINT ( 'NONE',  ( -3.464101615137725076, 5.999999999999979572, -91.08632486540520290 ) ) ;
#15422 = CARTESIAN_POINT ( 'NONE',  ( 116.1249999999999574, 1.767766952966265404, 1.767766952966431937 ) ) ;
#15423 = VERTEX_POINT ( 'NONE', #14495 ) ;
#15424 = DIRECTION ( 'NONE',  ( 0.000000000000000000, 0.000000000000000000, -1.000000000000000000 ) ) ;
#15425 = CARTESIAN_POINT ( 'NONE',  ( 142.6875000000000284, 4.242640687119269671, 4.242640687119298093 ) ) ;
#15426 = EDGE_CURVE ( 'NONE', #29417, #305, #26699, .T. ) ;
#15427 = CARTESIAN_POINT ( 'NONE',  ( 24.37500000000009237, 2.649519052838555933, 5.551115123125782702E-14 ) ) ;
#15428 = AXIS2_PLACEMENT_3D ( 'NONE', #12566, #14997, #24337 ) ;
#15429 = CARTESIAN_POINT ( 'NONE',  ( 135.8363248654052029, 0.000000000000000000, -5.500000000000005329 ) ) ;
#15430 = CARTESIAN_POINT ( 'NONE',  ( 4.763139720814407951, -2.749999999999988454, -50.00000000000004263 ) ) ;
#15431 = CARTESIAN_POINT ( 'NONE',  ( 159.1011751345948255, 3.889087296526011706, -3.889087296526011706 ) ) ;
#15432 = CARTESIAN_POINT ( 'NONE',  ( 6.000000000000000888, -1.859271017917181981E-14, -130.5863248654052313 ) ) ;
#15433 = CARTESIAN_POINT ( 'NONE',  ( 0.000000000000000000, 0.000000000000000000, 0.000000000000000000 ) ) ;
#15434 = CARTESIAN_POINT ( 'NONE',  ( 7.216878364870455975, -6.409875621278545621E-14, -77.30801270189223828 ) ) ;
#15435 = CARTESIAN_POINT ( 'NONE',  ( 0.000000000000000000, 0.000000000000000000, 0.000000000000000000 ) ) ;
#15436 = CARTESIAN_POINT ( 'NONE',  ( 148.5788997308104058, -4.999999999999989342, 2.071067811865468400 ) ) ;
#15437 = DIRECTION ( 'NONE',  ( 0.000000000000000000, 0.7999999999999996003, -0.6000000000000006439 ) ) ;
#15438 = CYLINDRICAL_SURFACE ( 'NONE', #20436, 5.500000000000000000 ) ;
#15439 = CARTESIAN_POINT ( 'NONE',  ( 135.3652387094614085, -8.709367079857635474, 8.045772721957300533 ) ) ;
#15440 =( BOUNDED_CURVE ( )  B_SPLINE_CURVE ( 2, ( #28293, #14378, #3387, #15264, #15106, #3541, #27045, #1402, #17568 ),
 .UNSPECIFIED., .F., .T. ) 
 B_SPLINE_CURVE_WITH_KNOTS ( ( 3, 2, 2, 2, 3 ),
 ( 0.7416666666666666963, 0.7425925925925925819, 0.7444444444444444642, 0.7462962962962963465, 0.7472222222222222321 ),
 .UNSPECIFIED. ) 
 CURVE ( )  GEOMETRIC_REPRESENTATION_ITEM ( )  RATIONAL_B_SPLINE_CURVE ( ( 0.9330127018922194093, 0.9330127018922234061, 1.000000000000000000, 0.8660254037844388186, 1.000000000000000000, 0.8660254037844388186, 1.000000000000000000, 0.9330127018922194093, 0.9330127018922194093 ) ) 
 REPRESENTATION_ITEM ( '' )  );
#15441 = CARTESIAN_POINT ( 'NONE',  ( 4.763139720814407951, 2.750000000000002665, -130.7500000000000284 ) ) ;
#15442 = CARTESIAN_POINT ( 'NONE',  ( 5.196152422706629359, -2.999999999999988898, -177.2113248654052597 ) ) ;
#15443 = CARTESIAN_POINT ( 'NONE',  ( 16.03867513459497474, 5.551115123125782702E-14, -2.500000000000057732 ) ) ;
#15444 = CARTESIAN_POINT ( 'NONE',  ( 5.999999999999949374, 1.607695154586804565, -178.5193375672974412 ) ) ;
#15445 = ORIENTED_EDGE ( 'NONE', *, *, #8921, .F. ) ;
#15446 = CARTESIAN_POINT ( 'NONE',  ( 3.175426480543072749, 5.499999999999865885, -63.12500000000001421 ) ) ;
#15447 = FACE_OUTER_BOUND ( 'NONE', #2130, .T. ) ;
#15448 = CARTESIAN_POINT ( 'NONE',  ( 3.175426480543072749, 5.499999999999865885, -60.12499999999999289 ) ) ;
#15449 = CARTESIAN_POINT ( 'NONE',  ( -5.999999999999963585, -1.487416814333745711E-14, -170.3363248654052313 ) ) ;
#15450 = VERTEX_POINT ( 'NONE', #5662 ) ;
#15451 = CARTESIAN_POINT ( 'NONE',  ( 110.1874999999997584, 1.035533905932779275, 2.500000000000205169 ) ) ;
#15452 = CARTESIAN_POINT ( 'NONE',  ( 148.4062500000000568, 6.000000000000005329, -2.485281374238556218 ) ) ;
#15453 = CARTESIAN_POINT ( 'NONE',  ( 13.87500000000011013, 1.414213562373312083, -1.414213562373145550 ) ) ;
#15454 = EDGE_CURVE ( 'NONE', #26763, #27165, #27913, .T. ) ;
#15455 = CARTESIAN_POINT ( 'NONE',  ( -5.196152422706573404, -3.000000000000002665, -49.28867513459483973 ) ) ;
#15456 = VERTEX_POINT ( 'NONE', #9856 ) ;
#15457 = CARTESIAN_POINT ( 'NONE',  ( 145.5000000000000284, 6.000000000000005329, 0.000000000000000000 ) ) ;
#15458 = DIRECTION ( 'NONE',  ( 0.000000000000000000, 0.000000000000000000, 1.000000000000000000 ) ) ;
#15459 = ORIENTED_EDGE ( 'NONE', *, *, #5647, .T. ) ;
#15460 = CARTESIAN_POINT ( 'NONE',  ( 3.175426480543072749, -5.500000000000105693, -144.6250000000000000 ) ) ;
#15461 = EDGE_CURVE ( 'NONE', #4790, #15666, #15529, .T. ) ;
#15462 = ORIENTED_EDGE ( 'NONE', *, *, #1470, .F. ) ;
#15463 = CARTESIAN_POINT ( 'NONE',  ( 7.216878364870455975, -6.409875621278545621E-14, -50.94198729810784698 ) ) ;
#15464 = CARTESIAN_POINT ( 'NONE',  ( 17.68750000000009592, -0.8284271247460553989, -1.999999999999971800 ) ) ;
#15465 = VERTEX_POINT ( 'NONE', #14774 ) ;
#15466 = CARTESIAN_POINT ( 'NONE',  ( 4.763139720814407951, 2.750000000000002665, -73.75000000000004263 ) ) ;
#15467 = CARTESIAN_POINT ( 'NONE',  ( 3.608439182435180470, 6.249999999999982236, -92.05801270189226670 ) ) ;
#15468 = CARTESIAN_POINT ( 'NONE',  ( -6.000000000000000888, 1.067854986875958443E-15, 7.560779664488942560E-35 ) ) ;
#15469 = DIRECTION ( 'NONE',  ( 1.000000000000000000, -0.000000000000000000, -0.000000000000000000 ) ) ;
#15470 = CARTESIAN_POINT ( 'NONE',  ( 135.6335788417890740, -8.691129701112460637, -8.179621397165890428 ) ) ;
#15471 = VECTOR ( 'NONE', #13475, 1000.000000000000000 ) ;
#15472 = CARTESIAN_POINT ( 'NONE',  ( 110.7261751345945413, -1.999999999999971800, 0.8284271247464157772 ) ) ;
#15473 = DIRECTION ( 'NONE',  ( 1.000000000000000000, 0.000000000000000000, 0.000000000000000000 ) ) ;
#15474 = CARTESIAN_POINT ( 'NONE',  ( 0.000000000000000000, 5.499999999999991118, -154.5000000000000284 ) ) ;
#15475 = CARTESIAN_POINT ( 'NONE',  ( 136.9613248654052313, -5.500000000000005329, 0.000000000000000000 ) ) ;
#15476 = CARTESIAN_POINT ( 'NONE',  ( 156.0863248654052597, 0.000000000000000000, 5.500000000000005329 ) ) ;
#15477 = CARTESIAN_POINT ( 'NONE',  ( 4.763139720814407951, -2.749999999999988454, -87.50000000000002842 ) ) ;
#15478 = CARTESIAN_POINT ( 'NONE',  ( 104.4997167782375413, 1.308140751793668288, -1.308140751793640533 ) ) ;
#15479 = SURFACE_STYLE_FILL_AREA ( #3143 ) ;
#15480 = CARTESIAN_POINT ( 'NONE',  ( 0.000000000000000000, 5.499999999999991118, -84.00000000000001421 ) ) ;
#15481 = CARTESIAN_POINT ( 'NONE',  ( -6.000000000000000888, 1.067854986875958443E-15, 7.560779664488942560E-35 ) ) ;
#15482 = CARTESIAN_POINT ( 'NONE',  ( 150.7648502691896510, 3.535533905932725318, 3.535533905932752852 ) ) ;
#15483 = CARTESIAN_POINT ( 'NONE',  ( 150.0074251345948539, 2.278174593052043395, -5.499999999999981348 ) ) ;
#15484 = CARTESIAN_POINT ( 'NONE',  ( 5.196152422706629359, -2.999999999999988898, -108.2113248654051887 ) ) ;
#15485 = CARTESIAN_POINT ( 'NONE',  ( -3.464101615137725076, 5.999999999999979572, -103.6636751345948255 ) ) ;
#15486 = CARTESIAN_POINT ( 'NONE',  ( 22.31250000000002842, -0.8284271247460552878, 2.000000000000031530 ) ) ;
#15487 = EDGE_CURVE ( 'NONE', #12929, #12702, #2444, .T. ) ;
#15488 = CARTESIAN_POINT ( 'NONE',  ( 3.464101615137757051, -5.999999999999979572, -165.3363248654051745 ) ) ;
#15489 =( BOUNDED_CURVE ( )  B_SPLINE_CURVE ( 2, ( #24375, #3466, #24080, #7937, #17046, #26522, #3319, #12901, #22086 ),
 .UNSPECIFIED., .F., .F. ) 
 B_SPLINE_CURVE_WITH_KNOTS ( ( 3, 2, 2, 2, 3 ),
 ( 0.4750000000000000333, 0.4759259259259259189, 0.4777777777777778012, 0.4796296296296296280, 0.4805555555555555136 ),
 .UNSPECIFIED. ) 
 CURVE ( )  GEOMETRIC_REPRESENTATION_ITEM ( )  RATIONAL_B_SPLINE_CURVE ( ( 0.9330127018922194093, 0.9330127018922214077, 1.000000000000000000, 0.8660254037844388186, 1.000000000000000000, 0.8660254037844388186, 1.000000000000000000, 0.9330127018922214077, 0.9330127018922194093 ) ) 
 REPRESENTATION_ITEM ( '' )  );
#15490 = CARTESIAN_POINT ( 'NONE',  ( -6.000000000000000888, 1.067854986875958443E-15, 7.560779664488942560E-35 ) ) ;
#15491 = VERTEX_POINT ( 'NONE', #10007 ) ;
#15492 = CARTESIAN_POINT ( 'NONE',  ( -10.00000000000000178, -19.99999999999998934, -4.000000000000003553 ) ) ;
#15493 = FACE_OUTER_BOUND ( 'NONE', #6736, .T. ) ;
#15494 = CARTESIAN_POINT ( 'NONE',  ( 145.6011751345948539, 3.889087296526011706, -3.889087296526011706 ) ) ;
#15495 = CARTESIAN_POINT ( 'NONE',  ( 117.4377832217621602, 1.849990392679562001, 0.7662911109079489913 ) ) ;
#15496 = CARTESIAN_POINT ( 'NONE',  ( 3.464101615137757051, -5.999999999999979572, -115.8363248654052171 ) ) ;
#15497 = VERTEX_POINT ( 'NONE', #16939 ) ;
#15498 = EDGE_CURVE ( 'NONE', #11567, #12257, #27042, .T. ) ;
#15499 = VERTEX_POINT ( 'NONE', #28560 ) ;
#15500 = CARTESIAN_POINT ( 'NONE',  ( 3.175426480543072749, 5.499999999999865885, -94.62500000000002842 ) ) ;
#15501 = CARTESIAN_POINT ( 'NONE',  ( -3.464101615137757051, -5.999999999999979572, -89.66367513459485394 ) ) ;
#15502 = CARTESIAN_POINT ( 'NONE',  ( -3.608439182435115633, 6.249999999999965361, -118.8080127018922525 ) ) ;
#15503 = ORIENTED_EDGE ( 'NONE', *, *, #11015, .T. ) ;
#15504 = CARTESIAN_POINT ( 'NONE',  ( 6.000000000000000888, 1.743066579297358182E-13, -92.16367513459482552 ) ) ;
#15505 = CARTESIAN_POINT ( 'NONE',  ( 3.464101615137852974, 5.999999999999884537, -63.41367513459483973 ) ) ;
#15506 = AXIS2_PLACEMENT_3D ( 'NONE', #23444, #25727, #25407 ) ;
#15507 = CARTESIAN_POINT ( 'NONE',  ( 2.775557561562891351E-14, 6.250000000000033751, -49.93301270189220986 ) ) ;
#15508 = ORIENTED_EDGE ( 'NONE', *, *, #17486, .T. ) ;
#15509 = CARTESIAN_POINT ( 'NONE',  ( 0.000000000000000000, 0.000000000000000000, 0.000000000000000000 ) ) ;
#15510 = CARTESIAN_POINT ( 'NONE',  ( -3.464101615137757051, -5.999999999999979572, -167.0863248654051461 ) ) ;
#15511 = FACE_OUTER_BOUND ( 'NONE', #17822, .T. ) ;
#15512 = CARTESIAN_POINT ( 'NONE',  ( 4.763139720814407951, -2.749999999999988454, -171.5000000000000000 ) ) ;
#15513 = CARTESIAN_POINT ( 'NONE',  ( 114.7499999999999147, -5.551115123125782702E-14, -2.499999999999946709 ) ) ;
#15514 = CARTESIAN_POINT ( 'NONE',  ( -5.412658773652684552, -3.125000000000099920, -163.4330127018922667 ) ) ;
#15515 = CARTESIAN_POINT ( 'NONE',  ( -0.5631067912581170232, -9.873786417483767508, 4.496381089953940702 ) ) ;
#15516 = CARTESIAN_POINT ( 'NONE',  ( 23.83632486540529527, 1.767766952966487448, 1.767766952966320915 ) ) ;
#15517 = CARTESIAN_POINT ( 'NONE',  ( -3.175426480542816510, -5.500000000000057732, -108.8750000000000426 ) ) ;
#15518 = TOROIDAL_SURFACE ( 'NONE', #27236, 1.000000000000000000, 0.5000000000000000000 ) ;
#15519 = TOROIDAL_SURFACE ( 'NONE', #7619, 10.49999999999999822, 0.5000000000000000000 ) ;
#15520 = CARTESIAN_POINT ( 'NONE',  ( -5.999999999999956479, -1.607695154586745057, -87.76933756729744118 ) ) ;
#15521 = CARTESIAN_POINT ( 'NONE',  ( 141.3824251345948539, 5.500000000000012434, 2.278174593052012309 ) ) ;
#15522 = CARTESIAN_POINT ( 'NONE',  ( 2.676951800742168933E-14, -11.00000000000000000, -19.00000000000002132 ) ) ;
#15523 = ORIENTED_EDGE ( 'NONE', *, *, #16785, .F. ) ;
#15524 = CARTESIAN_POINT ( 'NONE',  ( 14.93749999999998401, -1.097466725451499370, 2.649519052838298805 ) ) ;
#15525 = CARTESIAN_POINT ( 'NONE',  ( 117.9374999999998721, 2.500000000000114575, -1.035533905932448873 ) ) ;
#15526 = EDGE_CURVE ( 'NONE', #476, #3609, #26415, .T. ) ;
#15527 = CARTESIAN_POINT ( 'NONE',  ( 109.1252832217621744, -1.665334536937734811E-13, -1.849990392679523588 ) ) ;
#15528 = CARTESIAN_POINT ( 'NONE',  ( -3.464101615137757051, -5.999999999999979572, -134.0863248654051745 ) ) ;
#15529 =( BOUNDED_CURVE ( )  B_SPLINE_CURVE ( 2, ( #7392, #24258, #21537, #21686, #14920, #7677, #3066, #12491, #26120 ),
 .UNSPECIFIED., .F., .F. ) 
 B_SPLINE_CURVE_WITH_KNOTS ( ( 3, 2, 2, 2, 3 ),
 ( 0.3361111111111110272, 0.3370370370370370239, 0.3388888888888889062, 0.3407407407407407884, 0.3416666666666666741 ),
 .UNSPECIFIED. ) 
 CURVE ( )  GEOMETRIC_REPRESENTATION_ITEM ( )  RATIONAL_B_SPLINE_CURVE ( ( 0.9330127018922194093, 0.9330127018922154125, 1.000000000000000000, 0.8660254037844388186, 1.000000000000000000, 0.8660254037844388186, 1.000000000000000000, 0.9330127018922194093, 0.9330127018922194093 ) ) 
 REPRESENTATION_ITEM ( '' )  );
#15530 = ORIENTED_EDGE ( 'NONE', *, *, #25761, .F. ) ;
#15531 = CARTESIAN_POINT ( 'NONE',  ( 4.763139720814407951, 2.750000000000002665, -157.7500000000000568 ) ) ;
#15532 = CARTESIAN_POINT ( 'NONE',  ( 139.4925748654052313, 2.278174593052074925, 5.499999999999950262 ) ) ;
#15533 = AXIS2_PLACEMENT_3D ( 'NONE', #7301, #28469, #518 ) ;
#15534 = CARTESIAN_POINT ( 'NONE',  ( 5.412658773652712085, -3.125000000000086153, -79.56698729810784698 ) ) ;
#15535 = CARTESIAN_POINT ( 'NONE',  ( 156.8363248654052313, 0.000000000000000000, -5.500000000000005329 ) ) ;
#15536 = ORIENTED_EDGE ( 'NONE', *, *, #6053, .T. ) ;
#15537 = EDGE_CURVE ( 'NONE', #28127, #8469, #13372, .T. ) ;
#15538 = CARTESIAN_POINT ( 'NONE',  ( 115.8988248654050750, 0.8284271247463257382, 2.000000000000271783 ) ) ;
#15539 = ORIENTED_EDGE ( 'NONE', *, *, #16603, .T. ) ;
#15540 = CARTESIAN_POINT ( 'NONE',  ( 154.5937500000000284, 6.000000000000005329, 2.485281374238585972 ) ) ;
#15541 = CARTESIAN_POINT ( 'NONE',  ( 3.175426480543072749, -5.500000000000105693, -120.6250000000000284 ) ) ;
#15542 = CARTESIAN_POINT ( 'NONE',  ( 5.412658773652739619, 3.124999999999988898, -137.1830127018922667 ) ) ;
#15543 = ORIENTED_EDGE ( 'NONE', *, *, #9187, .F. ) ;
#15544 = CARTESIAN_POINT ( 'NONE',  ( 151.0386751345948539, -5.500000000000005329, 0.000000000000000000 ) ) ;
#15545 = CARTESIAN_POINT ( 'NONE',  ( -3.608439182435115633, 6.249999999999965361, -125.4419872981078043 ) ) ;
#15546 = CARTESIAN_POINT ( 'NONE',  ( 3.175426480543072749, 5.499999999999865885, -171.1250000000000000 ) ) ;
#15547 = MECHANICAL_DESIGN_GEOMETRIC_PRESENTATION_REPRESENTATION (  '', ( #9128 ), #12599 ) ;
#15548 = DIRECTION ( 'NONE',  ( 0.000000000000000000, 0.000000000000000000, -1.000000000000000000 ) ) ;
#15549 = CARTESIAN_POINT ( 'NONE',  ( 6.000000000000000888, 1.743066579297358182E-13, -48.08632486540521711 ) ) ;
#15550 = ORIENTED_EDGE ( 'NONE', *, *, #30265, .T. ) ;
#15551 = CARTESIAN_POINT ( 'NONE',  ( 12.50000000000012257, -1.999999999999835243, 0.000000000000000000 ) ) ;
#15552 = DIRECTION ( 'NONE',  ( -1.000000000000000000, -0.000000000000000000, -0.000000000000000000 ) ) ;
#15553 = CARTESIAN_POINT ( 'NONE',  ( 5.999999999999999112, 2.951592740943527306E-14, -148.5863248654052313 ) ) ;
#15554 = CARTESIAN_POINT ( 'NONE',  ( 159.5629673084600597, -11.38634829877173438, -3.839848799536992097 ) ) ;
#15555 = DIRECTION ( 'NONE',  ( -7.147005652999508048E-36, 5.642372883946980038E-36, 1.000000000000000000 ) ) ;
#15556 = CARTESIAN_POINT ( 'NONE',  ( 0.1053031288715573777, -15.23283975038563298, -8.619984219653423096 ) ) ;
#15557 = CARTESIAN_POINT ( 'NONE',  ( 110.8127832217621318, -1.849990392679381701, 0.7662911109078888172 ) ) ;
#15558 = CARTESIAN_POINT ( 'NONE',  ( -5.412658773652739619, 3.124999999999975131, -71.31698729810781856 ) ) ;
#15559 = TOROIDAL_SURFACE ( 'NONE', #15021, 12.50000000000000178, 0.5000000000000000000 ) ;
#15560 = CARTESIAN_POINT ( 'NONE',  ( 5.412658773652739619, 3.124999999999988898, -52.31698729810785409 ) ) ;
#15561 = DIRECTION ( 'NONE',  ( -7.147005652999508048E-36, 5.642372883946980038E-36, 1.000000000000000000 ) ) ;
#15562 = CARTESIAN_POINT ( 'NONE',  ( 140.0000000000000284, -8.500000000000007105, -7.500000000000007105 ) ) ;
#15563 = DIRECTION ( 'NONE',  ( -0.000000000000000000, -0.000000000000000000, -1.000000000000000000 ) ) ;
#15564 = CARTESIAN_POINT ( 'NONE',  ( -3.175426480542816510, 5.499999999999865885, -133.3750000000000284 ) ) ;
#15565 = CARTESIAN_POINT ( 'NONE',  ( 5.196152422706629359, 3.000000000000002665, -50.96132486540522422 ) ) ;
#15566 = CARTESIAN_POINT ( 'NONE',  ( 104.7401757384973138, -0.5936465683476789268, -1.756393372907816719 ) ) ;
#15567 = ORIENTED_EDGE ( 'NONE', *, *, #22466, .F. ) ;
#15568 = ADVANCED_FACE ( 'NONE', ( #3662 ), #17168, .T. ) ;
#15569 = CYLINDRICAL_SURFACE ( 'NONE', #2794, 6.000000000000000888 ) ;
#15570 = CARTESIAN_POINT ( 'NONE',  ( 16.52382486540528106, 1.035533905932929599, -2.500000000000024425 ) ) ;
#15571 = EDGE_CURVE ( 'NONE', #12687, #28026, #5353, .T. ) ;
#15572 = CARTESIAN_POINT ( 'NONE',  ( 138.7648502691896795, 3.535533905932725318, 3.535533905932752852 ) ) ;
#15573 = ORIENTED_EDGE ( 'NONE', *, *, #17980, .T. ) ;
#15574 = AXIS2_PLACEMENT_3D ( 'NONE', #20618, #29967, #2177 ) ;
#15575 = CARTESIAN_POINT ( 'NONE',  ( 113.6872167782373850, 1.849990392679532247, 0.7662911109078888172 ) ) ;
#15576 = SURFACE_STYLE_FILL_AREA ( #17558 ) ;
#15577 = CARTESIAN_POINT ( 'NONE',  ( 114.1636751345947829, 1.414213562373145550, -1.414213562372812483 ) ) ;
#15578 = CARTESIAN_POINT ( 'NONE',  ( 7.216878364870455975, -6.409875621278545621E-14, -115.4419872981078328 ) ) ;
#15579 = CARTESIAN_POINT ( 'NONE',  ( 6.000000000000000888, -1.859271017917181981E-14, -173.1636751345948539 ) ) ;
#15580 = CARTESIAN_POINT ( 'NONE',  ( 10.00000000000014744, 1.428066816532635119, 1.737247053690839760 ) ) ;
#15581 = VERTEX_POINT ( 'NONE', #15398 ) ;
#15582 = CARTESIAN_POINT ( 'NONE',  ( 138.4761751345948539, 3.889087296526011706, 3.889087296526011706 ) ) ;
#15583 = CARTESIAN_POINT ( 'NONE',  ( 141.4687500000000568, -2.485281374238585972, 6.000000000000005329 ) ) ;
#15584 = ORIENTED_EDGE ( 'NONE', *, *, #5819, .T. ) ;
#15585 = CARTESIAN_POINT ( 'NONE',  ( 161.0000000000000284, 0.000000000000000000, 0.000000000000000000 ) ) ;
#15586 = CARTESIAN_POINT ( 'NONE',  ( -3.175426480542816510, -5.500000000000057732, -53.37500000000002842 ) ) ;
#15587 = PRODUCT_DEFINITION_SHAPE ( 'NONE', 'NONE',  #6719 ) ;
#15588 = CARTESIAN_POINT ( 'NONE',  ( -3.464101615137725076, 5.999999999999979572, -120.1636751345947829 ) ) ;
#15589 = FACE_OUTER_BOUND ( 'NONE', #26655, .T. ) ;
#15590 = CARTESIAN_POINT ( 'NONE',  ( -5.412658773652684552, -3.125000000000099920, -65.93301270189222407 ) ) ;
#15591 = DIRECTION ( 'NONE',  ( -7.147005652999508048E-36, 5.642372883946980038E-36, 1.000000000000000000 ) ) ;
#15592 = CARTESIAN_POINT ( 'NONE',  ( 147.5476497308104058, 0.000000000000000000, -5.000000000000004441 ) ) ;
#15593 = DIRECTION ( 'NONE',  ( 1.000000000000000000, -5.551115123125773458E-17, -1.260129944081490338E-35 ) ) ;
#15594 = DIRECTION ( 'NONE',  ( -1.000000000000000000, -1.665334536937736783E-16, -2.220446049250315546E-16 ) ) ;
#15595 = DIRECTION ( 'NONE',  ( 0.000000000000000000, -0.000000000000000000, 1.000000000000000000 ) ) ;
#15596 = FILL_AREA_STYLE ('',( #10661 ) ) ;
#15597 = CARTESIAN_POINT ( 'NONE',  ( -6.350852961085760029, -1.281975124255709124E-13, -133.1250000000000284 ) ) ;
#15598 = MECHANICAL_DESIGN_GEOMETRIC_PRESENTATION_REPRESENTATION (  '', ( #10736 ), #9696 ) ;
#15599 = CARTESIAN_POINT ( 'NONE',  ( 5.412658773652712085, -3.125000000000086153, -149.4330127018922383 ) ) ;
#15600 = DIRECTION ( 'NONE',  ( 1.000000000000000000, -5.551115123125773458E-17, -1.260129944081490338E-35 ) ) ;
#15601 = ORIENTED_EDGE ( 'NONE', *, *, #13847, .T. ) ;
#15602 = EDGE_CURVE ( 'NONE', #23117, #2429, #1521, .T. ) ;
#15603 = CARTESIAN_POINT ( 'NONE',  ( -4.763139720814407951, -2.750000000000016431, -62.50000000000000000 ) ) ;
#15604 = CARTESIAN_POINT ( 'NONE',  ( 5.196152422706629359, 3.000000000000002665, -172.4613248654052313 ) ) ;
#15605 = EDGE_CURVE ( 'NONE', #14656, #23965, #18144, .T. ) ;
#15606 = CARTESIAN_POINT ( 'NONE',  ( -5.999999999999963585, 1.780251999655701777E-13, -56.91367513459483973 ) ) ;
#15607 = EDGE_LOOP ( 'NONE', ( #5610, #419, #11053, #6111 ) ) ;
#15608 = CARTESIAN_POINT ( 'NONE',  ( 109.6249999999999858, -1.767766952966376426, -1.767766952966320915 ) ) ;
#15609 = CARTESIAN_POINT ( 'NONE',  ( 148.7812500000000568, 2.485281374238585972, 6.000000000000005329 ) ) ;
#15610 = CARTESIAN_POINT ( 'NONE',  ( 140.0000000000000284, -54.99999999999990763, 7.500000000000007105 ) ) ;
#15611 = CARTESIAN_POINT ( 'NONE',  ( 13.62500000000016520, -1.414213562372923505, -1.414213562373145550 ) ) ;
#15612 = CYLINDRICAL_SURFACE ( 'NONE', #5242, 6.000000000000000888 ) ;
#15613 = VECTOR ( 'NONE', #5568, 1000.000000000000000 ) ;
#15614 = ORIENTED_EDGE ( 'NONE', *, *, #21949, .T. ) ;
#15615 = CARTESIAN_POINT ( 'NONE',  ( 135.8437500000000284, -6.000000000000005329, -2.485281374238555774 ) ) ;
#15616 = CARTESIAN_POINT ( 'NONE',  ( -4.999999999999990230, -55.00000000000002132, -7.500000000000007105 ) ) ;
#15617 = VERTEX_POINT ( 'NONE', #3513 ) ;
#15618 =( BOUNDED_CURVE ( )  B_SPLINE_CURVE ( 2, ( #15760, #27825, #18354, #27670, #24774, #29835, #15604, #13149, #29679 ),
 .UNSPECIFIED., .F., .T. ) 
 B_SPLINE_CURVE_WITH_KNOTS ( ( 3, 2, 2, 2, 3 ),
 ( 0.9305555555555555802, 0.9314814814814814659, 0.9333333333333333481, 0.9351851851851852304, 0.9361111111111111160 ),
 .UNSPECIFIED. ) 
 CURVE ( )  GEOMETRIC_REPRESENTATION_ITEM ( )  RATIONAL_B_SPLINE_CURVE ( ( 0.9330127018922194093, 0.9330127018922234061, 1.000000000000000000, 0.8660254037844388186, 1.000000000000000000, 0.8660254037844388186, 1.000000000000000000, 0.9330127018922194093, 0.9330127018922194093 ) ) 
 REPRESENTATION_ITEM ( '' )  );
#15619 = CARTESIAN_POINT ( 'NONE',  ( 3.175426480543072749, 5.499999999999865885, -147.1250000000000284 ) ) ;
#15620 = ORIENTED_EDGE ( 'NONE', *, *, #570, .F. ) ;
#15621 = CARTESIAN_POINT ( 'NONE',  ( 11.18750000000003730, 0.8284271247462955401, 2.000000000000031530 ) ) ;
#15622 = ORIENTED_EDGE ( 'NONE', *, *, #29154, .F. ) ;
#15623 = CARTESIAN_POINT ( 'NONE',  ( -6.350852961085760029, -1.281975124255709124E-13, -70.12500000000005684 ) ) ;
#15624 = CARTESIAN_POINT ( 'NONE',  ( 14.50000000000006750, 1.873492889145123019, 1.873492889144845464 ) ) ;
#15625 = CARTESIAN_POINT ( 'NONE',  ( 7.216878364870455975, -6.409875621278545621E-14, -95.30801270189220986 ) ) ;
#15626 =( BOUNDED_CURVE ( )  B_SPLINE_CURVE ( 2, ( #25086, #18369, #1900, #23119, #16083, #23423, #18519, #11771, #6811 ),
 .UNSPECIFIED., .F., .T. ) 
 B_SPLINE_CURVE_WITH_KNOTS ( ( 3, 2, 2, 2, 3 ),
 ( 0.1249999999999999861, 0.1259259259259259134, 0.1277777777777777679, 0.1296296296296296224, 0.1305555555555555636 ),
 .UNSPECIFIED. ) 
 CURVE ( )  GEOMETRIC_REPRESENTATION_ITEM ( )  RATIONAL_B_SPLINE_CURVE ( ( 0.9330127018922194093, 0.9330127018922189652, 1.000000000000000000, 0.8660254037844388186, 1.000000000000000000, 0.8660254037844388186, 1.000000000000000000, 0.9330127018922184101, 0.9330127018922194093 ) ) 
 REPRESENTATION_ITEM ( '' )  );
#15627 = CARTESIAN_POINT ( 'NONE',  ( -1.971541444415825683, -10.82814027403871471, -30.68027829220104863 ) ) ;
#15628 = CARTESIAN_POINT ( 'NONE',  ( 3.464101615137852974, 5.999999999999884537, -106.9136751345947971 ) ) ;
#15629 = CYLINDRICAL_SURFACE ( 'NONE', #12657, 1.000000000000000000 ) ;
#15630 = CARTESIAN_POINT ( 'NONE',  ( 135.8076776779767272, -8.774823127787460209, -8.164319474386353193 ) ) ;
#15631 = CARTESIAN_POINT ( 'NONE',  ( 3.175426480543072749, -5.500000000000105693, -153.6250000000000568 ) ) ;
#15632 = CARTESIAN_POINT ( 'NONE',  ( 17.52382486540523843, 1.035533905932869425, -2.499999999999904521 ) ) ;
#15633 = CARTESIAN_POINT ( 'NONE',  ( -5.999999999999963585, 1.780251999655701777E-13, -48.83632486540521711 ) ) ;
#15634 = CARTESIAN_POINT ( 'NONE',  ( -3.175426480542816066, 5.499999999999865885, -86.87500000000007105 ) ) ;
#15635 = FACE_OUTER_BOUND ( 'NONE', #7583, .T. ) ;
#15636 = LINE ( 'NONE', #24946, #5620 ) ;
#15637 = CARTESIAN_POINT ( 'NONE',  ( -2.775557561562891351E-14, -5.500000000000115463, -75.75000000000004263 ) ) ;
#15638 = ADVANCED_FACE ( 'NONE', ( #11234 ), #18001, .T. ) ;
#15639 = CARTESIAN_POINT ( 'NONE',  ( 152.3586002691896510, 2.071067811865468400, 4.999999999999989342 ) ) ;
#15640 = CARTESIAN_POINT ( 'NONE',  ( -5.999999999999971578, 1.607695154586715303, -164.4033121635129930 ) ) ;
#15641 = DIRECTION ( 'NONE',  ( -7.147005652999508048E-36, 5.642372883946980038E-36, 1.000000000000000000 ) ) ;
#15642 = MECHANICAL_DESIGN_GEOMETRIC_PRESENTATION_REPRESENTATION (  '', ( #392 ), #22474 ) ;
#15643 = CARTESIAN_POINT ( 'NONE',  ( 3.464101615137852974, 5.999999999999884537, -103.9136751345948255 ) ) ;
#15644 = CARTESIAN_POINT ( 'NONE',  ( 113.2113248654051034, -1.999999999999918510, 1.110223024625156540E-13 ) ) ;
#15645 = CARTESIAN_POINT ( 'NONE',  ( 119.8122167782374277, 0.7662911109078588412, 1.849990392679712103 ) ) ;
#15646 = CYLINDRICAL_SURFACE ( 'NONE', #12093, 6.000000000000000888 ) ;
#15647 = ORIENTED_EDGE ( 'NONE', *, *, #20639, .F. ) ;
#15648 = CARTESIAN_POINT ( 'NONE',  ( 156.0000000000000284, 6.000000000000005329, 0.000000000000000000 ) ) ;
#15649 = DIRECTION ( 'NONE',  ( 1.000000000000000000, -5.551115123125774690E-17, -1.260129944081490338E-35 ) ) ;
#15650 = CARTESIAN_POINT ( 'NONE',  ( -5.196152422706573404, -3.000000000000002665, -172.2886751345948255 ) ) ;
#15651 = PRESENTATION_LAYER_ASSIGNMENT (  '', '', ( #11728 ) ) ;
#15652 = CARTESIAN_POINT ( 'NONE',  ( 116.2502832217621886, 1.308140751793612777, -1.308140751793418488 ) ) ;
#15653 = DIRECTION ( 'NONE',  ( 1.000000000000000000, -5.551115123125773458E-17, -1.260129944081490338E-35 ) ) ;
#15654 = ORIENTED_EDGE ( 'NONE', *, *, #1550, .T. ) ;
#15655 = VERTEX_POINT ( 'NONE', #24870 ) ;
#15656 = CARTESIAN_POINT ( 'NONE',  ( -2.775557561562891351E-14, -5.500000000000115463, -99.75000000000000000 ) ) ;
#15657 = DIRECTION ( 'NONE',  ( 1.000000000000000000, -5.551115123125773458E-17, -1.260129944081490338E-35 ) ) ;
#15658 = CARTESIAN_POINT ( 'NONE',  ( -7.216878364870328078, 0.000000000000000000, -115.5580127018922383 ) ) ;
#15659 = ORIENTED_EDGE ( 'NONE', *, *, #25861, .T. ) ;
#15660 = CARTESIAN_POINT ( 'NONE',  ( 5.196152422706629359, 3.000000000000002665, -92.03867513459485394 ) ) ;
#15661 = SHAPE_REPRESENTATION ( 'Fixed Jaw', ( #18805 ), #19755 ) ;
#15662 = EDGE_CURVE ( 'NONE', #21925, #20404, #11406, .T. ) ;
#15663 = CARTESIAN_POINT ( 'NONE',  ( -3.464101615137757051, -5.999999999999979572, -143.6636751345948255 ) ) ;
#15664 = EDGE_CURVE ( 'NONE', #16115, #28288, #591, .T. ) ;
#15665 = CARTESIAN_POINT ( 'NONE',  ( 3.608439182435180470, 6.249999999999982236, -48.55801270189223828 ) ) ;
#15666 = VERTEX_POINT ( 'NONE', #10781 ) ;
#15667 = CARTESIAN_POINT ( 'NONE',  ( -5.999999999999963585, -1.487416814333745711E-14, -167.3363248654052029 ) ) ;
#15668 = CARTESIAN_POINT ( 'NONE',  ( 3.175426480543072749, -5.500000000000105693, -161.1250000000000284 ) ) ;
#15669 = CARTESIAN_POINT ( 'NONE',  ( 116.4374999999997726, -2.499999999999934719, 1.035533905932929599 ) ) ;
#15670 = CARTESIAN_POINT ( 'NONE',  ( 5.999999999999999112, 2.951592740943527306E-14, -157.5863248654052313 ) ) ;
#15671 = CARTESIAN_POINT ( 'NONE',  ( -4.763139720814407951, -2.750000000000016431, -106.0000000000000426 ) ) ;
#15672 = CARTESIAN_POINT ( 'NONE',  ( 13.47617513459483263, 1.035533905932869425, 2.499999999999844569 ) ) ;
#15673 = ADVANCED_FACE ( 'NONE', ( #15229 ), #22589, .F. ) ;
#15674 = CARTESIAN_POINT ( 'NONE',  ( -4.763139720814407951, 2.749999999999946709, -97.25000000000000000 ) ) ;
#15675 = ADVANCED_FACE ( 'NONE', ( #29473 ), #4126, .T. ) ;
#15676 = PRESENTATION_STYLE_ASSIGNMENT (( #15201 ) ) ;
#15677 = CARTESIAN_POINT ( 'NONE',  ( -15.49999999999999289, -25.00000000000007816, -7.500000000000007105 ) ) ;
#15678 = CARTESIAN_POINT ( 'NONE',  ( 5.196152422706629359, -2.999999999999988898, -84.21132486540521711 ) ) ;
#15679 = ORIENTED_EDGE ( 'NONE', *, *, #10185, .F. ) ;
#15680 = CARTESIAN_POINT ( 'NONE',  ( 16.00000000000012434, -1.873492889144845464, 1.873492889144845464 ) ) ;
#15681 = CARTESIAN_POINT ( 'NONE',  ( 115.4374999999997868, -2.499999999999934719, 1.035533905932929599 ) ) ;
#15682 = CARTESIAN_POINT ( 'NONE',  ( 109.7502832217623734, -1.308140751793612777, 1.308140751793640533 ) ) ;
#15683 = ORIENTED_EDGE ( 'NONE', *, *, #1925, .T. ) ;
#15684 = CARTESIAN_POINT ( 'NONE',  ( 109.0622167782374561, -1.849990392679501827, 0.7662911109077686911 ) ) ;
#15685 = CARTESIAN_POINT ( 'NONE',  ( 3.608439182435180470, -6.249999999999997335, -88.69198729810783277 ) ) ;
#15686 = CARTESIAN_POINT ( 'NONE',  ( -5.999999999999956479, -1.607695154586745057, -97.34668783648704959 ) ) ;
#15687 = ORIENTED_EDGE ( 'NONE', *, *, #21507, .F. ) ;
#15688 = CARTESIAN_POINT ( 'NONE',  ( -0.8024951133111937196, 10.97768020916284648, -30.95935331155643411 ) ) ;
#15689 = CARTESIAN_POINT ( 'NONE',  ( -4.763139720814407951, -2.750000000000016431, -151.0000000000000284 ) ) ;
#15690 = ORIENTED_EDGE ( 'NONE', *, *, #18609, .F. ) ;
#15691 = ORIENTED_EDGE ( 'NONE', *, *, #12241, .T. ) ;
#15692 = CARTESIAN_POINT ( 'NONE',  ( 158.0625000000000284, -4.242640687119298093, 4.242640687119298093 ) ) ;
#15693 = CARTESIAN_POINT ( 'NONE',  ( -3.175426480542816510, -5.500000000000057732, -120.8750000000000284 ) ) ;
#15694 = CARTESIAN_POINT ( 'NONE',  ( 3.608439182435180470, 6.249999999999982236, -140.0580127018922383 ) ) ;
#15695 = ORIENTED_EDGE ( 'NONE', *, *, #2646, .F. ) ;
#15696 = CARTESIAN_POINT ( 'NONE',  ( 6.000000000000000888, -3.330669073875464691E-16, -7.560779664488942560E-35 ) ) ;
#15697 = CARTESIAN_POINT ( 'NONE',  ( 3.608439182435180470, -6.249999999999997335, -121.6919872981077901 ) ) ;
#15698 = CARTESIAN_POINT ( 'NONE',  ( -7.216878364870328078, 0.000000000000000000, -174.6919872981077901 ) ) ;
#15699 = CARTESIAN_POINT ( 'NONE',  ( 0.000000000000000000, 5.499999999999991118, -175.5000000000000000 ) ) ;
#15700 = CARTESIAN_POINT ( 'NONE',  ( 159.1354668258956053, -11.07692307937646348, 4.615384609496523183 ) ) ;
#15701 = CARTESIAN_POINT ( 'NONE',  ( 20.46132486540533435, 1.110223024625156540E-13, -2.500000000000057732 ) ) ;
#15702 = EDGE_CURVE ( 'NONE', #5319, #24536, #17849, .T. ) ;
#15703 = ORIENTED_EDGE ( 'NONE', *, *, #17359, .T. ) ;
#15704 = CARTESIAN_POINT ( 'NONE',  ( 11.87500000000007994, 1.414213562373312083, -1.414213562373090038 ) ) ;
#15705 = CARTESIAN_POINT ( 'NONE',  ( 0.000000000000000000, 0.000000000000000000, 0.000000000000000000 ) ) ;
#15706 = CARTESIAN_POINT ( 'NONE',  ( -3.464101615137757051, -5.999999999999979572, -117.5863248654052171 ) ) ;
#15707 = CARTESIAN_POINT ( 'NONE',  ( -4.999999999999990230, -55.00000000000002132, 8.000000000000007105 ) ) ;
#15708 = CARTESIAN_POINT ( 'NONE',  ( 23.27382486540533790, -2.499999999999844569, -1.035533905932809473 ) ) ;
#15709 = CARTESIAN_POINT ( 'NONE',  ( 111.0627832217621602, -0.7662911109077987781, -1.849990392679291551 ) ) ;
#15710 = CARTESIAN_POINT ( 'NONE',  ( 2.775557561562891351E-14, 6.250000000000033751, -71.56698729810784698 ) ) ;
#15711 = CARTESIAN_POINT ( 'NONE',  ( 2.775557561562891351E-14, -6.250000000000061284, -52.81698729810779724 ) ) ;
#15712 = CARTESIAN_POINT ( 'NONE',  ( 0.000000000000000000, -5.999999999999991118, -121.0386751345948824 ) ) ;
#15713 = CARTESIAN_POINT ( 'NONE',  ( -4.763139720814407951, 2.749999999999946709, -47.75000000000001421 ) ) ;
#15714 = CARTESIAN_POINT ( 'NONE',  ( 119.9999999999999289, 2.500000000000057732, 1.110223024625156540E-13 ) ) ;
#15715 = FACE_OUTER_BOUND ( 'NONE', #27796, .T. ) ;
#15716 = ADVANCED_FACE ( 'NONE', ( #26852 ), #6138, .T. ) ;
#15717 =( BOUNDED_CURVE ( )  B_SPLINE_CURVE ( 2, ( #29096, #2745, #21061, #16631, #996, #9832, #8055, #19206, #15162 ),
 .UNSPECIFIED., .F., .F. ) 
 B_SPLINE_CURVE_WITH_KNOTS ( ( 3, 2, 2, 2, 3 ),
 ( 0.3906250000000000000, 0.3984375000000000000, 0.4062500000000000000, 0.4140625000000000000, 0.4218750000000000000 ),
 .UNSPECIFIED. ) 
 CURVE ( )  GEOMETRIC_REPRESENTATION_ITEM ( )  RATIONAL_B_SPLINE_CURVE ( ( 1.000000000000000000, 0.9238795325112867385, 1.000000000000000000, 0.9238795325112867385, 1.000000000000000000, 0.9238795325112867385, 1.000000000000000000, 0.9238795325112867385, 1.000000000000000000 ) ) 
 REPRESENTATION_ITEM ( '' )  );
#15718 = CARTESIAN_POINT ( 'NONE',  ( 0.000000000000000000, 5.499999999999991118, -129.0000000000000000 ) ) ;
#15719 = EDGE_CURVE ( 'NONE', #1672, #4112, #3719, .T. ) ;
#15720 = PLANE ( 'NONE',  #27407 ) ;
#15721 = ORIENTED_EDGE ( 'NONE', *, *, #9505, .T. ) ;
#15722 = CARTESIAN_POINT ( 'NONE',  ( -5.196152422706601826, 2.999999999999975131, -132.0386751345948255 ) ) ;
#15723 = CYLINDRICAL_SURFACE ( 'NONE', #9687, 2.000000000000012879 ) ;
#15724 = CARTESIAN_POINT ( 'NONE',  ( 137.9211002691896795, -4.999999999999989342, -2.071067811865468400 ) ) ;
#15725 = VECTOR ( 'NONE', #19812, 1000.000000000000000 ) ;
#15726 = ORIENTED_EDGE ( 'NONE', *, *, #1608, .F. ) ;
#15727 = CARTESIAN_POINT ( 'NONE',  ( 113.9997167782376266, -1.308140751793585022, 1.308140751793862577 ) ) ;
#15728 = SURFACE_STYLE_USAGE ( .BOTH. , #3991 ) ;
#15729 = CARTESIAN_POINT ( 'NONE',  ( -5.412658773652739619, 3.124999999999975131, -113.3169872981077901 ) ) ;
#15730 = CARTESIAN_POINT ( 'NONE',  ( 10.00000000000014744, 0.2433462418246987169, 2.400232754357976450 ) ) ;
#15731 = ORIENTED_EDGE ( 'NONE', *, *, #8784, .T. ) ;
#15732 = LINE ( 'NONE', #22764, #1733 ) ;
#15733 = CARTESIAN_POINT ( 'NONE',  ( 139.5000000000000284, 6.000000000000005329, 0.000000000000000000 ) ) ;
#15734 = VERTEX_POINT ( 'NONE', #16721 ) ;
#15735 = ORIENTED_EDGE ( 'NONE', *, *, #5725, .T. ) ;
#15736 = PRESENTATION_STYLE_ASSIGNMENT (( #29660 ) ) ;
#15737 = CARTESIAN_POINT ( 'NONE',  ( 6.350852961086080661, -9.614813431917819062E-14, -49.87500000000001421 ) ) ;
#15738 = ADVANCED_FACE ( 'NONE', ( #4990 ), #23757, .F. ) ;
#15739 = VECTOR ( 'NONE', #17348, 1000.000000000000000 ) ;
#15740 = CARTESIAN_POINT ( 'NONE',  ( 23.06250000000011013, 2.000000000000151879, 0.8284271247462354770 ) ) ;
#15741 = CARTESIAN_POINT ( 'NONE',  ( 117.2886751345947971, 2.000000000000140332, 2.220446049250313081E-13 ) ) ;
#15742 = DIRECTION ( 'NONE',  ( 1.000000000000000000, 0.000000000000000000, 0.000000000000000000 ) ) ;
#15743 = CARTESIAN_POINT ( 'NONE',  ( -7.216878364870328078, 0.000000000000000000, -64.55801270189225249 ) ) ;
#15744 = TOROIDAL_SURFACE ( 'NONE', #11821, 16.00000000000000000, 1.000000000000000000 ) ;
#15745 = CARTESIAN_POINT ( 'NONE',  ( 152.6101497308104058, 3.535533905932725318, 3.535533905932725318 ) ) ;
#15746 = FACE_OUTER_BOUND ( 'NONE', #17045, .T. ) ;
#15747 = CARTESIAN_POINT ( 'NONE',  ( 2.775557561562891351E-14, 10.99999999999998224, -14.99152654425661702 ) ) ;
#15748 = CIRCLE ( 'NONE', #24495, 1.000000000000000888 ) ;
#15749 = LINE ( 'NONE', #4171, #7427 ) ;
#15750 = CARTESIAN_POINT ( 'NONE',  ( 17.03867513459494987, 1.665334536937734811E-13, -2.500000000000002220 ) ) ;
#15751 = CARTESIAN_POINT ( 'NONE',  ( 106.3511751345947118, 2.000000000000091926, 0.8284271247462955401 ) ) ;
#15752 = EDGE_CURVE ( 'NONE', #7302, #14866, #6880, .T. ) ;
#15753 = CARTESIAN_POINT ( 'NONE',  ( 4.763139720814407951, -2.749999999999988454, -135.5000000000000000 ) ) ;
#15754 = CARTESIAN_POINT ( 'NONE',  ( 3.608439182435180470, 6.249999999999982236, -149.0580127018922667 ) ) ;
#15755 = CARTESIAN_POINT ( 'NONE',  ( 0.000000000000000000, 0.000000000000000000, 0.000000000000000000 ) ) ;
#15756 = DIRECTION ( 'NONE',  ( 0.000000000000000000, 0.000000000000000000, -1.000000000000000000 ) ) ;
#15757 = VERTEX_POINT ( 'NONE', #20891 ) ;
#15758 = CARTESIAN_POINT ( 'NONE',  ( 4.763139720814407951, 2.750000000000002665, -64.75000000000002842 ) ) ;
#15759 = CARTESIAN_POINT ( 'NONE',  ( 0.000000000000000000, 0.000000000000000000, 0.000000000000000000 ) ) ;
#15760 = CARTESIAN_POINT ( 'NONE',  ( -5.999999999999963585, -1.487416814333745711E-14, -171.8363248654052313 ) ) ;
#15761 = CARTESIAN_POINT ( 'NONE',  ( 5.196152422706629359, -2.999999999999988898, -162.7886751345948255 ) ) ;
#15762 = EDGE_LOOP ( 'NONE', ( #14311, #1165, #23314 ) ) ;
#15763 = CARTESIAN_POINT ( 'NONE',  ( 108.7499999999998579, 8.326672684688674053E-14, -2.499999999999835687 ) ) ;
#15764 = CARTESIAN_POINT ( 'NONE',  ( 143.1562500000000284, -6.000000000000005329, 2.485281374238556218 ) ) ;
#15765 = CYLINDRICAL_SURFACE ( 'NONE', #22180, 1.000000000000000000 ) ;
#15766 =( BOUNDED_CURVE ( )  B_SPLINE_CURVE ( 2, ( #14346, #16797, #23684, #17083, #2621, #12041, #16936, #14491, #5214 ),
 .UNSPECIFIED., .F., .F. ) 
 B_SPLINE_CURVE_WITH_KNOTS ( ( 3, 2, 2, 2, 3 ),
 ( 0.3861111111111111271, 0.3870370370370370128, 0.3888888888888888951, 0.3907407407407407218, 0.3916666666666666630 ),
 .UNSPECIFIED. ) 
 CURVE ( )  GEOMETRIC_REPRESENTATION_ITEM ( )  RATIONAL_B_SPLINE_CURVE ( ( 0.9330127018922194093, 0.9330127018922214077, 1.000000000000000000, 0.8660254037844388186, 1.000000000000000000, 0.8660254037844388186, 1.000000000000000000, 0.9330127018922194093, 0.9330127018922194093 ) ) 
 REPRESENTATION_ITEM ( '' )  );
#15767 = COLOUR_RGB ( '', 0.40784314, 0.44705882, 0.49803922) ;
#15768 = CARTESIAN_POINT ( 'NONE',  ( 140.2370868712064862, -11.61854343560322711, -4.230991509104584658 ) ) ;
#15769 = AXIS2_PLACEMENT_3D ( 'NONE', #27687, #6670, #20919 ) ;
#15770 = CARTESIAN_POINT ( 'NONE',  ( 139.5000000000000284, 6.000000000000005329, 0.000000000000000000 ) ) ;
#15771 = CARTESIAN_POINT ( 'NONE',  ( 119.9999999999999289, 2.500000000000057732, 1.110223024625156540E-13 ) ) ;
#15772 = VERTEX_POINT ( 'NONE', #2691 ) ;
#15773 = B_SPLINE_CURVE_WITH_KNOTS ( 'NONE', 3,
 ( #7585, #8344, #17597, #3416, #1121, #26617, #27226, #1430, #22186, #12842, #22498, #8501, #5723, #17442, #8036, #10519, #15296, #1590, #10842, #20195, #5877, #24464, #29545, #17750, #6198, #27075, #22649, #19872, #24784, #29218, #26913, #17908 ),
 .UNSPECIFIED., .F., .F.,
 ( 4, 2, 2, 2, 2, 2, 2, 2, 2, 2, 2, 2, 2, 2, 2, 4 ),
 ( 1.116565195435206273E-15, 0.001893041221572642650, 0.002839561832358405719, 0.003786082443144169005, 0.004732603053929931858, 0.005679123664715694277, 0.006625644275501457563, 0.007572164886287220849, 0.008518685497072985002, 0.009465206107858748288, 0.01041172671864451157, 0.01135824732943027313, 0.01230476794021603641, 0.01325128855100179970, 0.01419780916178756298, 0.01514432977257332627 ),
 .UNSPECIFIED. ) ;
#15774 = CARTESIAN_POINT ( 'NONE',  ( -3.175426480542816510, -5.500000000000057732, -149.3750000000000284 ) ) ;
#15775 = VERTEX_POINT ( 'NONE', #18300 ) ;
#15776 = CARTESIAN_POINT ( 'NONE',  ( 12.81250000000004441, 0.8284271247461753029, -2.000000000000091926 ) ) ;
#15777 = ORIENTED_EDGE ( 'NONE', *, *, #14420, .F. ) ;
#15778 = CARTESIAN_POINT ( 'NONE',  ( -4.763139720814407951, -2.750000000000016431, -76.00000000000001421 ) ) ;
#15779 = EDGE_CURVE ( 'NONE', #20769, #22758, #9777, .T. ) ;
#15780 = EDGE_CURVE ( 'NONE', #18409, #4573, #4717, .T. ) ;
#15781 = CARTESIAN_POINT ( 'NONE',  ( -3.608439182435052128, -6.250000000000110134, -88.30801270189222407 ) ) ;
#15782 = ORIENTED_EDGE ( 'NONE', *, *, #221, .T. ) ;
#15783 = CARTESIAN_POINT ( 'NONE',  ( -1.584453406822390775, -10.89233254831498598, -19.19936552286312903 ) ) ;
#15784 = CARTESIAN_POINT ( 'NONE',  ( -5.999999999999962697, 3.323446944526963891E-14, -149.9136751345948255 ) ) ;
#15785 = FACE_OUTER_BOUND ( 'NONE', #8070, .T. ) ;
#15786 =( GEOMETRIC_REPRESENTATION_CONTEXT ( 3 ) GLOBAL_UNCERTAINTY_ASSIGNED_CONTEXT ( ( #25943 ) ) GLOBAL_UNIT_ASSIGNED_CONTEXT ( ( #4123, #23199, #22884 ) ) REPRESENTATION_CONTEXT ( 'NONE', 'WORKASPACE' ) );
#15787 = CARTESIAN_POINT ( 'NONE',  ( -5.999999999999963585, 1.780251999655701777E-13, -91.41367513459486815 ) ) ;
#15788 = AXIS2_PLACEMENT_3D ( 'NONE', #15157, #991, #8051 ) ;
#15789 = CARTESIAN_POINT ( 'NONE',  ( 3.175426480543072749, -5.500000000000105693, -156.6250000000000000 ) ) ;
#15790 = CARTESIAN_POINT ( 'NONE',  ( 139.5000000000000284, -8.946933499675683521, -8.000000000000007105 ) ) ;
#15791 = CARTESIAN_POINT ( 'NONE',  ( 156.1800748654052882, -2.278174593052098018, 5.499999999999928058 ) ) ;
#15792 = CARTESIAN_POINT ( 'NONE',  ( 3.175426480543072749, -5.500000000000105693, -86.12500000000000000 ) ) ;
#15793 = DIRECTION ( 'NONE',  ( 1.000000000000000000, -5.551115123125773458E-17, -1.260129944081490338E-35 ) ) ;
#15794 = CARTESIAN_POINT ( 'NONE',  ( 3.175426480543072749, 5.499999999999865885, -73.62500000000005684 ) ) ;
#15795 = CARTESIAN_POINT ( 'NONE',  ( 6.000000000000052403, -1.607695154586662678, -74.23066243270258724 ) ) ;
#15796 = CARTESIAN_POINT ( 'NONE',  ( 149.9136751345948539, 0.000000000000000000, -5.500000000000005329 ) ) ;
#15797 = CARTESIAN_POINT ( 'NONE',  ( 5.196152422706629359, -2.999999999999988898, -174.7886751345948255 ) ) ;
#15798 = CARTESIAN_POINT ( 'NONE',  ( -5.196152422706573404, -3.000000000000002665, -76.28867513459481131 ) ) ;
#15799 = CARTESIAN_POINT ( 'NONE',  ( 5.999999999999992006, -3.330669073875460254E-16, -44.99152654425658682 ) ) ;
#15800 = LINE ( 'NONE', #3444, #22969 ) ;
#15801 = CYLINDRICAL_SURFACE ( 'NONE', #28219, 6.000000000000000888 ) ;
#15802 =( BOUNDED_CURVE ( )  B_SPLINE_CURVE ( 2, ( #403, #7760, #2566, #23919, #9792, #14439, #19469, #17025, #16592 ),
 .UNSPECIFIED., .F., .F. ) 
 B_SPLINE_CURVE_WITH_KNOTS ( ( 3, 2, 2, 2, 3 ),
 ( 0.1472222222222221433, 0.1481481481481481399, 0.1500000000000000222, 0.1518518518518519045, 0.1527777777777777901 ),
 .UNSPECIFIED. ) 
 CURVE ( )  GEOMETRIC_REPRESENTATION_ITEM ( )  RATIONAL_B_SPLINE_CURVE ( ( 0.9330127018922194093, 0.9330127018922154125, 1.000000000000000000, 0.8660254037844388186, 1.000000000000000000, 0.8660254037844388186, 1.000000000000000000, 0.9330127018922194093, 0.9330127018922194093 ) ) 
 REPRESENTATION_ITEM ( '' )  );
#15803 = EDGE_LOOP ( 'NONE', ( #13651, #24245, #25341, #3843 ) ) ;
#15804 = CARTESIAN_POINT ( 'NONE',  ( 157.9687500000000284, -2.485281374238585972, 6.000000000000005329 ) ) ;
#15805 = CARTESIAN_POINT ( 'NONE',  ( -3.464101615137757051, -5.999999999999979572, -109.1636751345948113 ) ) ;
#15806 =( REPRESENTATION_RELATIONSHIP ('NONE','NONE', #103, #15661 ) REPRESENTATION_RELATIONSHIP_WITH_TRANSFORMATION ( #29706 )SHAPE_REPRESENTATION_RELATIONSHIP( ) );
#15807 = VECTOR ( 'NONE', #692, 1000.000000000000000 ) ;
#15808 = CARTESIAN_POINT ( 'NONE',  ( 3.464101615137852974, 5.999999999999884537, -179.8363248654051745 ) ) ;
#15809 = ORIENTED_EDGE ( 'NONE', *, *, #1059, .F. ) ;
#15810 =( BOUNDED_CURVE ( )  B_SPLINE_CURVE ( 2, ( #16214, #25368, #13753, #27969, #5488, #28677, #10587, #12608, #19938 ),
 .UNSPECIFIED., .F., .T. ) 
 B_SPLINE_CURVE_WITH_KNOTS ( ( 3, 2, 2, 2, 3 ),
 ( 0.2861111111111111494, 0.2870370370370370350, 0.2888888888888888618, 0.2907407407407407440, 0.2916666666666666297 ),
 .UNSPECIFIED. ) 
 CURVE ( )  GEOMETRIC_REPRESENTATION_ITEM ( )  RATIONAL_B_SPLINE_CURVE ( ( 0.9330127018922194093, 0.9330127018922214077, 1.000000000000000000, 0.8660254037844388186, 1.000000000000000000, 0.8660254037844388186, 1.000000000000000000, 0.9330127018922214077, 0.9330127018922194093 ) ) 
 REPRESENTATION_ITEM ( '' )  );
#15811 = AXIS2_PLACEMENT_3D ( 'NONE', #16889, #18736, #21628 ) ;
#15812 = VERTEX_POINT ( 'NONE', #12116 ) ;
#15813 = CARTESIAN_POINT ( 'NONE',  ( 3.175426480543072749, 5.499999999999865885, -100.6250000000000000 ) ) ;
#15814 = DIRECTION ( 'NONE',  ( -7.147005652999508048E-36, 5.642372883946980038E-36, 1.000000000000000000 ) ) ;
#15815 = ADVANCED_FACE ( 'NONE', ( #18448 ), #11394, .F. ) ;
#15816 = CARTESIAN_POINT ( 'NONE',  ( 2.775557561562891351E-14, -6.250000000000061284, -104.6830127018922241 ) ) ;
#15817 = ORIENTED_EDGE ( 'NONE', *, *, #4523, .F. ) ;
#15818 = DIRECTION ( 'NONE',  ( -0.000000000000000000, -1.000000000000000000, -0.000000000000000000 ) ) ;
#15819 = CARTESIAN_POINT ( 'NONE',  ( 140.5000000000000284, -9.599999999999997868, -7.200000000000011724 ) ) ;
#15820 = CARTESIAN_POINT ( 'NONE',  ( 0.8631338372297875372, -15.37878787878788067, 8.351220472436777342 ) ) ;
#15821 = CARTESIAN_POINT ( 'NONE',  ( 3.608439182435180470, -6.249999999999997335, -53.55801270189220276 ) ) ;
#15822 =( NAMED_UNIT ( * ) PLANE_ANGLE_UNIT ( ) SI_UNIT ( $, .RADIAN. ) );
#15823 = ORIENTED_EDGE ( 'NONE', *, *, #14788, .F. ) ;
#15824 = PRESENTATION_STYLE_ASSIGNMENT (( #27424 ) ) ;
#15825 = CARTESIAN_POINT ( 'NONE',  ( 6.000000000000000888, -1.859271017917181981E-14, -166.5863248654052029 ) ) ;
#15826 = CARTESIAN_POINT ( 'NONE',  ( -2.775557561562891351E-14, -5.500000000000115463, -162.7500000000000000 ) ) ;
#15827 = CARTESIAN_POINT ( 'NONE',  ( 116.9999999999999005, 2.500000000000057732, 1.110223024625156540E-13 ) ) ;
#15828 = CARTESIAN_POINT ( 'NONE',  ( -0.05791364201276149454, -14.59225860131173924, 8.264570319127788167 ) ) ;
#15829 = CIRCLE ( 'NONE', #1058, 5.999999999999999112 ) ;
#15830 = CARTESIAN_POINT ( 'NONE',  ( 3.175426480543072749, 5.499999999999865885, -106.6250000000000284 ) ) ;
#15831 = CARTESIAN_POINT ( 'NONE',  ( 23.96132486540522422, 5.551115123125782702E-14, 2.500000000000002220 ) ) ;
#15832 = DIRECTION ( 'NONE',  ( -7.147005652999508048E-36, 5.642372883946980038E-36, 1.000000000000000000 ) ) ;
#15833 = CARTESIAN_POINT ( 'NONE',  ( -3.175426480542816510, -5.500000000000057732, -101.3750000000000000 ) ) ;
#15834 = CARTESIAN_POINT ( 'NONE',  ( 159.8586002691896795, 2.071067811865468400, 4.999999999999989342 ) ) ;
#15835 = DIRECTION ( 'NONE',  ( 0.000000000000000000, -2.081668171172248016E-17, 1.000000000000000000 ) ) ;
#15836 = CARTESIAN_POINT ( 'NONE',  ( 0.7579858402826514796, -15.51661825218675261, 8.092275262135514069 ) ) ;
#15837 = ORIENTED_EDGE ( 'NONE', *, *, #9780, .T. ) ;
#15838 = CARTESIAN_POINT ( 'NONE',  ( 12.81250000000010303, 1.097466725451559322, 2.649519052838238409 ) ) ;
#15839 = CARTESIAN_POINT ( 'NONE',  ( 117.7499999999998721, 1.387778780781445676E-13, -2.499999999999835687 ) ) ;
#15840 = CARTESIAN_POINT ( 'NONE',  ( 108.6252832217621886, 5.551115123125782702E-14, 1.849990392679634610 ) ) ;
#15841 = CARTESIAN_POINT ( 'NONE',  ( 108.0238248654050182, -0.8284271247461753029, 2.000000000000271783 ) ) ;
#15842 = EDGE_LOOP ( 'NONE', ( #13892, #28889, #11995, #25109 ) ) ;
#15843 = CARTESIAN_POINT ( 'NONE',  ( 109.9613248654051461, 5.551115123125782702E-14, 2.000000000000112799 ) ) ;
#15844 = AXIS2_PLACEMENT_3D ( 'NONE', #13099, #5981, #25016 ) ;
#15845 = EDGE_CURVE ( 'NONE', #9966, #12627, #14534, .T. ) ;
#15846 = CARTESIAN_POINT ( 'NONE',  ( -3.608439182435115633, 6.249999999999965361, -90.94198729810784698 ) ) ;
#15847 = CARTESIAN_POINT ( 'NONE',  ( 6.000000000000000888, 1.743066579297358182E-13, -102.6636751345948397 ) ) ;
#15848 = ORIENTED_EDGE ( 'NONE', *, *, #24279, .F. ) ;
#15849 = CARTESIAN_POINT ( 'NONE',  ( 141.0000000000000284, -54.99999999999989342, -4.000000000000003553 ) ) ;
#15850 = ORIENTED_EDGE ( 'NONE', *, *, #16432, .T. ) ;
#15851 = CARTESIAN_POINT ( 'NONE',  ( 159.3750000000000568, 0.000000000000000000, 6.000000000000005329 ) ) ;
#15852 = ORIENTED_EDGE ( 'NONE', *, *, #10363, .F. ) ;
#15853 = CARTESIAN_POINT ( 'NONE',  ( -6.350852961085760029, -1.281975124255709124E-13, -118.1250000000000142 ) ) ;
#15854 = ADVANCED_FACE ( 'NONE', ( #13705 ), #9928, .T. ) ;
#15855 = CARTESIAN_POINT ( 'NONE',  ( 3.608439182435180470, 6.249999999999982236, -137.0580127018922099 ) ) ;
#15856 = ORIENTED_EDGE ( 'NONE', *, *, #10236, .F. ) ;
#15857 = CARTESIAN_POINT ( 'NONE',  ( -6.000000000000007105, -1.607695154586655129, -57.76933756729741276 ) ) ;
#15858 = CARTESIAN_POINT ( 'NONE',  ( -5.412658773652684552, -3.125000000000099920, -125.0669872981078328 ) ) ;
#15859 = CARTESIAN_POINT ( 'NONE',  ( 7.216878364870455975, -6.409875621278545621E-14, -176.9419872981078754 ) ) ;
#15860 = FILL_AREA_STYLE_COLOUR ( '', #339 ) ;
#15861 = CYLINDRICAL_SURFACE ( 'NONE', #27011, 5.500000000000000000 ) ;
#15862 =( BOUNDED_CURVE ( )  B_SPLINE_CURVE ( 2, ( #23399, #25679, #6639, #15910, #2345, #23093, #29673, #11278, #11442 ),
 .UNSPECIFIED., .F., .F. ) 
 B_SPLINE_CURVE_WITH_KNOTS ( ( 3, 2, 2, 2, 3 ),
 ( 0.5083333333333333037, 0.5092592592592593004, 0.5111111111111110716, 0.5129629629629629539, 0.5138888888888888395 ),
 .UNSPECIFIED. ) 
 CURVE ( )  GEOMETRIC_REPRESENTATION_ITEM ( )  RATIONAL_B_SPLINE_CURVE ( ( 0.9330127018922194093, 0.9330127018922154125, 1.000000000000000000, 0.8660254037844388186, 1.000000000000000000, 0.8660254037844388186, 1.000000000000000000, 0.9330127018922234061, 0.9330127018922194093 ) ) 
 REPRESENTATION_ITEM ( '' )  );
#15863 = ORIENTED_EDGE ( 'NONE', *, *, #19031, .F. ) ;
#15864 = DIRECTION ( 'NONE',  ( -7.147005652999508048E-36, 5.642372883946980038E-36, 1.000000000000000000 ) ) ;
#15865 = CARTESIAN_POINT ( 'NONE',  ( 5.999999999999949374, 1.607695154586804565, -90.59668783648706381 ) ) ;
#15866 = DIRECTION ( 'NONE',  ( -0.000000000000000000, 1.000000000000000000, 0.000000000000000000 ) ) ;
#15867 = CARTESIAN_POINT ( 'NONE',  ( 0.8353273635461547775, -15.41366153578293563, -8.287000568860444005 ) ) ;
#15868 = CARTESIAN_POINT ( 'NONE',  ( 112.8752832217622029, -1.849990392679384810, 0.000000000000000000 ) ) ;
#15869 = CARTESIAN_POINT ( 'NONE',  ( -5.412658773652739619, 3.124999999999975131, -72.81698729810781856 ) ) ;
#15870 = CARTESIAN_POINT ( 'NONE',  ( -3.608439182435052128, -6.250000000000110134, -58.94198729810782567 ) ) ;
#15871 = CARTESIAN_POINT ( 'NONE',  ( -5.196152422706573404, -3.000000000000002665, -121.2886751345948539 ) ) ;
#15872 = CARTESIAN_POINT ( 'NONE',  ( 4.763139720814407951, -2.749999999999988454, -51.49999999999999289 ) ) ;
#15873 = CARTESIAN_POINT ( 'NONE',  ( 6.000000000000000000, 2.951592740943527306E-14, -149.1636751345948824 ) ) ;
#15874 = DIRECTION ( 'NONE',  ( -1.000000000000000000, 0.000000000000000000, 0.000000000000000000 ) ) ;
#15875 = CARTESIAN_POINT ( 'NONE',  ( -4.763139720814407951, 2.749999999999946709, -122.7500000000000284 ) ) ;
#15876 = LINE ( 'NONE', #11245, #6839 ) ;
#15877 = CARTESIAN_POINT ( 'NONE',  ( 104.7401757384973564, 0.1229795387093424036, -1.849864891959644098 ) ) ;
#15878 = ORIENTED_EDGE ( 'NONE', *, *, #5508, .F. ) ;
#15879 = CARTESIAN_POINT ( 'NONE',  ( 3.464101615137852974, 5.999999999999884537, -132.4136751345947971 ) ) ;
#15880 = CARTESIAN_POINT ( 'NONE',  ( -5.999999999999963585, -1.487416814333745711E-14, -122.3363248654052029 ) ) ;
#15881 = CARTESIAN_POINT ( 'NONE',  ( 139.7961002691896510, 2.071067811865468400, -4.999999999999989342 ) ) ;
#15882 = ORIENTED_EDGE ( 'NONE', *, *, #16511, .F. ) ;
#15883 = CARTESIAN_POINT ( 'NONE',  ( 108.1247167782375556, -1.849990392679468076, 2.220446049250313081E-13 ) ) ;
#15884 = LINE ( 'NONE', #22611, #23940 ) ;
#15885 = EDGE_CURVE ( 'NONE', #27983, #17415, #4285, .T. ) ;
#15886 = CARTESIAN_POINT ( 'NONE',  ( 7.216878364870455975, -6.409875621278545621E-14, -118.4419872981078470 ) ) ;
#15887 = CARTESIAN_POINT ( 'NONE',  ( 3.464101615137757051, -5.999999999999979572, -54.33632486540517448 ) ) ;
#15888 = CARTESIAN_POINT ( 'NONE',  ( 10.00000000000014744, 1.172613085279341938, 1.967453276497120429 ) ) ;
#15889 = ORIENTED_EDGE ( 'NONE', *, *, #4870, .T. ) ;
#15890 = ORIENTED_EDGE ( 'NONE', *, *, #18370, .F. ) ;
#15891 = CARTESIAN_POINT ( 'NONE',  ( 159.5331181682643944, -12.11593836010622738, 3.856815297222582650 ) ) ;
#15892 = CARTESIAN_POINT ( 'NONE',  ( 141.9375000000000284, -4.242640687119298093, -4.242640687119298093 ) ) ;
#15893 = ADVANCED_FACE ( 'NONE', ( #21603 ), #24513, .F. ) ;
#15894 = ORIENTED_EDGE ( 'NONE', *, *, #17955, .F. ) ;
#15895 = CARTESIAN_POINT ( 'NONE',  ( 5.412658773652739619, 3.124999999999988898, -143.8169872981078186 ) ) ;
#15896 = ORIENTED_EDGE ( 'NONE', *, *, #17184, .F. ) ;
#15897 = CARTESIAN_POINT ( 'NONE',  ( 19.03867513459492500, 1.110223024625156540E-13, -2.500000000000057732 ) ) ;
#15898 =( NAMED_UNIT ( * ) SI_UNIT ( $, .STERADIAN. ) SOLID_ANGLE_UNIT ( ) );
#15899 = CARTESIAN_POINT ( 'NONE',  ( 22.25000000000010303, 1.110223024625156540E-13, 1.999999999999946265 ) ) ;
#15900 = CARTESIAN_POINT ( 'NONE',  ( 5.196152422706629359, 3.000000000000002665, -62.03867513459482552 ) ) ;
#15901 = CARTESIAN_POINT ( 'NONE',  ( 2.775557561562891351E-14, 6.250000000000033751, -70.93301270189222407 ) ) ;
#15902 =( BOUNDED_CURVE ( )  B_SPLINE_CURVE ( 2, ( #17935, #1458, #3906, #20225, #11168, #27550, #29405, #4061, #27401 ),
 .UNSPECIFIED., .F., .T. ) 
 B_SPLINE_CURVE_WITH_KNOTS ( ( 3, 2, 2, 2, 3 ),
 ( 0.3529411764705882582, 0.3602941176470588203, 0.3676470588235294379, 0.3750000000000000000, 0.3823529411764705621 ),
 .UNSPECIFIED. ) 
 CURVE ( )  GEOMETRIC_REPRESENTATION_ITEM ( )  RATIONAL_B_SPLINE_CURVE ( ( 1.000000000000000000, 0.9238795325112867385, 1.000000000000000000, 0.9238795325112867385, 1.000000000000000000, 0.9238795325112867385, 1.000000000000000000, 0.9238795325112867385, 1.000000000000000000 ) ) 
 REPRESENTATION_ITEM ( '' )  );
#15903 = CARTESIAN_POINT ( 'NONE',  ( 135.1771402107443407, -8.419396982527448614, -8.000000000000007105 ) ) ;
#15904 = AXIS2_PLACEMENT_3D ( 'NONE', #16557, #14253, #26024 ) ;
#15905 = CARTESIAN_POINT ( 'NONE',  ( 152.5163997308104058, 4.999999999999989342, 2.071067811865468400 ) ) ;
#15906 = CARTESIAN_POINT ( 'NONE',  ( 140.5000000000000284, -10.00000000000000888, 7.500000000000007105 ) ) ;
#15907 = CARTESIAN_POINT ( 'NONE',  ( 141.0000000000000284, -8.500000000000007105, -5.000000000000004441 ) ) ;
#15908 = CARTESIAN_POINT ( 'NONE',  ( -5.999999999999963585, 8.134310703387671600E-14, -146.9136751345948255 ) ) ;
#15909 = CARTESIAN_POINT ( 'NONE',  ( -4.999999999999886313, -15.00000000000001421, 8.000000000000007105 ) ) ;
#15910 = CARTESIAN_POINT ( 'NONE',  ( -3.464101615137725076, 5.999999999999979572, -115.0863248654051887 ) ) ;
#15911 = PRODUCT_DEFINITION_FORMATION_WITH_SPECIFIED_SOURCE ( 'ANY', '', #5956, .NOT_KNOWN. ) ;
#15912 = CARTESIAN_POINT ( 'NONE',  ( -3.175426480542816066, 5.499999999999865885, -121.3750000000000284 ) ) ;
#15913 = DIRECTION ( 'NONE',  ( 1.000000000000000000, -5.551115123125773458E-17, -1.260129944081490338E-35 ) ) ;
#15914 = CARTESIAN_POINT ( 'NONE',  ( 7.216878364870455975, -6.409875621278545621E-14, -144.8080127018922667 ) ) ;
#15915 = DIRECTION ( 'NONE',  ( -7.147005652999508048E-36, 5.642372883946980038E-36, 1.000000000000000000 ) ) ;
#15916 = VERTEX_POINT ( 'NONE', #19303 ) ;
#15917 = CARTESIAN_POINT ( 'NONE',  ( 0.000000000000000000, 5.499999999999991118, -54.00000000000004974 ) ) ;
#15918 = ORIENTED_EDGE ( 'NONE', *, *, #9361, .T. ) ;
#15919 = CARTESIAN_POINT ( 'NONE',  ( 120.3747167782374277, 0.000000000000000000, -1.849990392679301543 ) ) ;
#15920 = CARTESIAN_POINT ( 'NONE',  ( 146.3437500000000284, -6.000000000000005329, -2.485281374238556218 ) ) ;
#15921 = CARTESIAN_POINT ( 'NONE',  ( 160.9487148452246572, -11.55421731372604377, -3.248622259074093854 ) ) ;
#15922 = ADVANCED_FACE ( 'NONE', ( #2149 ), #20582, .F. ) ;
#15923 = SURFACE_SIDE_STYLE ('',( #6499 ) ) ;
#15924 = CARTESIAN_POINT ( 'NONE',  ( 137.3437500000000568, -6.000000000000005329, -2.485281374238555774 ) ) ;
#15925 = CARTESIAN_POINT ( 'NONE',  ( -4.999999999999990230, -24.99999999999999289, -7.500000000000007105 ) ) ;
#15926 = EDGE_LOOP ( 'NONE', ( #29578, #1857, #15654, #21057 ) ) ;
#15927 = EDGE_CURVE ( 'NONE', #25700, #11104, #20615, .T. ) ;
#15928 = CARTESIAN_POINT ( 'NONE',  ( 0.000000000000000000, 5.499999999999991118, -138.0000000000000000 ) ) ;
#15929 = EDGE_LOOP ( 'NONE', ( #8608, #13851, #8298, #25443 ) ) ;
#15930 = CARTESIAN_POINT ( 'NONE',  ( 14.93750000000010303, 2.000000000000151879, -0.8284271247462955401 ) ) ;
#15931 = ORIENTED_EDGE ( 'NONE', *, *, #19252, .T. ) ;
#15932 = CARTESIAN_POINT ( 'NONE',  ( 3.175426480543072749, -5.500000000000105693, -72.62500000000005684 ) ) ;
#15933 = CARTESIAN_POINT ( 'NONE',  ( 10.00000000000014566, 1.542760454755543353, -1.608875422785432052 ) ) ;
#15934 = CARTESIAN_POINT ( 'NONE',  ( -5.381246803625084674, -9.595437032880933970, -22.31808132294487734 ) ) ;
#15935 = CARTESIAN_POINT ( 'NONE',  ( -5.999999999999971578, 1.607695154586715303, -106.4806624327025872 ) ) ;
#15936 = CARTESIAN_POINT ( 'NONE',  ( 14.03867513459489125, 5.551115123125782702E-14, -2.500000000000057732 ) ) ;
#15937 = CARTESIAN_POINT ( 'NONE',  ( -6.000000000000000888, 1.067854986875958443E-15, 7.560779664488942560E-35 ) ) ;
#15938 = APPLICATION_PROTOCOL_DEFINITION ( 'draft international standard', 'automotive_design', 1998, #28880 ) ;
#15939 = CARTESIAN_POINT ( 'NONE',  ( -3.175426480542816066, -5.500000000000057732, -149.3750000000000284 ) ) ;
#15940 = DIRECTION ( 'NONE',  ( -1.000000000000000000, -1.665334536937731113E-16, 1.526556658859586792E-16 ) ) ;
#15941 = CARTESIAN_POINT ( 'NONE',  ( 6.000000000000000888, 1.743066579297358182E-13, -95.16367513459482552 ) ) ;
#15942 = CARTESIAN_POINT ( 'NONE',  ( 4.763139720814407951, 2.750000000000002665, -84.25000000000004263 ) ) ;
#15943 = DIRECTION ( 'NONE',  ( 0.8660254037844380415, -0.5000000000000008882, -1.905606012543395233E-16 ) ) ;
#15944 = CARTESIAN_POINT ( 'NONE',  ( 4.763139720814407951, -2.749999999999988454, -77.00000000000001421 ) ) ;
#15945 = CARTESIAN_POINT ( 'NONE',  ( 149.0773502691896510, 5.000000000000004441, 0.000000000000000000 ) ) ;
#15946 = CARTESIAN_POINT ( 'NONE',  ( -5.999999999999963585, 8.134310703387671600E-14, -114.8363248654052171 ) ) ;
#15947 = FACE_OUTER_BOUND ( 'NONE', #13992, .T. ) ;
#15948 = FACE_OUTER_BOUND ( 'NONE', #28877, .T. ) ;
#15949 = CARTESIAN_POINT ( 'NONE',  ( 18.81250000000011013, 0.8284271247462354770, -2.000000000000091926 ) ) ;
#15950 = LINE ( 'NONE', #28015, #25149 ) ;
#15951 = EDGE_CURVE ( 'NONE', #26678, #23968, #8357, .T. ) ;
#15952 = CARTESIAN_POINT ( 'NONE',  ( 119.3122167782375556, -0.7662911109076785410, -1.849990392679411677 ) ) ;
#15953 = CARTESIAN_POINT ( 'NONE',  ( 6.000000000000052403, -1.607695154586662678, -97.65331216351302146 ) ) ;
#15954 = ADVANCED_FACE ( 'NONE', ( #19453 ), #20044, .T. ) ;
#15955 = EDGE_LOOP ( 'NONE', ( #5641, #20327, #2044, #4421 ) ) ;
#15956 = CARTESIAN_POINT ( 'NONE',  ( 153.8437500000000284, -6.000000000000005329, -2.485281374238555774 ) ) ;
#15957 = CARTESIAN_POINT ( 'NONE',  ( 14.64882486540525086, 2.500000000000144773, -1.035533905932749299 ) ) ;
#15958 = DIRECTION ( 'NONE',  ( -7.147005652999508048E-36, 5.642372883946980038E-36, 1.000000000000000000 ) ) ;
#15959 = ORIENTED_EDGE ( 'NONE', *, *, #22928, .T. ) ;
#15960 = ORIENTED_EDGE ( 'NONE', *, *, #8248, .T. ) ;
#15961 = VERTEX_POINT ( 'NONE', #17768 ) ;
#15962 = CARTESIAN_POINT ( 'NONE',  ( 3.175426480543072749, 5.499999999999865885, -99.12500000000005684 ) ) ;
#15963 = CARTESIAN_POINT ( 'NONE',  ( 115.5863248654050892, 1.414213562373201061, -1.414213562373145550 ) ) ;
#15964 = CARTESIAN_POINT ( 'NONE',  ( -7.216878364870328078, 0.000000000000000000, -108.0580127018922667 ) ) ;
#15965 = ORIENTED_EDGE ( 'NONE', *, *, #15018, .T. ) ;
#15966 =( NAMED_UNIT ( * ) SI_UNIT ( $, .STERADIAN. ) SOLID_ANGLE_UNIT ( ) );
#15967 = CARTESIAN_POINT ( 'NONE',  ( -6.350852961085760029, -1.281975124255709124E-13, -149.6250000000000568 ) ) ;
#15968 = CARTESIAN_POINT ( 'NONE',  ( -4.763139720814407951, -2.750000000000016431, -163.0000000000000284 ) ) ;
#15969 = CARTESIAN_POINT ( 'NONE',  ( 3.464101615137757051, -5.999999999999979572, -105.9136751345947829 ) ) ;
#15970 = ORIENTED_EDGE ( 'NONE', *, *, #1820, .T. ) ;
#15971 = CARTESIAN_POINT ( 'NONE',  ( 6.000000000000000888, 1.607695154586715303, -160.5193375672974128 ) ) ;
#15972 = CYLINDRICAL_SURFACE ( 'NONE', #22676, 1.000000000000000888 ) ;
#15973 = CARTESIAN_POINT ( 'NONE',  ( 140.1537810142820604, -9.001257532780330806, 7.936737533466877714 ) ) ;
#15974 = CARTESIAN_POINT ( 'NONE',  ( 0.000000000000000000, 5.499999999999991118, -163.5000000000000284 ) ) ;
#15975 = CARTESIAN_POINT ( 'NONE',  ( 117.3750000000000142, -1.767766952966320915, 1.767766952966431937 ) ) ;
#15976 = CARTESIAN_POINT ( 'NONE',  ( 4.763139720814407951, -2.749999999999988454, -111.5000000000000426 ) ) ;
#15977 = CARTESIAN_POINT ( 'NONE',  ( -3.464101615137725076, 5.999999999999979572, -87.16367513459483973 ) ) ;
#15978 =( BOUNDED_CURVE ( )  B_SPLINE_CURVE ( 2, ( #12018, #21355, #293, #9681, #594, #19070, #28679, #3043, #749 ),
 .UNSPECIFIED., .F., .T. ) 
 B_SPLINE_CURVE_WITH_KNOTS ( ( 3, 2, 2, 2, 3 ),
 ( 0.6861111111111111160, 0.6870370370370370017, 0.6888888888888888840, 0.6907407407407407662, 0.6916666666666666519 ),
 .UNSPECIFIED. ) 
 CURVE ( )  GEOMETRIC_REPRESENTATION_ITEM ( )  RATIONAL_B_SPLINE_CURVE ( ( 0.9330127018922194093, 0.9330127018922194093, 1.000000000000000000, 0.8660254037844388186, 1.000000000000000000, 0.8660254037844388186, 1.000000000000000000, 0.9330127018922194093, 0.9330127018922194093 ) ) 
 REPRESENTATION_ITEM ( '' )  );
#15979 = CARTESIAN_POINT ( 'NONE',  ( -3.175426480542816510, 5.499999999999865885, -95.87500000000002842 ) ) ;
#15980 = CARTESIAN_POINT ( 'NONE',  ( 160.0461002691896795, -2.071067811865468400, 4.999999999999989342 ) ) ;
#15981 =( LENGTH_UNIT ( ) NAMED_UNIT ( * ) SI_UNIT ( .MILLI., .METRE. ) );
#15982 = CARTESIAN_POINT ( 'NONE',  ( -0.08076307744279384582, -15.22030785687954157, 7.625468407401369220 ) ) ;
#15983 = ORIENTED_EDGE ( 'NONE', *, *, #25503, .T. ) ;
#15984 = CARTESIAN_POINT ( 'NONE',  ( 13.00000000000009415, -1.873492889144789952, 1.873492889144845464 ) ) ;
#15985 = CARTESIAN_POINT ( 'NONE',  ( 117.3124999999997300, -1.035533905932689347, 2.500000000000265121 ) ) ;
#15986 = CARTESIAN_POINT ( 'NONE',  ( 0.000000000000000000, 5.999999999999977796, -130.2113248654052029 ) ) ;
#15987 = VECTOR ( 'NONE', #20151, 1000.000000000000000 ) ;
#15988 = CARTESIAN_POINT ( 'NONE',  ( 112.3127832217622455, 1.849990392679411677, -0.7662911109077087390 ) ) ;
#15989 = DIRECTION ( 'NONE',  ( 0.000000000000000000, 0.000000000000000000, 1.000000000000000000 ) ) ;
#15990 = ADVANCED_FACE ( 'NONE', ( #24478 ), #26626, .F. ) ;
#15991 =( BOUNDED_CURVE ( )  B_SPLINE_CURVE ( 2, ( #22798, #27072, #15455, #13157, #20190, #29542, #8498, #24925, #13304 ),
 .UNSPECIFIED., .F., .T. ) 
 B_SPLINE_CURVE_WITH_KNOTS ( ( 3, 2, 2, 2, 3 ),
 ( 0.9805555555555555136, 0.9814814814814815103, 0.9833333333333332815, 0.9851851851851851638, 0.9861111111111111605 ),
 .UNSPECIFIED. ) 
 CURVE ( )  GEOMETRIC_REPRESENTATION_ITEM ( )  RATIONAL_B_SPLINE_CURVE ( ( 0.9330127018922194093, 0.9330127018922154125, 1.000000000000000000, 0.8660254037844388186, 1.000000000000000000, 0.8660254037844388186, 1.000000000000000000, 0.9330127018922154125, 0.9330127018922194093 ) ) 
 REPRESENTATION_ITEM ( '' )  );
#15992 = EDGE_LOOP ( 'NONE', ( #19799, #18320, #9014, #15647 ) ) ;
#15993 = AXIS2_PLACEMENT_3D ( 'NONE', #7666, #19372, #14620 ) ;
#15994 = CARTESIAN_POINT ( 'NONE',  ( 107.9997167782376835, -1.308140751793585022, 1.308140751793640533 ) ) ;
#15995 = CARTESIAN_POINT ( 'NONE',  ( -5.412658773652739619, 3.124999999999975131, -87.81698729810783277 ) ) ;
#15996 = ORIENTED_EDGE ( 'NONE', *, *, #5279, .T. ) ;
#15997 = CARTESIAN_POINT ( 'NONE',  ( -5.380679364423349043, 9.595766763449166348, -27.68326114948589733 ) ) ;
#15998 = VERTEX_POINT ( 'NONE', #5434 ) ;
#15999 = ORIENTED_EDGE ( 'NONE', *, *, #25458, .T. ) ;
#16000 = CARTESIAN_POINT ( 'NONE',  ( 151.8750000000000284, 0.000000000000000000, 6.000000000000005329 ) ) ;
#16001 = ORIENTED_EDGE ( 'NONE', *, *, #30402, .F. ) ;
#16002 = CARTESIAN_POINT ( 'NONE',  ( -3.175426480542816510, -5.500000000000057732, -123.8749999999999716 ) ) ;
#16003 = CARTESIAN_POINT ( 'NONE',  ( 22.00000000000007461, -1.873492889144678930, -1.873492889145011997 ) ) ;
#16004 = CARTESIAN_POINT ( 'NONE',  ( -7.216878364870328078, 0.000000000000000000, -132.0580127018922383 ) ) ;
#16005 = VERTEX_POINT ( 'NONE', #14845 ) ;
#16006 = CARTESIAN_POINT ( 'NONE',  ( 3.608439182435180470, -6.249999999999997335, -169.6919872981078470 ) ) ;
#16007 = CARTESIAN_POINT ( 'NONE',  ( 2.775557561562891351E-14, 6.250000000000033751, -178.0669872981078186 ) ) ;
#16008 = CARTESIAN_POINT ( 'NONE',  ( -0.5000000000000004441, -14.50000000000001243, 8.000000000000007105 ) ) ;
#16009 = CARTESIAN_POINT ( 'NONE',  ( -20.99999999999998224, -25.00000000000010658, 5.000000000000004441 ) ) ;
#16010 = VERTEX_POINT ( 'NONE', #27087 ) ;
#16011 = CARTESIAN_POINT ( 'NONE',  ( 12.00000000000012079, 2.000000000000112799, -1.665334536937734811E-13 ) ) ;
#16012 = CARTESIAN_POINT ( 'NONE',  ( 5.196152422706629359, 3.000000000000002665, -54.53867513459481842 ) ) ;
#16013 = CARTESIAN_POINT ( 'NONE',  ( 5.630955349231442142, 2.071796769705314123, -180.0000000000000568 ) ) ;
#16014 = CARTESIAN_POINT ( 'NONE',  ( 10.00000000000014744, 1.110223024625156540E-13, -5.551115123125782702E-14 ) ) ;
#16015 = CARTESIAN_POINT ( 'NONE',  ( 113.3127832217621176, 1.849990392679501827, -0.7662911109077087390 ) ) ;
#16016 = CARTESIAN_POINT ( 'NONE',  ( -5.412658773652684552, -3.125000000000099920, -74.06698729810784698 ) ) ;
#16017 = CARTESIAN_POINT ( 'NONE',  ( 2.775557561562891351E-14, 6.250000000000033751, -58.06698729810783277 ) ) ;
#16018 = ADVANCED_FACE ( 'NONE', ( #22198 ), #10531, .T. ) ;
#16019 = CYLINDRICAL_SURFACE ( 'NONE', #9328, 6.000000000000000888 ) ;
#16020 = CARTESIAN_POINT ( 'NONE',  ( -5.412658773652684552, -3.125000000000099920, -181.4330127018922667 ) ) ;
#16021 = CARTESIAN_POINT ( 'NONE',  ( 6.000000000000052403, -1.607695154586662678, -111.1533121635129504 ) ) ;
#16022 = CARTESIAN_POINT ( 'NONE',  ( -5.999999999999963585, -1.487416814333745711E-14, -123.8363248654052171 ) ) ;
#16023 = CARTESIAN_POINT ( 'NONE',  ( -3.464101615137757051, -5.999999999999979572, -177.5863248654051745 ) ) ;
#16024 = CARTESIAN_POINT ( 'NONE',  ( 6.350852961086080661, -9.614813431917819062E-14, -124.8749999999999858 ) ) ;
#16025 = CARTESIAN_POINT ( 'NONE',  ( -3.175426480542816510, 5.499999999999865885, -157.3750000000000000 ) ) ;
#16026 = CARTESIAN_POINT ( 'NONE',  ( 0.000000000000000000, 5.999999999999977796, -138.2886751345947971 ) ) ;
#16027 = CARTESIAN_POINT ( 'NONE',  ( 0.000000000000000000, 0.000000000000000000, 0.000000000000000000 ) ) ;
#16028 = EDGE_LOOP ( 'NONE', ( #25029, #6172, #10905, #22879 ) ) ;
#16029 = CARTESIAN_POINT ( 'NONE',  ( 19.62500000000008527, 2.649519052838500421, -5.551115123125782702E-14 ) ) ;
#16030 = CARTESIAN_POINT ( 'NONE',  ( 6.000000000000000888, -1.859271017917181981E-14, -105.6636751345948397 ) ) ;
#16031 = CARTESIAN_POINT ( 'NONE',  ( 0.000000000000000000, 0.000000000000000000, 0.000000000000000000 ) ) ;
#16032 = CARTESIAN_POINT ( 'NONE',  ( 141.7648502691896510, 3.535533905932725318, 3.535533905932752852 ) ) ;
#16033 = ADVANCED_FACE ( 'NONE', ( #3133 ), #15744, .F. ) ;
#16034 = ORIENTED_EDGE ( 'NONE', *, *, #6509, .T. ) ;
#16035 = CARTESIAN_POINT ( 'NONE',  ( 109.4372167782374845, 0.7662911109079189043, -1.849990392679231599 ) ) ;
#16036 = CARTESIAN_POINT ( 'NONE',  ( 151.4925748654052029, 2.278174593051965235, 5.500000000000058620 ) ) ;
#16037 = CARTESIAN_POINT ( 'NONE',  ( 113.3747167782374987, -1.110223024625156540E-13, -1.849990392679523588 ) ) ;
#16038 = CARTESIAN_POINT ( 'NONE',  ( 5.412658773652739619, 3.124999999999988898, -115.3169872981078043 ) ) ;
#16039 = CARTESIAN_POINT ( 'NONE',  ( 0.000000000000000000, 5.999999999999977796, -108.2886751345948397 ) ) ;
#16040 = CARTESIAN_POINT ( 'NONE',  ( 113.5238248654049471, 0.8284271247463257382, -1.999999999999791278 ) ) ;
#16041 = VERTEX_POINT ( 'NONE', #28931 ) ;
#16042 = ORIENTED_EDGE ( 'NONE', *, *, #18463, .T. ) ;
#16043 = CARTESIAN_POINT ( 'NONE',  ( 0.000000000000000000, 0.000000000000000000, 0.000000000000000000 ) ) ;
#16044 = CARTESIAN_POINT ( 'NONE',  ( 142.4062500000000568, 6.000000000000005329, -2.485281374238555774 ) ) ;
#16045 = CARTESIAN_POINT ( 'NONE',  ( -3.608439182435052128, -6.250000000000110134, -144.4419872981078470 ) ) ;
#16046 = EDGE_LOOP ( 'NONE', ( #8095, #22531, #29621, #26829 ) ) ;
#16047 = CYLINDRICAL_SURFACE ( 'NONE', #1303, 4.000000000000010658 ) ;
#16048 = VECTOR ( 'NONE', #4176, 1000.000000000000000 ) ;
#16049 = CARTESIAN_POINT ( 'NONE',  ( 14.60117513459484861, -1.035533905932629173, 2.499999999999784173 ) ) ;
#16050 = CARTESIAN_POINT ( 'NONE',  ( 21.25000000000015632, 0.000000000000000000, 2.000000000000057288 ) ) ;
#16051 = CYLINDRICAL_SURFACE ( 'NONE', #446, 5.500000000000000000 ) ;
#16052 = CARTESIAN_POINT ( 'NONE',  ( 6.000000000000000000, 2.951592740943527306E-14, -151.5863248654052029 ) ) ;
#16053 = CARTESIAN_POINT ( 'NONE',  ( 5.412658773652739619, 3.124999999999988898, -69.68301270189225249 ) ) ;
#16054 = CARTESIAN_POINT ( 'NONE',  ( 141.7351497308104058, 3.535533905932725318, -3.535533905932725318 ) ) ;
#16055 = CARTESIAN_POINT ( 'NONE',  ( 11.97617513459491612, -1.035533905932629173, -2.499999999999964473 ) ) ;
#16056 = CARTESIAN_POINT ( 'NONE',  ( 116.0000000000000142, 0.000000000000000000, -5.500000000000000000 ) ) ;
#16057 = ADVANCED_FACE ( 'NONE', ( #17156 ), #19885, .F. ) ;
#16058 = CARTESIAN_POINT ( 'NONE',  ( 125.0000000000000568, -55.00000000000000711, 8.000000000000007105 ) ) ;
#16059 = EDGE_CURVE ( 'NONE', #12915, #3959, #23753, .T. ) ;
#16060 = CARTESIAN_POINT ( 'NONE',  ( 12.28867513459488947, 2.500000000000113243, -1.110223024625156540E-13 ) ) ;
#16061 =( NAMED_UNIT ( * ) SI_UNIT ( $, .STERADIAN. ) SOLID_ANGLE_UNIT ( ) );
#16062 = CARTESIAN_POINT ( 'NONE',  ( 111.3749999999999289, -1.767766952966320915, 1.767766952966431937 ) ) ;
#16063 = CARTESIAN_POINT ( 'NONE',  ( -4.763139720814407951, 2.749999999999946709, -122.7500000000000284 ) ) ;
#16064 = CARTESIAN_POINT ( 'NONE',  ( 2.775557561562891351E-14, -6.250000000000061284, -143.6830127018922099 ) ) ;
#16065 = CARTESIAN_POINT ( 'NONE',  ( -5.999999999999963585, 1.780251999655701777E-13, -112.4136751345948255 ) ) ;
#16066 = ORIENTED_EDGE ( 'NONE', *, *, #23620, .F. ) ;
#16067 = CARTESIAN_POINT ( 'NONE',  ( -3.175426480542816066, -5.500000000000057732, -51.87500000000002132 ) ) ;
#16068 = DIRECTION ( 'NONE',  ( 1.000000000000000000, -5.551115123125774074E-17, -1.260129944081490338E-35 ) ) ;
#16069 = EDGE_CURVE ( 'NONE', #9311, #16823, #6385, .T. ) ;
#16070 = CARTESIAN_POINT ( 'NONE',  ( -5.999999999999919176, 1.607695154586804565, -69.90331216351299304 ) ) ;
#16071 = LINE ( 'NONE', #11605, #1811 ) ;
#16072 = ORIENTED_EDGE ( 'NONE', *, *, #22885, .F. ) ;
#16073 = CARTESIAN_POINT ( 'NONE',  ( 106.3124999999997584, -1.035533905932659149, 2.500000000000205169 ) ) ;
#16074 = CARTESIAN_POINT ( 'NONE',  ( 142.5937500000000568, 6.000000000000005329, 2.485281374238585972 ) ) ;
#16075 = CARTESIAN_POINT ( 'NONE',  ( -6.000000000000000888, 1.067854986875958443E-15, 7.560779664488942560E-35 ) ) ;
#16076 = CARTESIAN_POINT ( 'NONE',  ( 139.9687500000000284, -2.485281374238585972, 6.000000000000005329 ) ) ;
#16077 = FACE_OUTER_BOUND ( 'NONE', #30222, .T. ) ;
#16078 = CARTESIAN_POINT ( 'NONE',  ( 6.350852961086080661, -9.614813431917819062E-14, -138.3750000000000568 ) ) ;
#16079 =( BOUNDED_CURVE ( )  B_SPLINE_CURVE ( 2, ( #24104, #7377, #606, #11725, #9540, #18933, #14482, #14189, #9992 ),
 .UNSPECIFIED., .F., .T. ) 
 B_SPLINE_CURVE_WITH_KNOTS ( ( 3, 2, 2, 2, 3 ),
 ( 0.4138888888888888618, 0.4148148148148148029, 0.4166666666666666852, 0.4185185185185185119, 0.4194444444444444531 ),
 .UNSPECIFIED. ) 
 CURVE ( )  GEOMETRIC_REPRESENTATION_ITEM ( )  RATIONAL_B_SPLINE_CURVE ( ( 0.9330127018922194093, 0.9330127018922174109, 1.000000000000000000, 0.8660254037844388186, 1.000000000000000000, 0.8660254037844388186, 1.000000000000000000, 0.9330127018922194093, 0.9330127018922194093 ) ) 
 REPRESENTATION_ITEM ( '' )  );
#16080 = CARTESIAN_POINT ( 'NONE',  ( 12.12500000000005329, 1.414213562373201061, 1.414213562373034527 ) ) ;
#16081 = ORIENTED_EDGE ( 'NONE', *, *, #17850, .F. ) ;
#16082 = CARTESIAN_POINT ( 'NONE',  ( -4.763139720814407951, -2.750000000000016431, -64.00000000000000000 ) ) ;
#16083 = CARTESIAN_POINT ( 'NONE',  ( 0.000000000000000000, -5.999999999999991118, -164.5386751345948539 ) ) ;
#16084 = CARTESIAN_POINT ( 'NONE',  ( 10.25000000000000888, 5.551115123125782702E-14, 2.000000000000001776 ) ) ;
#16085 = EDGE_LOOP ( 'NONE', ( #22994, #164, #9081, #9383 ) ) ;
#16086 = AXIS2_PLACEMENT_3D ( 'NONE', #25880, #681, #28767 ) ;
#16087 = CARTESIAN_POINT ( 'NONE',  ( -5.999999999999963585, -1.487416814333745711E-14, -113.9136751345948255 ) ) ;
#16088 = ADVANCED_FACE ( 'NONE', ( #27386 ), #23121, .T. ) ;
#16089 = CARTESIAN_POINT ( 'NONE',  ( 118.6877832217621460, -0.7662911109076785410, 1.849990392679712103 ) ) ;
#16090 = CARTESIAN_POINT ( 'NONE',  ( 0.7502279533883222662, 150.2326934200733888, 181.9927197319565551 ) ) ;
#16091 = CARTESIAN_POINT ( 'NONE',  ( 3.175426480543072749, -5.500000000000105693, -146.1250000000000284 ) ) ;
#16092 = CARTESIAN_POINT ( 'NONE',  ( 139.8812274360932122, -9.071603356455097966, -7.858226389042775928 ) ) ;
#16093 = CARTESIAN_POINT ( 'NONE',  ( -5.412658773652684552, -3.125000000000099920, -158.9330127018922383 ) ) ;
#16094 = CARTESIAN_POINT ( 'NONE',  ( -0.5000000000000009992, -10.00000000000000888, 5.000000000000004441 ) ) ;
#16095 = PRODUCT_DEFINITION_SHAPE ( 'NONE', 'NONE',  #30417 ) ;
#16096 = CARTESIAN_POINT ( 'NONE',  ( -3.175426480542816066, 5.499999999999865885, -76.37500000000001421 ) ) ;
#16097 = STYLED_ITEM ( 'NONE', ( #18204 ), #4571 ) ;
#16098 = CARTESIAN_POINT ( 'NONE',  ( 117.0863248654050892, -1.414213562373090038, 1.414213562373256572 ) ) ;
#16099 = EDGE_CURVE ( 'NONE', #21329, #11022, #776, .T. ) ;
#16100 = CARTESIAN_POINT ( 'NONE',  ( -2.775557561562891351E-14, -5.500000000000115463, -72.75000000000004263 ) ) ;
#16101 = EDGE_CURVE ( 'NONE', #27374, #27987, #16526, .T. ) ;
#16102 = CARTESIAN_POINT ( 'NONE',  ( 3.464101615137852974, 5.999999999999884537, -154.9136751345947971 ) ) ;
#16103 = CARTESIAN_POINT ( 'NONE',  ( 147.5773502691896795, 5.000000000000004441, 0.000000000000000000 ) ) ;
#16104 = CARTESIAN_POINT ( 'NONE',  ( 160.9801477675673311, -5.500000000000006217, -0.4574064797147053274 ) ) ;
#16105 = CARTESIAN_POINT ( 'NONE',  ( 158.2500000000000284, -6.000000000000005329, 0.000000000000000000 ) ) ;
#16106 = FILL_AREA_STYLE ('',( #25729 ) ) ;
#16107 = CARTESIAN_POINT ( 'NONE',  ( 19.50000000000009948, -1.999999999999835243, 0.000000000000000000 ) ) ;
#16108 = DIRECTION ( 'NONE',  ( -1.000000000000000000, -1.665334536937736783E-16, -2.220446049250315546E-16 ) ) ;
#16109 = CARTESIAN_POINT ( 'NONE',  ( 116.9997167782375698, -1.308140751793557266, 1.308140751793862577 ) ) ;
#16110 = CARTESIAN_POINT ( 'NONE',  ( 6.000000000000000888, -1.859271017917181981E-14, -116.1636751345948255 ) ) ;
#16111 = ORIENTED_EDGE ( 'NONE', *, *, #25462, .F. ) ;
#16112 = CARTESIAN_POINT ( 'NONE',  ( 155.9062500000000853, 6.000000000000005329, -2.485281374238555774 ) ) ;
#16113 = VECTOR ( 'NONE', #22443, 1000.000000000000000 ) ;
#16114 = CARTESIAN_POINT ( 'NONE',  ( -5.999999999999962697, 3.323446944526963260E-14, -156.8363248654052313 ) ) ;
#16115 = VERTEX_POINT ( 'NONE', #3887 ) ;
#16116 = ORIENTED_EDGE ( 'NONE', *, *, #473, .F. ) ;
#16117 = VERTEX_POINT ( 'NONE', #13618 ) ;
#16118 = CARTESIAN_POINT ( 'NONE',  ( -3.175426480542816510, -5.500000000000057732, -92.37500000000002842 ) ) ;
#16119 = CARTESIAN_POINT ( 'NONE',  ( 5.412658773652712085, -3.125000000000086153, -107.4330127018922667 ) ) ;
#16120 = VERTEX_POINT ( 'NONE', #18373 ) ;
#16121 = FACE_BOUND ( 'NONE', #23105, .T. ) ;
#16122 = CARTESIAN_POINT ( 'NONE',  ( -2.081668171172168020E-16, -5.204170427930420051E-17, 2.499999999999999112 ) ) ;
#16123 = ADVANCED_FACE ( 'NONE', ( #20660 ), #30008, .T. ) ;
#16124 = CARTESIAN_POINT ( 'NONE',  ( 0.8024951133112347978, -10.97768020916284648, -30.95935331155644477 ) ) ;
#16125 = ORIENTED_EDGE ( 'NONE', *, *, #28205, .F. ) ;
#16126 = CYLINDRICAL_SURFACE ( 'NONE', #10314, 6.000000000000000888 ) ;
#16127 = CARTESIAN_POINT ( 'NONE',  ( 0.000000000000000000, 5.499999999999991118, -172.5000000000000000 ) ) ;
#16128 = CARTESIAN_POINT ( 'NONE',  ( 23.22617513459493921, 2.500000000000205169, -1.035533905932869425 ) ) ;
#16129 = CARTESIAN_POINT ( 'NONE',  ( 4.763139720814407951, -2.749999999999988454, -159.5000000000000284 ) ) ;
#16130 = CARTESIAN_POINT ( 'NONE',  ( 117.3124999999997300, -1.035533905932689347, 2.500000000000265121 ) ) ;
#16131 = FACE_OUTER_BOUND ( 'NONE', #23639, .T. ) ;
#16132 = CARTESIAN_POINT ( 'NONE',  ( 0.000000000000000000, 0.000000000000000000, -200.0000000000000000 ) ) ;
#16133 = EDGE_CURVE ( 'NONE', #29507, #10931, #20768, .T. ) ;
#16134 = CARTESIAN_POINT ( 'NONE',  ( -3.175426480542816510, 5.499999999999865885, -100.3750000000000000 ) ) ;
#16135 = CARTESIAN_POINT ( 'NONE',  ( 161.9211002691896510, -4.999999999999989342, -2.071067811865468400 ) ) ;
#16136 = CARTESIAN_POINT ( 'NONE',  ( 0.7548346512657310159, -15.52549481223858407, 8.075233279249948382 ) ) ;
#16137 = VECTOR ( 'NONE', #14068, 1000.000000000000000 ) ;
#16138 = ORIENTED_EDGE ( 'NONE', *, *, #14701, .F. ) ;
#16139 = CARTESIAN_POINT ( 'NONE',  ( 12.18750000000011369, -2.649519052838238409, -1.097466725451559322 ) ) ;
#16140 = CARTESIAN_POINT ( 'NONE',  ( 118.7499999999997868, -1.665334536937734811E-13, -2.500000000000057732 ) ) ;
#16141 = DIRECTION ( 'NONE',  ( 0.000000000000000000, -1.000000000000000000, 0.000000000000000000 ) ) ;
#16142 = CARTESIAN_POINT ( 'NONE',  ( 107.6877832217621744, -0.7662911109077987781, 1.849990392679652151 ) ) ;
#16143 = CYLINDRICAL_SURFACE ( 'NONE', #11064, 0.5000000000000004441 ) ;
#16144 = AXIS2_PLACEMENT_3D ( 'NONE', #19819, #8284, #24730 ) ;
#16145 = ORIENTED_EDGE ( 'NONE', *, *, #19257, .T. ) ;
#16146 = CARTESIAN_POINT ( 'NONE',  ( 2.775557561562891351E-14, 6.250000000000033751, -86.56698729810786119 ) ) ;
#16147 = VERTEX_POINT ( 'NONE', #25338 ) ;
#16148 = CARTESIAN_POINT ( 'NONE',  ( -3.464101615137757051, -5.999999999999979572, -65.66367513459478289 ) ) ;
#16149 = AXIS2_PLACEMENT_3D ( 'NONE', #12580, #11993, #26207 ) ;
#16150 = CARTESIAN_POINT ( 'NONE',  ( 151.7812500000000284, 2.485281374238585972, 6.000000000000005329 ) ) ;
#16151 = B_SPLINE_CURVE_WITH_KNOTS ( 'NONE', 3,
 ( #15714, #10624, #24878, #5670, #17858, #12950, #27176, #26861, #1077, #3828, #10941, #5821, #22748, #8285, #10467, #3979, #20289, #6147 ),
 .UNSPECIFIED., .F., .F.,
 ( 4, 2, 2, 2, 2, 2, 2, 2, 4 ),
 ( 0.000000000000000000, 0.0005121067916115667898, 0.001024213583223133580, 0.001536320374834700695, 0.002048427166446268027, 0.002560533958057835575, 0.003072640749669401823, 0.003584747541280968938, 0.004096854332892535186 ),
 .UNSPECIFIED. ) ;
#16152 = CARTESIAN_POINT ( 'NONE',  ( -6.350852961085760029, -1.281975124255709124E-13, -124.1250000000000568 ) ) ;
#16153 = CARTESIAN_POINT ( 'NONE',  ( 23.62500000000017408, 1.110223024625156540E-13, 2.649519052838167354 ) ) ;
#16154 = CARTESIAN_POINT ( 'NONE',  ( -3.608439182435115633, 6.249999999999965361, -133.8080127018922951 ) ) ;
#16155 = ORIENTED_EDGE ( 'NONE', *, *, #22745, .F. ) ;
#16156 = SURFACE_STYLE_USAGE ( .BOTH. , #25930 ) ;
#16157 = CARTESIAN_POINT ( 'NONE',  ( 3.608439182435180470, 6.249999999999982236, -166.1919872981078186 ) ) ;
#16158 = CARTESIAN_POINT ( 'NONE',  ( 3.608439182435180470, 6.249999999999982236, -176.6919872981077901 ) ) ;
#16159 = CARTESIAN_POINT ( 'NONE',  ( 159.2683792240647165, -11.08218540272183716, 4.602811073450635782 ) ) ;
#16160 = FACE_OUTER_BOUND ( 'NONE', #4306, .T. ) ;
#16161 = EDGE_CURVE ( 'NONE', #9582, #14656, #2736, .T. ) ;
#16162 = ORIENTED_EDGE ( 'NONE', *, *, #2463, .T. ) ;
#16163 = CARTESIAN_POINT ( 'NONE',  ( 11.43750000000003197, -1.999999999999911626, 0.8284271247462955401 ) ) ;
#16164 = CARTESIAN_POINT ( 'NONE',  ( 0.000000000000000000, 5.999999999999977796, -54.28867513459484684 ) ) ;
#16165 =( BOUNDED_CURVE ( )  B_SPLINE_CURVE ( 2, ( #1146, #995, #15484, #10396, #8529, #29245, #1615, #11017, #24653 ),
 .UNSPECIFIED., .F., .T. ) 
 B_SPLINE_CURVE_WITH_KNOTS ( ( 3, 2, 2, 2, 3 ),
 ( 0.4583333333333332593, 0.4592592592592592560, 0.4611111111111111382, 0.4629629629629629095, 0.4638888888888889062 ),
 .UNSPECIFIED. ) 
 CURVE ( )  GEOMETRIC_REPRESENTATION_ITEM ( )  RATIONAL_B_SPLINE_CURVE ( ( 0.9330127018922194093, 0.9330127018922154125, 1.000000000000000000, 0.8660254037844388186, 1.000000000000000000, 0.8660254037844388186, 1.000000000000000000, 0.9330127018922154125, 0.9330127018922194093 ) ) 
 REPRESENTATION_ITEM ( '' )  );
#16166 = ADVANCED_FACE ( 'NONE', ( #18172 ), #9230, .T. ) ;
#16167 = CARTESIAN_POINT ( 'NONE',  ( 6.000000000000000888, 1.743066579297358182E-13, -96.08632486540521711 ) ) ;
#16168 = CARTESIAN_POINT ( 'NONE',  ( -5.196152422706601826, 2.999999999999975131, -136.5386751345948255 ) ) ;
#16169 = CARTESIAN_POINT ( 'NONE',  ( 157.9613248654052029, -5.500000000000005329, 0.000000000000000000 ) ) ;
#16170 = CARTESIAN_POINT ( 'NONE',  ( 112.5627832217621886, 0.7662911109078588412, 1.849990392679712103 ) ) ;
#16171 = CARTESIAN_POINT ( 'NONE',  ( 3.608439182435180470, 6.249999999999982236, -73.19198729810781856 ) ) ;
#16172 = CARTESIAN_POINT ( 'NONE',  ( 3.608439182435180470, 6.249999999999982236, -61.19198729810783277 ) ) ;
#16173 = CARTESIAN_POINT ( 'NONE',  ( 0.000000000000000000, 5.499999999999991118, -49.49999999999998579 ) ) ;
#16174 = CARTESIAN_POINT ( 'NONE',  ( -5.196152422706573404, -3.000000000000002665, -111.7113248654052455 ) ) ;
#16175 = CARTESIAN_POINT ( 'NONE',  ( -5.196152422706573404, -3.000000000000002665, -123.7113248654052597 ) ) ;
#16176 = CARTESIAN_POINT ( 'NONE',  ( 4.763139720814407951, 2.750000000000002665, -118.7500000000000284 ) ) ;
#16177 =( BOUNDED_CURVE ( )  B_SPLINE_CURVE ( 2, ( #30028, #1765, #15798, #22108, #15048, #8998, #6684, #24238, #21955 ),
 .UNSPECIFIED., .F., .T. ) 
 B_SPLINE_CURVE_WITH_KNOTS ( ( 3, 2, 2, 2, 3 ),
 ( 0.7805555555555555580, 0.7814814814814814437, 0.7833333333333333259, 0.7851851851851852082, 0.7861111111111112049 ),
 .UNSPECIFIED. ) 
 CURVE ( )  GEOMETRIC_REPRESENTATION_ITEM ( )  RATIONAL_B_SPLINE_CURVE ( ( 0.9330127018922194093, 0.9330127018922194093, 1.000000000000000000, 0.8660254037844388186, 1.000000000000000000, 0.8660254037844388186, 1.000000000000000000, 0.9330127018922154125, 0.9330127018922194093 ) ) 
 REPRESENTATION_ITEM ( '' )  );
#16178 = CARTESIAN_POINT ( 'NONE',  ( 135.0000000000000568, -8.936994204536771846, -7.963449837756274796 ) ) ;
#16179 = CARTESIAN_POINT ( 'NONE',  ( -5.999999999999919176, 1.607695154586804565, -153.9033121635130215 ) ) ;
#16180 = ORIENTED_EDGE ( 'NONE', *, *, #28478, .F. ) ;
#16181 = CARTESIAN_POINT ( 'NONE',  ( 20.93750000000008171, -1.097466725451379244, 2.649519052838178457 ) ) ;
#16182 = DIRECTION ( 'NONE',  ( 0.000000000000000000, -1.000000000000000000, 0.000000000000000000 ) ) ;
#16183 = CARTESIAN_POINT ( 'NONE',  ( 0.000000000000000000, 0.000000000000000000, -14.99152654425661702 ) ) ;
#16184 = ORIENTED_EDGE ( 'NONE', *, *, #4463, .T. ) ;
#16185 = CARTESIAN_POINT ( 'NONE',  ( 109.7497167782375698, 1.308140751793640533, 1.308140751793862577 ) ) ;
#16186 = CARTESIAN_POINT ( 'NONE',  ( 150.8363248654052029, 0.000000000000000000, -5.500000000000005329 ) ) ;
#16187 = CARTESIAN_POINT ( 'NONE',  ( 2.775557561562891351E-14, 6.250000000000033751, -107.5669872981078186 ) ) ;
#16188 = CARTESIAN_POINT ( 'NONE',  ( 22.46132486540528106, 1.665334536937734811E-13, -2.500000000000113243 ) ) ;
#16189 = CARTESIAN_POINT ( 'NONE',  ( 0.000000000000000000, 0.000000000000000000, 0.000000000000000000 ) ) ;
#16190 = VERTEX_POINT ( 'NONE', #29956 ) ;
#16191 = ORIENTED_EDGE ( 'NONE', *, *, #14254, .T. ) ;
#16192 = CARTESIAN_POINT ( 'NONE',  ( -5.999999999999963585, 8.134310703387671600E-14, -142.4136751345948539 ) ) ;
#16193 = CARTESIAN_POINT ( 'NONE',  ( 135.7500000000000284, -6.000000000000005329, 0.000000000000000000 ) ) ;
#16194 = ORIENTED_EDGE ( 'NONE', *, *, #601, .F. ) ;
#16195 = CARTESIAN_POINT ( 'NONE',  ( -7.216878364870328078, 0.000000000000000000, -140.1919872981078186 ) ) ;
#16196 = DIRECTION ( 'NONE',  ( 1.734723475976824844E-16, -1.000000000000000000, 0.000000000000000000 ) ) ;
#16197 = CARTESIAN_POINT ( 'NONE',  ( 143.1636751345948255, 0.000000000000000000, 5.500000000000005329 ) ) ;
#16198 = CARTESIAN_POINT ( 'NONE',  ( 22.93749999999995737, 1.999999999999971800, -0.8284271247462354770 ) ) ;
#16199 = CARTESIAN_POINT ( 'NONE',  ( -39.00000000000000000, -20.00000000000021316, 4.000000000000003553 ) ) ;
#16200 = CARTESIAN_POINT ( 'NONE',  ( 5.196152422706629359, -2.999999999999988898, -137.2886751345948539 ) ) ;
#16201 = CARTESIAN_POINT ( 'NONE',  ( 5.412658773652712085, -3.125000000000086153, -69.93301270189222407 ) ) ;
#16202 = EDGE_CURVE ( 'NONE', #15581, #30081, #14852, .T. ) ;
#16203 = CARTESIAN_POINT ( 'NONE',  ( 141.5476497308104058, 0.000000000000000000, -5.000000000000004441 ) ) ;
#16204 = CARTESIAN_POINT ( 'NONE',  ( 11.60117513459491967, -1.035533905932568999, 2.499999999999784173 ) ) ;
#16205 = CARTESIAN_POINT ( 'NONE',  ( -5.999999999999963585, -1.487416814333745711E-14, -54.83632486540523132 ) ) ;
#16206 = DIRECTION ( 'NONE',  ( -1.000000000000000000, -0.000000000000000000, -0.000000000000000000 ) ) ;
#16207 = CARTESIAN_POINT ( 'NONE',  ( 24.73102515769420506, -2.036758492458766057, -1.044594274058695316 ) ) ;
#16208 = PRESENTATION_STYLE_ASSIGNMENT (( #1722 ) ) ;
#16209 = CARTESIAN_POINT ( 'NONE',  ( 109.9999999999999432, 2.500000000000030198, 0.000000000000000000 ) ) ;
#16210 = VECTOR ( 'NONE', #23717, 1000.000000000000000 ) ;
#16211 = CARTESIAN_POINT ( 'NONE',  ( -2.775557561562891351E-14, -5.500000000000115463, -126.7500000000000284 ) ) ;
#16212 = PRESENTATION_LAYER_ASSIGNMENT (  '', '', ( #924 ) ) ;
#16213 = DIRECTION ( 'NONE',  ( -1.000000000000000000, 0.000000000000000000, 0.000000000000000000 ) ) ;
#16214 = CARTESIAN_POINT ( 'NONE',  ( 6.000000000000000888, 7.762456499804234384E-14, -143.1636751345948255 ) ) ;
#16215 = EDGE_LOOP ( 'NONE', ( #4383, #1348, #20959, #7479 ) ) ;
#16216 = CARTESIAN_POINT ( 'NONE',  ( 6.350852961086080661, -9.614813431917819062E-14, -57.37500000000004974 ) ) ;
#16217 = CARTESIAN_POINT ( 'NONE',  ( 5.196152422706629359, 3.000000000000002665, -124.4613248654052313 ) ) ;
#16218 = CARTESIAN_POINT ( 'NONE',  ( 6.000000000000000888, 1.743066579297358182E-13, -52.58632486540518869 ) ) ;
#16219 = CARTESIAN_POINT ( 'NONE',  ( 6.000000000000052403, -1.607695154586662678, -178.6533121635129362 ) ) ;
#16220 = ORIENTED_EDGE ( 'NONE', *, *, #26811, .T. ) ;
#16221 = CARTESIAN_POINT ( 'NONE',  ( 107.2499999999999147, 0.000000000000000000, 2.499999999999946709 ) ) ;
#16222 = CARTESIAN_POINT ( 'NONE',  ( 142.4062500000000284, 6.000000000000005329, -2.485281374238556218 ) ) ;
#16223 = CARTESIAN_POINT ( 'NONE',  ( 12.68750000000013500, -0.8284271247459952248, -1.999999999999911626 ) ) ;
#16224 = CARTESIAN_POINT ( 'NONE',  ( 3.608439182435180470, 6.249999999999982236, -101.6919872981078328 ) ) ;
#16225 = CARTESIAN_POINT ( 'NONE',  ( 142.4136751345948539, 0.000000000000000000, -5.500000000000005329 ) ) ;
#16226 = CARTESIAN_POINT ( 'NONE',  ( 139.3125000000000284, 4.242640687119298093, -4.242640687119298093 ) ) ;
#16227 = CARTESIAN_POINT ( 'NONE',  ( 119.9374999999996874, 2.499999999999852118, -1.035533905932651377 ) ) ;
#16228 = ADVANCED_FACE ( 'NONE', ( #13272 ), #2015, .T. ) ;
#16229 = CIRCLE ( 'NONE', #26938, 1.000000000000000888 ) ;
#16230 = CARTESIAN_POINT ( 'NONE',  ( -3.175426480542816510, 5.499999999999865885, -134.8750000000000000 ) ) ;
#16231 = AXIS2_PLACEMENT_3D ( 'NONE', #13028, #20058, #29403 ) ;
#16232 = ORIENTED_EDGE ( 'NONE', *, *, #27046, .T. ) ;
#16233 = CARTESIAN_POINT ( 'NONE',  ( 11.81250000000005862, 0.8284271247463557142, -2.000000000000031530 ) ) ;
#16234 = VERTEX_POINT ( 'NONE', #6307 ) ;
#16235 = VECTOR ( 'NONE', #25209, 1000.000000000000227 ) ;
#16236 = AXIS2_PLACEMENT_3D ( 'NONE', #27355, #2339, #21232 ) ;
#16237 = CARTESIAN_POINT ( 'NONE',  ( -2.775557561562891351E-14, -5.500000000000115463, -62.25000000000002842 ) ) ;
#16238 = EDGE_CURVE ( 'NONE', #19610, #14931, #1275, .T. ) ;
#16239 = CARTESIAN_POINT ( 'NONE',  ( 119.8988248654050324, 0.8284271247462654530, 2.000000000000151879 ) ) ;
#16240 = CARTESIAN_POINT ( 'NONE',  ( -3.464101615137757051, -5.999999999999979572, -83.66367513459481131 ) ) ;
#16241 = DIRECTION ( 'NONE',  ( 5.551115123125785167E-17, -1.000000000000000000, -8.881784197001256268E-16 ) ) ;
#16242 = CARTESIAN_POINT ( 'NONE',  ( 119.5002832217621886, 1.308140751793640533, 1.308140751793751555 ) ) ;
#16243 = CARTESIAN_POINT ( 'NONE',  ( -4.763139720814407951, -2.750000000000016431, -151.0000000000000284 ) ) ;
#16244 = CARTESIAN_POINT ( 'NONE',  ( 139.9574378273420336, -9.627775814265145726, -7.738041920342903168 ) ) ;
#16245 = CARTESIAN_POINT ( 'NONE',  ( -4.763139720814407951, 2.749999999999946709, -136.2499999999999716 ) ) ;
#16246 = CARTESIAN_POINT ( 'NONE',  ( 2.775557561562891351E-14, -6.250000000000061284, -164.6830127018922383 ) ) ;
#16247 = FILL_AREA_STYLE ('',( #7288 ) ) ;
#16248 = CARTESIAN_POINT ( 'NONE',  ( 105.3988248654049471, -0.8284271247460852639, -1.999999999999851674 ) ) ;
#16249 = CARTESIAN_POINT ( 'NONE',  ( -3.175426480542816066, -5.500000000000057732, -80.37500000000002842 ) ) ;
#16250 =( NAMED_UNIT ( * ) SI_UNIT ( $, .STERADIAN. ) SOLID_ANGLE_UNIT ( ) );
#16251 = CARTESIAN_POINT ( 'NONE',  ( -4.763139720814407951, -2.750000000000016431, -71.50000000000001421 ) ) ;
#16252 = CARTESIAN_POINT ( 'NONE',  ( -3.464101615137725076, 5.999999999999979572, -154.6636751345947971 ) ) ;
#16253 = CARTESIAN_POINT ( 'NONE',  ( 147.4836002691896795, 4.999999999999989342, -2.071067811865468400 ) ) ;
#16254 = DIRECTION ( 'NONE',  ( -7.147005652999508048E-36, 5.642372883946980038E-36, 1.000000000000000000 ) ) ;
#16255 = DIRECTION ( 'NONE',  ( -1.000000000000000000, 0.000000000000000000, 0.000000000000000000 ) ) ;
#16256 = CARTESIAN_POINT ( 'NONE',  ( 155.6250000000000284, 0.000000000000000000, -6.000000000000005329 ) ) ;
#16257 = CARTESIAN_POINT ( 'NONE',  ( 5.999999999999974243, 1.607695154586759934, -134.0966878364870638 ) ) ;
#16258 = CARTESIAN_POINT ( 'NONE',  ( 6.000000000000000888, 1.743066579297358182E-13, -95.16367513459482552 ) ) ;
#16259 = CARTESIAN_POINT ( 'NONE',  ( -5.999999999999904965, -1.607695154586834541, -147.7693375672974128 ) ) ;
#16260 = CARTESIAN_POINT ( 'NONE',  ( 117.4372167782373566, 0.7662911109078888172, -1.849990392679411677 ) ) ;
#16261 = CARTESIAN_POINT ( 'NONE',  ( -3.464101615137725076, 5.999999999999979572, -169.6636751345948255 ) ) ;
#16262 =( BOUNDED_CURVE ( )  B_SPLINE_CURVE ( 2, ( #11453, #20797, #25066, #9258, #13756, #18653, #18803, #4638, #25371 ),
 .UNSPECIFIED., .F., .F. ) 
 B_SPLINE_CURVE_WITH_KNOTS ( ( 3, 2, 2, 2, 3 ),
 ( 0.8027777777777778123, 0.8037037037037036979, 0.8055555555555555802, 0.8074074074074073515, 0.8083333333333333481 ),
 .UNSPECIFIED. ) 
 CURVE ( )  GEOMETRIC_REPRESENTATION_ITEM ( )  RATIONAL_B_SPLINE_CURVE ( ( 0.9330127018922194093, 0.9330127018922234061, 1.000000000000000000, 0.8660254037844388186, 1.000000000000000000, 0.8660254037844388186, 1.000000000000000000, 0.9330127018922154125, 0.9330127018922194093 ) ) 
 REPRESENTATION_ITEM ( '' )  );
#16263 = ORIENTED_EDGE ( 'NONE', *, *, #7201, .F. ) ;
#16264 = CARTESIAN_POINT ( 'NONE',  ( 158.8125000000000284, 4.242640687119298093, -4.242640687119298093 ) ) ;
#16265 = CARTESIAN_POINT ( 'NONE',  ( 14.96132486540535567, 5.551115123125782702E-14, 2.500000000000002220 ) ) ;
#16266 = CARTESIAN_POINT ( 'NONE',  ( 113.4377832217621460, 1.849990392679591977, 0.7662911109080692285 ) ) ;
#16267 = EDGE_CURVE ( 'NONE', #22758, #13173, #23585, .T. ) ;
#16268 = CARTESIAN_POINT ( 'NONE',  ( 5.196152422706629359, -2.999999999999988898, -84.78867513459481131 ) ) ;
#16269 = ORIENTED_EDGE ( 'NONE', *, *, #21884, .T. ) ;
#16270 = VERTEX_POINT ( 'NONE', #13417 ) ;
#16271 = VERTEX_POINT ( 'NONE', #1705 ) ;
#16272 = CARTESIAN_POINT ( 'NONE',  ( -3.175426480542816510, 5.499999999999865885, -92.87500000000002842 ) ) ;
#16273 = CIRCLE ( 'NONE', #26014, 12.00000000000000178 ) ;
#16274 = EDGE_CURVE ( 'NONE', #27307, #22257, #19448, .T. ) ;
#16275 = CARTESIAN_POINT ( 'NONE',  ( -3.608439182435115633, 6.249999999999965361, -105.3080127018922525 ) ) ;
#16276 = ORIENTED_EDGE ( 'NONE', *, *, #8288, .T. ) ;
#16277 =( GEOMETRIC_REPRESENTATION_CONTEXT ( 3 ) GLOBAL_UNCERTAINTY_ASSIGNED_CONTEXT ( ( #24802 ) ) GLOBAL_UNIT_ASSIGNED_CONTEXT ( ( #30165, #6349, #20348 ) ) REPRESENTATION_CONTEXT ( 'NONE', 'WORKASPACE' ) );
#16278 = CARTESIAN_POINT ( 'NONE',  ( 5.799430203125144345, 9.347489878302534194, -23.41021253818531989 ) ) ;
#16279 = DIRECTION ( 'NONE',  ( 5.551115123125785167E-17, -1.000000000000000000, -8.881784197001256268E-16 ) ) ;
#16280 = VERTEX_POINT ( 'NONE', #28100 ) ;
#16281 = FACE_OUTER_BOUND ( 'NONE', #16028, .T. ) ;
#16282 = SURFACE_STYLE_FILL_AREA ( #541 ) ;
#16283 = AXIS2_PLACEMENT_3D ( 'NONE', #21092, #6323, #471 ) ;
#16284 = CARTESIAN_POINT ( 'NONE',  ( 3.175426480543072749, -5.500000000000105693, -168.6250000000000000 ) ) ;
#16285 = CARTESIAN_POINT ( 'NONE',  ( -5.999999999999956479, -1.607695154586745057, -80.84668783648706381 ) ) ;
#16286 = CARTESIAN_POINT ( 'NONE',  ( 4.763139720814407951, 2.750000000000002665, -160.7500000000000568 ) ) ;
#16287 = CARTESIAN_POINT ( 'NONE',  ( 4.763139720814407951, -2.749999999999988454, -101.0000000000000284 ) ) ;
#16288 = CARTESIAN_POINT ( 'NONE',  ( 21.14882486540530593, -2.499999999999904521, 1.035533905932629173 ) ) ;
#16289 = CARTESIAN_POINT ( 'NONE',  ( 6.000000000000000888, 5.577813053751546416E-15, -165.6636751345948255 ) ) ;
#16290 = CARTESIAN_POINT ( 'NONE',  ( 4.763139720814407951, 2.750000000000002665, -99.25000000000000000 ) ) ;
#16291 = CARTESIAN_POINT ( 'NONE',  ( 160.8898502691896510, 3.535533905932725318, -3.535533905932725318 ) ) ;
#16292 = CARTESIAN_POINT ( 'NONE',  ( 0.1148185598142369424, -15.24995533668263370, 8.589789778559206113 ) ) ;
#16293 = EDGE_LOOP ( 'NONE', ( #20527, #10073, #13681, #29725 ) ) ;
#16294 = CARTESIAN_POINT ( 'NONE',  ( 12.75000000000009415, 1.873492889145067508, 1.873492889144900975 ) ) ;
#16295 = CARTESIAN_POINT ( 'NONE',  ( 112.7499999999998579, -5.551115123125782702E-14, -2.499999999999946709 ) ) ;
#16296 = FACE_OUTER_BOUND ( 'NONE', #22377, .T. ) ;
#16297 = CIRCLE ( 'NONE', #24557, 0.5000000000000004441 ) ;
#16298 = CARTESIAN_POINT ( 'NONE',  ( 107.6252832217623308, -2.775557561562891351E-14, 1.849990392679523588 ) ) ;
#16299 = CARTESIAN_POINT ( 'NONE',  ( 158.1636751345948255, 0.000000000000000000, 5.500000000000005329 ) ) ;
#16300 = ORIENTED_EDGE ( 'NONE', *, *, #10236, .T. ) ;
#16301 = CARTESIAN_POINT ( 'NONE',  ( 5.196152422706629359, 3.000000000000002665, -112.4613248654052171 ) ) ;
#16302 = AXIS2_PLACEMENT_3D ( 'NONE', #2431, #11843, #7031 ) ;
#16303 = EDGE_CURVE ( 'NONE', #7661, #10410, #6876, .T. ) ;
#16304 = ORIENTED_EDGE ( 'NONE', *, *, #11215, .F. ) ;
#16305 = CARTESIAN_POINT ( 'NONE',  ( 0.000000000000000000, -5.999999999999991118, -52.96132486540522422 ) ) ;
#16306 = ORIENTED_EDGE ( 'NONE', *, *, #27454, .F. ) ;
#16307 = CARTESIAN_POINT ( 'NONE',  ( 147.6562500000000284, -6.000000000000005329, 2.485281374238555774 ) ) ;
#16308 = VERTEX_POINT ( 'NONE', #30415 ) ;
#16309 =( BOUNDED_CURVE ( )  B_SPLINE_CURVE ( 2, ( #11621, #27992, #30316, #27417, #6963, #8550, #9276, #18672, #22694 ),
 .UNSPECIFIED., .F., .F. ) 
 B_SPLINE_CURVE_WITH_KNOTS ( ( 3, 2, 2, 2, 3 ),
 ( 0.4249999999999999889, 0.4259259259259259300, 0.4277777777777777568, 0.4296296296296296391, 0.4305555555555555802 ),
 .UNSPECIFIED. ) 
 CURVE ( )  GEOMETRIC_REPRESENTATION_ITEM ( )  RATIONAL_B_SPLINE_CURVE ( ( 0.9330127018922194093, 0.9330127018922194093, 1.000000000000000000, 0.8660254037844388186, 1.000000000000000000, 0.8660254037844388186, 1.000000000000000000, 0.9330127018922174109, 0.9330127018922194093 ) ) 
 REPRESENTATION_ITEM ( '' )  );
#16310 = CARTESIAN_POINT ( 'NONE',  ( 0.000000000000000000, 5.499999999999991118, -110.9999999999999858 ) ) ;
#16311 = EDGE_CURVE ( 'NONE', #19788, #16147, #9543, .T. ) ;
#16312 = CARTESIAN_POINT ( 'NONE',  ( -5.412658773652739619, 3.124999999999975131, -135.1830127018922667 ) ) ;
#16313 = ORIENTED_EDGE ( 'NONE', *, *, #17599, .F. ) ;
#16314 = CARTESIAN_POINT ( 'NONE',  ( -3.608439182435052128, -6.250000000000110134, -165.4419872981077901 ) ) ;
#16315 = CARTESIAN_POINT ( 'NONE',  ( -7.216878364870328078, 0.000000000000000000, -180.6919872981078186 ) ) ;
#16316 = VECTOR ( 'NONE', #12631, 1000.000000000000000 ) ;
#16317 = EDGE_LOOP ( 'NONE', ( #4651, #27315, #12293, #13405 ) ) ;
#16318 = CARTESIAN_POINT ( 'NONE',  ( 5.374111793520025770, 2.595803520882615789, -180.0000000000001705 ) ) ;
#16319 = CARTESIAN_POINT ( 'NONE',  ( 0.000000000000000000, 0.000000000000000000, -43.99152654425658682 ) ) ;
#16320 = AXIS2_PLACEMENT_3D ( 'NONE', #28988, #1043, #3638 ) ;
#16321 = CARTESIAN_POINT ( 'NONE',  ( 158.1488248654052029, -3.889087296526011706, -3.889087296526011706 ) ) ;
#16322 = CARTESIAN_POINT ( 'NONE',  ( 108.3127832217620181, 1.849990392679562001, -0.7662911109076485650 ) ) ;
#16323 = CARTESIAN_POINT ( 'NONE',  ( 2.775557561562891351E-14, 6.250000000000033751, -62.56698729810783277 ) ) ;
#16324 = CARTESIAN_POINT ( 'NONE',  ( -5.412658773652684552, -3.125000000000099920, -175.4330127018922667 ) ) ;
#16325 = DIRECTION ( 'NONE',  ( 0.7071067811865555663, 0.000000000000000000, -0.7071067811865394681 ) ) ;
#16326 = CARTESIAN_POINT ( 'NONE',  ( 6.000000000000000888, -1.607695154586752384, -47.23066243270262277 ) ) ;
#16327 = CARTESIAN_POINT ( 'NONE',  ( -6.350852961085760029, -1.281975124255709124E-13, -119.6250000000000142 ) ) ;
#16328 = CARTESIAN_POINT ( 'NONE',  ( 135.4618877836824424, -8.932258562185509732, -8.000000000000047962 ) ) ;
#16329 = CARTESIAN_POINT ( 'NONE',  ( 5.196152422706629359, 3.000000000000002665, -154.4613248654052029 ) ) ;
#16330 = ORIENTED_EDGE ( 'NONE', *, *, #10649, .F. ) ;
#16331 = CARTESIAN_POINT ( 'NONE',  ( 22.25000000000015987, -1.873492889144789952, -1.873492889145178530 ) ) ;
#16332 = CARTESIAN_POINT ( 'NONE',  ( -3.464101615137725076, 5.999999999999979572, -122.5863248654052313 ) ) ;
#16333 = ORIENTED_EDGE ( 'NONE', *, *, #24041, .T. ) ;
#16334 = CIRCLE ( 'NONE', #20221, 30.00000000000000355 ) ;
#16335 = CARTESIAN_POINT ( 'NONE',  ( 111.3747167782376692, -5.551115123125782702E-14, -1.849990392679523588 ) ) ;
#16336 = CARTESIAN_POINT ( 'NONE',  ( 3.464101615137852974, 5.999999999999884537, -121.9136751345948682 ) ) ;
#16337 = CARTESIAN_POINT ( 'NONE',  ( 2.775557561562891351E-14, 6.250000000000033751, -110.5669872981078186 ) ) ;
#16338 = AXIS2_PLACEMENT_3D ( 'NONE', #20784, #18948, #7246 ) ;
#16339 = ADVANCED_FACE ( 'NONE', ( #21370 ), #9695, .T. ) ;
#16340 = CARTESIAN_POINT ( 'NONE',  ( 17.46132486540527395, 5.551115123125782702E-14, -2.500000000000002220 ) ) ;
#16341 = EDGE_CURVE ( 'NONE', #15144, #17475, #4907, .T. ) ;
#16342 = DIRECTION ( 'NONE',  ( -1.000000000000000000, -1.665334536937736783E-16, -2.220446049250315546E-16 ) ) ;
#16343 = VERTEX_POINT ( 'NONE', #9385 ) ;
#16344 = ORIENTED_EDGE ( 'NONE', *, *, #9244, .F. ) ;
#16345 = CARTESIAN_POINT ( 'NONE',  ( 152.0550748654052313, -5.500000000000012434, -2.278174593052012309 ) ) ;
#16346 = CARTESIAN_POINT ( 'NONE',  ( 133.4062500000000568, 6.000000000000005329, -2.485281374238555774 ) ) ;
#16347 =( BOUNDED_CURVE ( )  B_SPLINE_CURVE ( 2, ( #15796, #15483, #5747, #20511, #8528, #10714, #15161, #17933, #24493 ),
 .UNSPECIFIED., .F., .T. ) 
 B_SPLINE_CURVE_WITH_KNOTS ( ( 3, 2, 2, 2, 3 ),
 ( 0.5875000000000001332, 0.5937499999999998890, 0.5999999999999996447, 0.6062499999999992895, 0.6124999999999991562 ),
 .UNSPECIFIED. ) 
 CURVE ( )  GEOMETRIC_REPRESENTATION_ITEM ( )  RATIONAL_B_SPLINE_CURVE ( ( 0.9999999999999986677, 0.9238795325112880708, 1.000000000000000000, 0.9238795325112867385, 1.000000000000000000, 0.9238795325112867385, 1.000000000000000000, 0.9238795325112975076, 0.9999999999999892308 ) ) 
 REPRESENTATION_ITEM ( '' )  );
#16348 = CARTESIAN_POINT ( 'NONE',  ( -7.216878364870328078, 0.000000000000000000, -135.6919872981078754 ) ) ;
#16349 = CARTESIAN_POINT ( 'NONE',  ( 10.18750000000011013, 1.097466725451679892, -2.649519052838419153 ) ) ;
#16350 = CARTESIAN_POINT ( 'NONE',  ( 14.91367513459485039, -1.767766952966265404, -1.767766952966320915 ) ) ;
#16351 = CARTESIAN_POINT ( 'NONE',  ( 21.00000000000007461, 2.000000000000057288, 0.000000000000000000 ) ) ;
#16352 = CARTESIAN_POINT ( 'NONE',  ( 8.673617379884035472E-16, -14.26964382489354399, 8.429284772777599244 ) ) ;
#16353 = CARTESIAN_POINT ( 'NONE',  ( -7.216878364870328078, 0.000000000000000000, -58.55801270189222407 ) ) ;
#16354 = CARTESIAN_POINT ( 'NONE',  ( 142.7663997308104058, -4.999999999999989342, -2.071067811865468400 ) ) ;
#16355 = CARTESIAN_POINT ( 'NONE',  ( 136.0000000000000284, 0.000000000000000000, -12.00000000000000178 ) ) ;
#16356 = CARTESIAN_POINT ( 'NONE',  ( 6.000000000000000888, 1.743066579297358182E-13, -69.66367513459481131 ) ) ;
#16357 = CARTESIAN_POINT ( 'NONE',  ( 156.4761751345948255, 3.889087296526011706, 3.889087296526011706 ) ) ;
#16358 = DIRECTION ( 'NONE',  ( -8.326672684688675286E-17, -2.081668171172168821E-17, 1.000000000000000000 ) ) ;
#16359 = CARTESIAN_POINT ( 'NONE',  ( 108.8749999999999574, 1.767766952966265404, -1.767766952966320915 ) ) ;
#16360 = CYLINDRICAL_SURFACE ( 'NONE', #16283, 6.000000000000000888 ) ;
#16361 = CARTESIAN_POINT ( 'NONE',  ( 115.2261751345946266, 2.000000000000091926, -0.8284271247459952248 ) ) ;
#16362 = PLANE ( 'NONE',  #28732 ) ;
#16363 = VERTEX_POINT ( 'NONE', #16638 ) ;
#16364 = CARTESIAN_POINT ( 'NONE',  ( 4.763139720814407951, -2.749999999999988454, -59.00000000000004974 ) ) ;
#16365 = CARTESIAN_POINT ( 'NONE',  ( 0.000000000000000000, 0.000000000000000000, 0.000000000000000000 ) ) ;
#16366 =( NAMED_UNIT ( * ) SI_UNIT ( $, .STERADIAN. ) SOLID_ANGLE_UNIT ( ) );
#16367 = VERTEX_POINT ( 'NONE', #2612 ) ;
#16368 = CARTESIAN_POINT ( 'NONE',  ( 120.6247167782375413, 1.849990392679579099, 0.000000000000000000 ) ) ;
#16369 = CARTESIAN_POINT ( 'NONE',  ( 140.4375000000000284, -4.242640687119298093, -4.242640687119298093 ) ) ;
#16370 = CARTESIAN_POINT ( 'NONE',  ( 5.412658773652712085, -3.125000000000086153, -100.5669872981078186 ) ) ;
#16371 = LINE ( 'NONE', #13762, #19975 ) ;
#16372 = EDGE_CURVE ( 'NONE', #28281, #3967, #2469, .T. ) ;
#16373 = CARTESIAN_POINT ( 'NONE',  ( 161.0476497308104342, 0.000000000000000000, -5.000000000000004441 ) ) ;
#16374 = CARTESIAN_POINT ( 'NONE',  ( 6.000000000000000888, -3.330669073875464691E-16, -7.560779664488942560E-35 ) ) ;
#16375 = ORIENTED_EDGE ( 'NONE', *, *, #8945, .F. ) ;
#16376 = CARTESIAN_POINT ( 'NONE',  ( -4.763139720814407951, -2.750000000000016431, -136.0000000000000000 ) ) ;
#16377 = VECTOR ( 'NONE', #30133, 1000.000000000000000 ) ;
#16378 = VERTEX_POINT ( 'NONE', #12029 ) ;
#16379 = ORIENTED_EDGE ( 'NONE', *, *, #9538, .T. ) ;
#16380 = CARTESIAN_POINT ( 'NONE',  ( 4.763139720814407951, 2.750000000000002665, -63.25000000000002842 ) ) ;
#16381 = CARTESIAN_POINT ( 'NONE',  ( 10.00000000000014566, 1.739457083235398827, -1.326893112237951700 ) ) ;
#16382 = CARTESIAN_POINT ( 'NONE',  ( 5.999999999999949374, 1.607695154586804565, -94.51933756729744118 ) ) ;
#16383 = PRESENTATION_LAYER_ASSIGNMENT (  '', '', ( #11964 ) ) ;
#16384 = VERTEX_POINT ( 'NONE', #4611 ) ;
#16385 = DIRECTION ( 'NONE',  ( 1.000000000000000000, 0.000000000000000000, 0.000000000000000000 ) ) ;
#16386 = CARTESIAN_POINT ( 'NONE',  ( 106.3122167782376124, -0.7662911109076184779, -1.849990392679351725 ) ) ;
#16387 = LINE ( 'NONE', #2072, #7182 ) ;
#16388 = CARTESIAN_POINT ( 'NONE',  ( 120.3752832217621460, 1.849990392679579099, 0.000000000000000000 ) ) ;
#16389 = CARTESIAN_POINT ( 'NONE',  ( 4.763139720814407951, 2.750000000000002665, -145.7500000000000568 ) ) ;
#16390 = DIRECTION ( 'NONE',  ( 0.000000000000000000, 6.695352868347765393E-17, 1.000000000000000000 ) ) ;
#16391 = CARTESIAN_POINT ( 'NONE',  ( 3.175426480543072749, -5.500000000000105693, -140.1250000000000000 ) ) ;
#16392 = CARTESIAN_POINT ( 'NONE',  ( -3.608439182435115633, 6.249999999999965361, -159.3080127018922667 ) ) ;
#16393 = CARTESIAN_POINT ( 'NONE',  ( 124.9999999999999432, -70.00000000000000000, 7.500000000000007105 ) ) ;
#16394 = ADVANCED_FACE ( 'NONE', ( #23379 ), #2326, .T. ) ;
#16395 = CARTESIAN_POINT ( 'NONE',  ( 4.763139720814407951, 2.750000000000002665, -79.74999999999998579 ) ) ;
#16396 = CARTESIAN_POINT ( 'NONE',  ( 6.000000000000000888, 7.762456499804234384E-14, -140.1636751345948255 ) ) ;
#16397 = FACE_BOUND ( 'NONE', #9188, .T. ) ;
#16398 = CARTESIAN_POINT ( 'NONE',  ( -4.763139720814407951, -2.750000000000016431, -67.00000000000000000 ) ) ;
#16399 =( GEOMETRIC_REPRESENTATION_CONTEXT ( 3 ) GLOBAL_UNCERTAINTY_ASSIGNED_CONTEXT ( ( #115 ) ) GLOBAL_UNIT_ASSIGNED_CONTEXT ( ( #12056, #12209, #2782 ) ) REPRESENTATION_CONTEXT ( 'NONE', 'WORKASPACE' ) );
#16400 = CARTESIAN_POINT ( 'NONE',  ( 150.2023502691896510, 0.000000000000000000, -5.000000000000004441 ) ) ;
#16401 = CYLINDRICAL_SURFACE ( 'NONE', #7349, 6.000000000000000888 ) ;
#16402 = CARTESIAN_POINT ( 'NONE',  ( -5.999999999999964473, 9.063946212346262433E-15, -175.4136751345948824 ) ) ;
#16403 = AXIS2_PLACEMENT_3D ( 'NONE', #25904, #252, #16434 ) ;
#16404 = CARTESIAN_POINT ( 'NONE',  ( 157.3125000000000284, 4.242640687119298093, -4.242640687119298093 ) ) ;
#16405 = FACE_OUTER_BOUND ( 'NONE', #4343, .T. ) ;
#16406 = CARTESIAN_POINT ( 'NONE',  ( 19.75000000000009948, 1.665334536937734811E-13, -2.000000000000001776 ) ) ;
#16407 = CARTESIAN_POINT ( 'NONE',  ( 139.1324251345948824, -5.500000000000012434, -2.278174593052012309 ) ) ;
#16408 = DIRECTION ( 'NONE',  ( 1.000000000000000000, 0.000000000000000000, 0.000000000000000000 ) ) ;
#16409 = CARTESIAN_POINT ( 'NONE',  ( 117.6872167782374845, 1.849990392679621953, 0.7662911109078287542 ) ) ;
#16410 = LINE ( 'NONE', #1770, #1240 ) ;
#16411 = EDGE_CURVE ( 'NONE', #8626, #24992, #6559, .T. ) ;
#16412 = VERTEX_POINT ( 'NONE', #13986 ) ;
#16413 = CARTESIAN_POINT ( 'NONE',  ( 147.9375000000000284, -4.242640687119298093, -4.242640687119298093 ) ) ;
#16414 = FACE_OUTER_BOUND ( 'NONE', #6665, .T. ) ;
#16415 = CARTESIAN_POINT ( 'NONE',  ( 113.5002832217622455, 1.308140751793696044, 1.308140751793640533 ) ) ;
#16416 = CARTESIAN_POINT ( 'NONE',  ( 4.763139720814407951, -2.749999999999988454, -153.5000000000000284 ) ) ;
#16417 = EDGE_LOOP ( 'NONE', ( #9690, #25765, #14592, #14555 ) ) ;
#16418 = ORIENTED_EDGE ( 'NONE', *, *, #7034, .T. ) ;
#16419 = ORIENTED_EDGE ( 'NONE', *, *, #24910, .F. ) ;
#16420 = B_SPLINE_CURVE_WITH_KNOTS ( 'NONE', 3,
 ( #30066, #21027, #2568, #11991, #18733, #8888, #18276, #27589, #3150, #26497 ),
 .UNSPECIFIED., .F., .F.,
 ( 4, 2, 2, 2, 4 ),
 ( 0.01514432977257332627, 0.01608480558703491436, 0.01702528140149650246, 0.01796575721595809055, 0.01890623303041967865 ),
 .UNSPECIFIED. ) ;
#16421 = CARTESIAN_POINT ( 'NONE',  ( -2.775557561562891351E-14, -5.500000000000115463, -92.25000000000000000 ) ) ;
#16422 = CARTESIAN_POINT ( 'NONE',  ( -5.412658773652684552, -3.125000000000099920, -109.4330127018922099 ) ) ;
#16423 = CARTESIAN_POINT ( 'NONE',  ( 1.595708107228637651, 10.89084870836962260, -30.79786109011546102 ) ) ;
#16424 = CARTESIAN_POINT ( 'NONE',  ( 154.8601497308104058, -3.535533905932725318, -3.535533905932725318 ) ) ;
#16425 = CARTESIAN_POINT ( 'NONE',  ( 6.350852961086080661, -9.614813431917819062E-14, -166.8750000000000568 ) ) ;
#16426 = CARTESIAN_POINT ( 'NONE',  ( 0.000000000000000000, -5.999999999999991118, -63.46132486540523132 ) ) ;
#16427 = CARTESIAN_POINT ( 'NONE',  ( 6.000000000000000888, 1.607695154586715303, -47.09668783648704249 ) ) ;
#16428 = CARTESIAN_POINT ( 'NONE',  ( -3.175426480542816066, -5.500000000000057732, -173.3750000000000284 ) ) ;
#16429 = CARTESIAN_POINT ( 'NONE',  ( 147.6488248654052029, -3.889087296526011706, -3.889087296526011706 ) ) ;
#16430 = CARTESIAN_POINT ( 'NONE',  ( 6.350852961086080661, -9.614813431917819062E-14, -154.8750000000000000 ) ) ;
#16431 = CARTESIAN_POINT ( 'NONE',  ( 110.8124999999999432, 1.035533905932719101, -2.499999999999904521 ) ) ;
#16432 = EDGE_CURVE ( 'NONE', #26506, #20437, #10028, .T. ) ;
#16433 = CARTESIAN_POINT ( 'NONE',  ( -3.175426480542816066, -5.500000000000057732, -101.3750000000000000 ) ) ;
#16434 = DIRECTION ( 'NONE',  ( 0.000000000000000000, 0.000000000000000000, -1.000000000000000000 ) ) ;
#16435 = DIRECTION ( 'NONE',  ( -7.147005652999508048E-36, 5.642372883946980038E-36, 1.000000000000000000 ) ) ;
#16436 = CARTESIAN_POINT ( 'NONE',  ( -3.175426480542816510, -5.500000000000057732, -89.37500000000001421 ) ) ;
#16437 =( BOUNDED_SURFACE ( )  B_SPLINE_SURFACE ( 1, 2, ( 
 ( #26949, #29408, #17789, #3603, #13033, #22370, #1306, #8378, #27107, #24813, #22529, #1461, #17938, #15645, #24954, #28169, #2089, #25412, #14111, #18695, #23145, #15952, #7139, #20835, #16559, #6836, #18999, #25732, #4679, #23594, #20993, #28321, #30184, #25877, #23449, #2532, #2387, #25250, #18542, #21139, #27868, #23301, #18846, #4223, #4373, #30340, #2245, #16409, #11647, #11957, #9609, #16260, #4831, #9461, #13640, #9303, #14257, #22986, #16109, #25580, #28017, #18390, #21284, #11798, #30031, #76, #1927, #224, #11333, #6990, #20679, #9002, #27708, #6688, #12393, #9911, #4973, #12097, #12248, #369, #16993, #14408, #23743, #7580, #3120, #26316, #19134, #7732, #2672, #10063, #5273, #10218, #16704, #19579, #16846, #19440, #28915, #7881, #14972, #22026, #24313, #962, #3262, #26171, #12693, #25334, #25184, #4309, #20765, #2011, #18323, #22910, #5872, #15130, #22183, #8177, #16037, #27481, #4150, #6615, #6459, #13728, #18468, #23225, #8933, #25494, #2170, #6766, #11570, #27790, #24461, #23070, #10516, #10682, #12839, #4459, #1851, #13885, #11420, #11255, #20606, #8033, #17439, #29215, #29953, #30111, #26753, #17594, #27636, #9075, #5720, #1115, #19869, #12997, #26908, #15293, #24618, #3567, #1270, #22335, #20027, #8339, #25811, #18928, #7226, #5049, #19212, #23376, #28544, #22238, #1048, #5795, #12921, #29299, #19949, #28687, #8255, #3644, #29758, #25291, #13530, #13683, #11055, #18279, #6265, #15684, #11377, #3946, #1808, #11213, #13082, #22414, #20401, #13375, #10761, #20561, #29451, #1661, #29912, #17830, #27592, #6570, #15994, #4263, #20720, #23023, #30069, #25623, #27903, #409, #5013, #7337, #26070, #9798, #14444, #23186, #28212, #21032, #14298, #2129, #19044, #18889, #7478, #30378, #23778, #23637, #21483, #21326, #28509, #9346, #2711, #18738, #2432, #19177, #11530, #14001, #16598, #23490, #25920, #25451, #4415, #23341, #28059, #2284, #11689, #7032, #4721, #8063, #16890, #26360, #5309, #19614, #19329, #5758, #12732, #564, #22071, #14575, #17479, #15171, #26504, #28956, #12885, #3155, #14723 ),
 ( #2865, #21773, #24356, #7766, #9951, #17333, #12286, #26648, #5458, #19760, #19912, #24504, #14865, #5608, #7621, #3450, #28650, #1003, #29105, #12430, #22222, #10555, #1153, #10406, #3012, #15015, #26209, #24208, #24064, #28804, #720, #23924, #29258, #5162, #10104, #21629, #19475, #17180, #21924, #13494, #10726, #29877, #4228, #29415, #8385, #5913, #4072, #24819, #1466, #17794, #27112, #8857, #6080, #13647, #18240, #11339, #20684, #20525, #22833, #25255, #10878, #8220, #3767, #15495, #6375, #20371, #13198, #17634, #15342, #22534, #24663, #29582, #13040, #18094, #27409, #20235, #8539, #17945, #27259, #6231, #29721, #8701, #15652, #22686, #1774, #4539, #9007, #2392, #18396, #20999, #81, #4378, #25882, #14117, #11962, #4835, #7305, #7145, #21143, #30189, #23151, #4978, #19003, #21289, #228, #14412, #16709, #13805, #11805, #13964, #18851, #2094, #23600, #28175, #11499, #18700, #23306, #2538, #28022, #2676, #26031, #20840, #9155, #18548, #4683, #27873, #16415, #16266, #2249, #11651, #30345, #9309, #6995, #25737, #9764, #19140, #14545, #16851, #26175, #2830, #5121, #373, #28473, #13679, #29754, #15988, #23020, #27588, #19945, #8887, #15374, #13526, #1347, #1497, #5953, #25287, #6261, #4259, #1804, #13370, #27289, #29295, #8251, #20103, #3941, #4104, #17664, #29446, #18119, #22866, #26988, #8734, #17975, #3797, #24696, #3640, #11209, #20398, #22566, #13226, #20557, #18275, #6113, #17825, #8420, #10908, #15682, #13076, #29907, #6566, #24990, #24847, #25139, #22409, #10757, #27145, #15527, #20263, #22713, #29609, #1656, #11052, #27436, #6405, #15840, #7181, #25447, #16593, #9035, #11990, #9646, #21026, #14148, #7331, #28054, #30220, #7027, #13996, #18423, #16142, #16298, #4411, #30373, #30065, #27744, #25618, #18884, #2279, #13838, #11839, #6724, #25771, #9341, #14292, #14440, #263, #18732, #118, #2125, #28356, #23181, #25915, #23632, #6874, #19038, #5008, #16739, #4863, #27900, #21176, #11371, #16444, #9185, #23335, #11527, #20869, #9499, #28204, #18580, #26064, #4570, #11682, #2567, #21321, #4715 ) ),
 .UNSPECIFIED., .F., .F., .F. ) 
 B_SPLINE_SURFACE_WITH_KNOTS ( ( 2, 2 ),
 ( 3, 2, 2, 2, 2, 2, 2, 2, 2, 2, 2, 2, 2, 2, 2, 2, 2, 2, 2, 2, 2, 2, 2, 2, 2, 2, 2, 2, 2, 2, 2, 2, 2, 2, 2, 2, 2, 2, 2, 2, 2, 2, 2, 2, 2, 2, 2, 2, 2, 2, 2, 2, 2, 2, 2, 2, 2, 2, 2, 2, 2, 2, 2, 2, 2, 2, 2, 2, 2, 2, 2, 2, 2, 2, 2, 2, 2, 2, 2, 2, 2, 2, 2, 2, 2, 2, 2, 2, 2, 2, 2, 2, 2, 2, 2, 2, 2, 2, 2, 2, 2, 2, 2, 2, 2, 2, 2, 2, 2, 2, 2, 2, 2, 2, 2, 2, 2, 2, 2, 2, 2, 2, 2, 2, 2, 2, 2, 2, 2, 2, 2, 2, 3 ),
 ( 0.000000000000000000, 1.000000000000000000 ),
 ( 0.000000000000000000, 0.007352941176470588133, 0.01470588235294117627, 0.02205882352941176613, 0.02941176470588235253, 0.03676470588235294240, 0.04411764705882353227, 0.05147058823529411520, 0.05882352941176470507, 0.06617647058823529493, 0.07352941176470588480, 0.08088235294117647467, 0.08823529411764706454, 0.09558823529411764053, 0.1029411764705882304, 0.1102941176470588203, 0.1176470588235294101, 0.1250000000000000000, 0.1323529411764705899, 0.1397058823529411797, 0.1470588235294117696, 0.1544117647058823595, 0.1617647058823529493, 0.1691176470588235392, 0.1764705882352941291, 0.1838235294117647189, 0.1911764705882352811, 0.1985294117647058709, 0.2058823529411764608, 0.2132352941176470507, 0.2205882352941176405, 0.2279411764705882304, 0.2352941176470588203, 0.2426470588235294101, 0.2500000000000000000, 0.2573529411764705621, 0.2647058823529411797, 0.2720588235294117418, 0.2794117647058823595, 0.2867647058823529216, 0.2941176470588235392, 0.3014705882352941013, 0.3088235294117647189, 0.3161764705882352811, 0.3235294117647058987, 0.3308823529411764608, 0.3382352941176470784, 0.3455882352941176405, 0.3529411764705882582, 0.3602941176470588203, 0.3676470588235294379, 0.3750000000000000000, 0.3823529411764705621, 0.3897058823529411797, 0.3970588235294117418, 0.4044117647058823595, 0.4117647058823529216, 0.4191176470588235392, 0.4264705882352941013, 0.4338235294117647189, 0.4411764705882352811, 0.4485294117647058987, 0.4558823529411764608, 0.4632352941176470784, 0.4705882352941176405, 0.4779411764705882582, 0.4852941176470588203, 0.4926470588235294379, 0.5000000000000000000, 0.5073529411764705621, 0.5147058823529411242, 0.5220588235294117974, 0.5294117647058823595, 0.5367647058823529216, 0.5441176470588234837, 0.5514705882352941568, 0.5588235294117647189, 0.5661764705882352811, 0.5735294117647058432, 0.5808823529411765163, 0.5882352941176470784, 0.5955882352941176405, 0.6029411764705882026, 0.6102941176470588758, 0.6176470588235294379, 0.6250000000000000000, 0.6323529411764705621, 0.6397058823529411242, 0.6470588235294117974, 0.6544117647058823595, 0.6617647058823529216, 0.6691176470588234837, 0.6764705882352941568, 0.6838235294117647189, 0.6911764705882352811, 0.6985294117647058432, 0.7058823529411765163, 0.7132352941176470784, 0.7205882352941176405, 0.7279411764705882026, 0.7352941176470588758, 0.7426470588235294379, 0.7500000000000000000, 0.7573529411764705621, 0.7647058823529411242, 0.7720588235294117974, 0.7794117647058823595, 0.7867647058823529216, 0.7941176470588234837, 0.8014705882352941568, 0.8088235294117647189, 0.8161764705882352811, 0.8235294117647058432, 0.8308823529411765163, 0.8382352941176470784, 0.8455882352941176405, 0.8529411764705882026, 0.8602941176470588758, 0.8676470588235294379, 0.8750000000000000000, 0.8823529411764705621, 0.8897058823529411242, 0.8970588235294117974, 0.9044117647058823595, 0.9117647058823529216, 0.9191176470588234837, 0.9264705882352941568, 0.9338235294117647189, 0.9411764705882352811, 0.9485294117647058432, 0.9558823529411765163, 0.9632352941176470784, 0.9705882352941176405 ),
 .UNSPECIFIED. ) 
 GEOMETRIC_REPRESENTATION_ITEM ( )  RATIONAL_B_SPLINE_SURFACE ( (
 ( 1.000000000000000000, 0.9238795325112867385, 1.000000000000000000, 0.9238795325112867385, 1.000000000000000000, 0.9238795325112867385, 1.000000000000000000, 0.9238795325112867385, 1.000000000000000000, 0.9238795325112867385, 1.000000000000000000, 0.9238795325112867385, 1.000000000000000000, 0.9238795325112867385, 1.000000000000000000, 0.9238795325112867385, 1.000000000000000000, 0.9238795325112867385, 1.000000000000000000, 0.9238795325112867385, 1.000000000000000000, 0.9238795325112867385, 1.000000000000000000, 0.9238795325112867385, 1.000000000000000000, 0.9238795325112867385, 1.000000000000000000, 0.9238795325112867385, 1.000000000000000000, 0.9238795325112867385, 1.000000000000000000, 0.9238795325112867385, 1.000000000000000000, 0.9238795325112867385, 1.000000000000000000, 0.9238795325112867385, 1.000000000000000000, 0.9238795325112867385, 1.000000000000000000, 0.9238795325112867385, 1.000000000000000000, 0.9238795325112867385, 1.000000000000000000, 0.9238795325112867385, 1.000000000000000000, 0.9238795325112867385, 1.000000000000000000, 0.9238795325112867385, 1.000000000000000000, 0.9238795325112867385, 1.000000000000000000, 0.9238795325112867385, 1.000000000000000000, 0.9238795325112867385, 1.000000000000000000, 0.9238795325112867385, 1.000000000000000000, 0.9238795325112867385, 1.000000000000000000, 0.9238795325112867385, 1.000000000000000000, 0.9238795325112867385, 1.000000000000000000, 0.9238795325112867385, 1.000000000000000000, 0.9238795325112867385, 1.000000000000000000, 0.9238795325112867385, 1.000000000000000000, 0.9238795325112867385, 1.000000000000000000, 0.9238795325112867385, 1.000000000000000000, 0.9238795325112867385, 1.000000000000000000, 0.9238795325112867385, 1.000000000000000000, 0.9238795325112867385, 1.000000000000000000, 0.9238795325112867385, 1.000000000000000000, 0.9238795325112867385, 1.000000000000000000, 0.9238795325112867385, 1.000000000000000000, 0.9238795325112867385, 1.000000000000000000, 0.9238795325112867385, 1.000000000000000000, 0.9238795325112867385, 1.000000000000000000, 0.9238795325112867385, 1.000000000000000000, 0.9238795325112867385, 1.000000000000000000, 0.9238795325112867385, 1.000000000000000000, 0.9238795325112867385, 1.000000000000000000, 0.9238795325112867385, 1.000000000000000000, 0.9238795325112867385, 1.000000000000000000, 0.9238795325112867385, 1.000000000000000000, 0.9238795325112867385, 1.000000000000000000, 0.9238795325112867385, 1.000000000000000000, 0.9238795325112867385, 1.000000000000000000, 0.9238795325112867385, 1.000000000000000000, 0.9238795325112867385, 1.000000000000000000, 0.9238795325112867385, 1.000000000000000000, 0.9238795325112867385, 1.000000000000000000, 0.9238795325112867385, 1.000000000000000000, 0.9238795325112867385, 1.000000000000000000, 0.9238795325112867385, 1.000000000000000000, 0.9238795325112867385, 1.000000000000000000, 0.9238795325112867385, 1.000000000000000000, 0.9238795325112867385, 1.000000000000000000, 0.9238795325112867385, 1.000000000000000000, 0.9238795325112867385, 1.000000000000000000, 0.9238795325112867385, 1.000000000000000000, 0.9238795325112867385, 1.000000000000000000, 0.9238795325112867385, 1.000000000000000000, 0.9238795325112867385, 1.000000000000000000, 0.9238795325112867385, 1.000000000000000000, 0.9238795325112867385, 1.000000000000000000, 0.9238795325112867385, 1.000000000000000000, 0.9238795325112867385, 1.000000000000000000, 0.9238795325112867385, 1.000000000000000000, 0.9238795325112867385, 1.000000000000000000, 0.9238795325112867385, 1.000000000000000000, 0.9238795325112867385, 1.000000000000000000, 0.9238795325112867385, 1.000000000000000000, 0.9238795325112867385, 1.000000000000000000, 0.9238795325112867385, 1.000000000000000000, 0.9238795325112867385, 1.000000000000000000, 0.9238795325112867385, 1.000000000000000000, 0.9238795325112867385, 1.000000000000000000, 0.9238795325112867385, 1.000000000000000000, 0.9238795325112867385, 1.000000000000000000, 0.9238795325112867385, 1.000000000000000000, 0.9238795325112867385, 1.000000000000000000, 0.9238795325112867385, 1.000000000000000000, 0.9238795325112867385, 1.000000000000000000, 0.9238795325112867385, 1.000000000000000000, 0.9238795325112867385, 1.000000000000000000, 0.9238795325112867385, 1.000000000000000000, 0.9238795325112867385, 1.000000000000000000, 0.9238795325112867385, 1.000000000000000000, 0.9238795325112867385, 1.000000000000000000, 0.9238795325112867385, 1.000000000000000000, 0.9238795325112867385, 1.000000000000000000, 0.9238795325112867385, 1.000000000000000000, 0.9238795325112867385, 1.000000000000000000, 0.9238795325112867385, 1.000000000000000000, 0.9238795325112867385, 1.000000000000000000, 0.9238795325112867385, 1.000000000000000000, 0.9238795325112867385, 1.000000000000000000, 0.9238795325112867385, 1.000000000000000000, 0.9238795325112867385, 1.000000000000000000, 0.9238795325112867385, 1.000000000000000000, 0.9238795325112867385, 1.000000000000000000, 0.9238795325112867385, 1.000000000000000000, 0.9238795325112867385, 1.000000000000000000, 0.9238795325112867385, 1.000000000000000000, 0.9238795325112867385, 1.000000000000000000, 0.9238795325112867385, 1.000000000000000000, 0.9238795325112867385, 1.000000000000000000, 0.9238795325112867385, 1.000000000000000000, 0.9238795325112867385, 1.000000000000000000, 0.9238795325112867385, 1.000000000000000000, 0.9238795325112867385, 1.000000000000000000, 0.9238795325112867385, 1.000000000000000000, 0.9238795325112867385, 1.000000000000000000, 0.9238795325112867385, 1.000000000000000000, 0.9238795325112867385, 1.000000000000000000, 0.9238795325112867385, 1.000000000000000000, 0.9238795325112867385, 1.000000000000000000, 0.9238795325112867385, 1.000000000000000000, 0.9238795325112867385, 1.000000000000000000, 0.9238795325112867385, 1.000000000000000000, 0.9238795325112867385, 1.000000000000000000, 0.9238795325112867385, 1.000000000000000000, 0.9238795325112867385, 1.000000000000000000, 0.9238795325112867385, 1.000000000000000000),
 ( 1.000000000000000000, 0.9238795325112867385, 1.000000000000000000, 0.9238795325112867385, 1.000000000000000000, 0.9238795325112867385, 1.000000000000000000, 0.9238795325112867385, 1.000000000000000000, 0.9238795325112867385, 1.000000000000000000, 0.9238795325112867385, 1.000000000000000000, 0.9238795325112867385, 1.000000000000000000, 0.9238795325112867385, 1.000000000000000000, 0.9238795325112867385, 1.000000000000000000, 0.9238795325112867385, 1.000000000000000000, 0.9238795325112867385, 1.000000000000000000, 0.9238795325112867385, 1.000000000000000000, 0.9238795325112867385, 1.000000000000000000, 0.9238795325112867385, 1.000000000000000000, 0.9238795325112867385, 1.000000000000000000, 0.9238795325112867385, 1.000000000000000000, 0.9238795325112867385, 1.000000000000000000, 0.9238795325112867385, 1.000000000000000000, 0.9238795325112867385, 1.000000000000000000, 0.9238795325112867385, 1.000000000000000000, 0.9238795325112867385, 1.000000000000000000, 0.9238795325112867385, 1.000000000000000000, 0.9238795325112867385, 1.000000000000000000, 0.9238795325112867385, 1.000000000000000000, 0.9238795325112867385, 1.000000000000000000, 0.9238795325112867385, 1.000000000000000000, 0.9238795325112867385, 1.000000000000000000, 0.9238795325112867385, 1.000000000000000000, 0.9238795325112867385, 1.000000000000000000, 0.9238795325112867385, 1.000000000000000000, 0.9238795325112867385, 1.000000000000000000, 0.9238795325112867385, 1.000000000000000000, 0.9238795325112867385, 1.000000000000000000, 0.9238795325112867385, 1.000000000000000000, 0.9238795325112867385, 1.000000000000000000, 0.9238795325112867385, 1.000000000000000000, 0.9238795325112867385, 1.000000000000000000, 0.9238795325112867385, 1.000000000000000000, 0.9238795325112867385, 1.000000000000000000, 0.9238795325112867385, 1.000000000000000000, 0.9238795325112867385, 1.000000000000000000, 0.9238795325112867385, 1.000000000000000000, 0.9238795325112867385, 1.000000000000000000, 0.9238795325112867385, 1.000000000000000000, 0.9238795325112867385, 1.000000000000000000, 0.9238795325112867385, 1.000000000000000000, 0.9238795325112867385, 1.000000000000000000, 0.9238795325112867385, 1.000000000000000000, 0.9238795325112867385, 1.000000000000000000, 0.9238795325112867385, 1.000000000000000000, 0.9238795325112867385, 1.000000000000000000, 0.9238795325112867385, 1.000000000000000000, 0.9238795325112867385, 1.000000000000000000, 0.9238795325112867385, 1.000000000000000000, 0.9238795325112867385, 1.000000000000000000, 0.9238795325112867385, 1.000000000000000000, 0.9238795325112867385, 1.000000000000000000, 0.9238795325112867385, 1.000000000000000000, 0.9238795325112867385, 1.000000000000000000, 0.9238795325112867385, 1.000000000000000000, 0.9238795325112867385, 1.000000000000000000, 0.9238795325112867385, 1.000000000000000000, 0.9238795325112867385, 1.000000000000000000, 0.9238795325112867385, 1.000000000000000000, 0.9238795325112867385, 1.000000000000000000, 0.9238795325112867385, 1.000000000000000000, 0.9238795325112867385, 1.000000000000000000, 0.9238795325112867385, 1.000000000000000000, 0.9238795325112867385, 1.000000000000000000, 0.9238795325112867385, 1.000000000000000000, 0.9238795325112867385, 1.000000000000000000, 0.9238795325112867385, 1.000000000000000000, 0.9238795325112867385, 1.000000000000000000, 0.9238795325112867385, 1.000000000000000000, 0.9238795325112867385, 1.000000000000000000, 0.9238795325112867385, 1.000000000000000000, 0.9238795325112867385, 1.000000000000000000, 0.9238795325112867385, 1.000000000000000000, 0.9238795325112867385, 1.000000000000000000, 0.9238795325112867385, 1.000000000000000000, 0.9238795325112867385, 1.000000000000000000, 0.9238795325112867385, 1.000000000000000000, 0.9238795325112867385, 1.000000000000000000, 0.9238795325112867385, 1.000000000000000000, 0.9238795325112867385, 1.000000000000000000, 0.9238795325112867385, 1.000000000000000000, 0.9238795325112867385, 1.000000000000000000, 0.9238795325112867385, 1.000000000000000000, 0.9238795325112867385, 1.000000000000000000, 0.9238795325112867385, 1.000000000000000000, 0.9238795325112867385, 1.000000000000000000, 0.9238795325112867385, 1.000000000000000000, 0.9238795325112867385, 1.000000000000000000, 0.9238795325112867385, 1.000000000000000000, 0.9238795325112867385, 1.000000000000000000, 0.9238795325112867385, 1.000000000000000000, 0.9238795325112867385, 1.000000000000000000, 0.9238795325112867385, 1.000000000000000000, 0.9238795325112867385, 1.000000000000000000, 0.9238795325112867385, 1.000000000000000000, 0.9238795325112867385, 1.000000000000000000, 0.9238795325112867385, 1.000000000000000000, 0.9238795325112867385, 1.000000000000000000, 0.9238795325112867385, 1.000000000000000000, 0.9238795325112867385, 1.000000000000000000, 0.9238795325112867385, 1.000000000000000000, 0.9238795325112867385, 1.000000000000000000, 0.9238795325112867385, 1.000000000000000000, 0.9238795325112867385, 1.000000000000000000, 0.9238795325112867385, 1.000000000000000000, 0.9238795325112867385, 1.000000000000000000, 0.9238795325112867385, 1.000000000000000000, 0.9238795325112867385, 1.000000000000000000, 0.9238795325112867385, 1.000000000000000000, 0.9238795325112867385, 1.000000000000000000, 0.9238795325112867385, 1.000000000000000000, 0.9238795325112867385, 1.000000000000000000, 0.9238795325112867385, 1.000000000000000000, 0.9238795325112867385, 1.000000000000000000, 0.9238795325112867385, 1.000000000000000000, 0.9238795325112867385, 1.000000000000000000, 0.9238795325112867385, 1.000000000000000000, 0.9238795325112867385, 1.000000000000000000, 0.9238795325112867385, 1.000000000000000000, 0.9238795325112867385, 1.000000000000000000, 0.9238795325112867385, 1.000000000000000000, 0.9238795325112867385, 1.000000000000000000, 0.9238795325112867385, 1.000000000000000000, 0.9238795325112867385, 1.000000000000000000, 0.9238795325112867385, 1.000000000000000000, 0.9238795325112867385, 1.000000000000000000, 0.9238795325112867385, 1.000000000000000000) ) ) 
 REPRESENTATION_ITEM ( '' )  SURFACE ( )  );
#16438 = CARTESIAN_POINT ( 'NONE',  ( 160.5148502691896510, -3.535533905932725318, -3.535533905932725318 ) ) ;
#16439 = DIRECTION ( 'NONE',  ( -7.147005652999508048E-36, 5.642372883946980038E-36, 1.000000000000000000 ) ) ;
#16440 = ORIENTED_EDGE ( 'NONE', *, *, #4500, .F. ) ;
#16441 = CARTESIAN_POINT ( 'NONE',  ( 10.37500000000013500, 1.665334536937734811E-13, -2.649519052838444910 ) ) ;
#16442 = CARTESIAN_POINT ( 'NONE',  ( 113.6249999999998721, -1.767766952966376426, -1.767766952966431937 ) ) ;
#16443 = CYLINDRICAL_SURFACE ( 'NONE', #17367, 6.000000000000000888 ) ;
#16444 = CARTESIAN_POINT ( 'NONE',  ( 105.6877832217623023, -0.7662911109077987781, 1.849990392679532247 ) ) ;
#16445 = EDGE_CURVE ( 'NONE', #4894, #11998, #6398, .T. ) ;
#16446 = CARTESIAN_POINT ( 'NONE',  ( 157.4136751345948539, 0.000000000000000000, -5.500000000000005329 ) ) ;
#16447 = ORIENTED_EDGE ( 'NONE', *, *, #6574, .F. ) ;
#16448 = CARTESIAN_POINT ( 'NONE',  ( 114.2886751345947971, 2.000000000000029310, 1.110223024625156540E-13 ) ) ;
#16449 = DIRECTION ( 'NONE',  ( 0.000000000000000000, 0.000000000000000000, -1.000000000000000000 ) ) ;
#16450 = DIRECTION ( 'NONE',  ( 1.000000000000000000, -5.551115123125774074E-17, 0.000000000000000000 ) ) ;
#16451 = ORIENTED_EDGE ( 'NONE', *, *, #2285, .F. ) ;
#16452 = CARTESIAN_POINT ( 'NONE',  ( -3.464101615137757051, -5.999999999999979572, -53.08632486540517448 ) ) ;
#16453 = CARTESIAN_POINT ( 'NONE',  ( 153.2812500000000568, 2.485281374238585972, 6.000000000000005329 ) ) ;
#16454 = ORIENTED_EDGE ( 'NONE', *, *, #9919, .T. ) ;
#16455 = CARTESIAN_POINT ( 'NONE',  ( -3.175426480542816510, 5.499999999999865885, -116.8750000000000142 ) ) ;
#16456 = CARTESIAN_POINT ( 'NONE',  ( 20.81250000000017053, -2.649519052838178457, 1.097466725451499370 ) ) ;
#16457 = CARTESIAN_POINT ( 'NONE',  ( 5.412658773652712085, -3.125000000000086153, -132.9330127018922383 ) ) ;
#16458 = ORIENTED_EDGE ( 'NONE', *, *, #4726, .F. ) ;
#16459 = DIRECTION ( 'NONE',  ( 0.000000000000000000, -0.000000000000000000, -1.000000000000000000 ) ) ;
#16460 = CARTESIAN_POINT ( 'NONE',  ( 2.775557561562891351E-14, -6.250000000000061284, -166.8169872981077901 ) ) ;
#16461 = CARTESIAN_POINT ( 'NONE',  ( 106.9374999999997868, 2.500000000000055067, -1.035533905932568777 ) ) ;
#16462 = CARTESIAN_POINT ( 'NONE',  ( -1.000000000000000888, -9.000000000000007105, 4.000000000000003553 ) ) ;
#16463 = CARTESIAN_POINT ( 'NONE',  ( 4.293779821593954438, 3.976156217459086317, -180.0000000000000284 ) ) ;
#16464 = CARTESIAN_POINT ( 'NONE',  ( 5.999999999999897859, 1.607695154586893826, -133.5193375672974128 ) ) ;
#16465 = CARTESIAN_POINT ( 'NONE',  ( -4.763139720814407951, 2.749999999999946709, -179.7500000000000284 ) ) ;
#16466 = CARTESIAN_POINT ( 'NONE',  ( 110.0002832217622597, -1.308140751793585022, -1.308140751793640533 ) ) ;
#16467 = CARTESIAN_POINT ( 'NONE',  ( 3.608439182435180470, 6.249999999999982236, -177.5580127018922667 ) ) ;
#16468 = CARTESIAN_POINT ( 'NONE',  ( -0.3085845443850022130, -9.691415455614869501, -4.244941038143118739 ) ) ;
#16469 = EDGE_CURVE ( 'NONE', #29957, #6341, #8027, .T. ) ;
#16470 = CARTESIAN_POINT ( 'NONE',  ( -5.999999999999963585, 1.780251999655701777E-13, -104.9136751345948255 ) ) ;
#16471 = CARTESIAN_POINT ( 'NONE',  ( 138.8363248654052029, 0.000000000000000000, -5.500000000000005329 ) ) ;
#16472 = CARTESIAN_POINT ( 'NONE',  ( 0.000000000000000000, 5.499999999999991118, -120.0000000000000000 ) ) ;
#16473 = CARTESIAN_POINT ( 'NONE',  ( 135.0000000000000284, -8.265636665782029269, -8.005364441812183429 ) ) ;
#16474 = CARTESIAN_POINT ( 'NONE',  ( 153.8363248654052029, 0.000000000000000000, -5.500000000000005329 ) ) ;
#16475 = ORIENTED_EDGE ( 'NONE', *, *, #29029, .T. ) ;
#16476 = CARTESIAN_POINT ( 'NONE',  ( 20.81250000000014211, 1.097466725451679892, 2.649519052838298805 ) ) ;
#16477 = CARTESIAN_POINT ( 'NONE',  ( 0.9171503098353951389, -15.89765342390441916, 7.324020193813952417 ) ) ;
#16478 = DIRECTION ( 'NONE',  ( -1.000000000000000000, -1.665334536937731113E-16, 1.526556658859586792E-16 ) ) ;
#16479 = CARTESIAN_POINT ( 'NONE',  ( -5.999999999999963585, 8.134310703387671600E-14, -125.3363248654052171 ) ) ;
#16480 = ADVANCED_FACE ( 'NONE', ( #11045 ), #25609, .T. ) ;
#16481 = EDGE_CURVE ( 'NONE', #4074, #3881, #13323, .T. ) ;
#16482 = VERTEX_POINT ( 'NONE', #18112 ) ;
#16483 = LINE ( 'NONE', #7372, #18280 ) ;
#16484 = DIRECTION ( 'NONE',  ( 0.000000000000000000, -2.081668171172247091E-17, 1.000000000000000000 ) ) ;
#16485 = CIRCLE ( 'NONE', #3678, 10.00000000000001421 ) ;
#16486 = CARTESIAN_POINT ( 'NONE',  ( -7.216878364870328078, 0.000000000000000000, -108.6919872981078043 ) ) ;
#16487 =( BOUNDED_CURVE ( )  B_SPLINE_CURVE ( 2, ( #10652, #26446, #12818, #27048, #14807, #14951, #24152, #17570, #3095 ),
 .UNSPECIFIED., .F., .F. ) 
 B_SPLINE_CURVE_WITH_KNOTS ( ( 3, 2, 2, 2, 3 ),
 ( 0.8805555555555555358, 0.8814814814814815325, 0.8833333333333333037, 0.8851851851851851860, 0.8861111111111111827 ),
 .UNSPECIFIED. ) 
 CURVE ( )  GEOMETRIC_REPRESENTATION_ITEM ( )  RATIONAL_B_SPLINE_CURVE ( ( 0.9330127018922194093, 0.9330127018922154125, 1.000000000000000000, 0.8660254037844388186, 1.000000000000000000, 0.8660254037844388186, 1.000000000000000000, 0.9330127018922154125, 0.9330127018922194093 ) ) 
 REPRESENTATION_ITEM ( '' )  );
#16488 = CARTESIAN_POINT ( 'NONE',  ( -3.464101615137757051, -5.999999999999979572, -77.66367513459483973 ) ) ;
#16489 = CARTESIAN_POINT ( 'NONE',  ( 140.4300748654052029, 2.278174593051702335, -5.500000000000323297 ) ) ;
#16490 = ORIENTED_EDGE ( 'NONE', *, *, #22049, .T. ) ;
#16491 = ORIENTED_EDGE ( 'NONE', *, *, #18783, .F. ) ;
#16492 = CARTESIAN_POINT ( 'NONE',  ( 106.1636751345947260, 1.414213562373034527, -1.414213562373034527 ) ) ;
#16493 = CARTESIAN_POINT ( 'NONE',  ( 136.1250000000000284, 0.000000000000000000, -6.000000000000005329 ) ) ;
#16494 = ORIENTED_EDGE ( 'NONE', *, *, #24516, .F. ) ;
#16495 = CARTESIAN_POINT ( 'NONE',  ( -3.608439182435115633, 6.249999999999965361, -141.9419872981078186 ) ) ;
#16496 = CARTESIAN_POINT ( 'NONE',  ( 11.87500000000013500, -2.649519052838111843, 1.110223024625156540E-13 ) ) ;
#16497 = DIRECTION ( 'NONE',  ( 0.000000000000000000, -2.081668171172248016E-17, 1.000000000000000000 ) ) ;
#16498 = CARTESIAN_POINT ( 'NONE',  ( 17.75000000000015632, 1.110223024625156540E-13, -2.000000000000001776 ) ) ;
#16499 = CARTESIAN_POINT ( 'NONE',  ( 19.99999999999998934, -3.608224830031758756E-16, 6.500000000000016875 ) ) ;
#16500 = CARTESIAN_POINT ( 'NONE',  ( 1.000000000000000888, -16.43939393939394833, 5.999693900976793337 ) ) ;
#16501 = CARTESIAN_POINT ( 'NONE',  ( 2.775557561562891351E-14, -6.250000000000061284, -58.18301270189224539 ) ) ;
#16502 = CARTESIAN_POINT ( 'NONE',  ( 147.0788997308104342, -4.999999999999989342, 2.071067811865468400 ) ) ;
#16503 = DIRECTION ( 'NONE',  ( -1.000000000000000000, -1.665334536937736783E-16, -2.220446049250315546E-16 ) ) ;
#16504 = DIRECTION ( 'NONE',  ( 1.000000000000000000, -5.551115123125773458E-17, -1.260129944081490338E-35 ) ) ;
#16505 = DIRECTION ( 'NONE',  ( 1.000000000000000000, 0.000000000000000000, 0.000000000000000000 ) ) ;
#16506 = CIRCLE ( 'NONE', #21856, 0.5000000000000000000 ) ;
#16507 = CARTESIAN_POINT ( 'NONE',  ( 24.61237180318302364, -1.845499441024646803, 1.545370191226289602 ) ) ;
#16508 = DIRECTION ( 'NONE',  ( -1.000000000000000000, -1.665334536937731113E-16, 1.526556658859586792E-16 ) ) ;
#16509 = CARTESIAN_POINT ( 'NONE',  ( 111.1249999999999289, 1.767766952966320915, 1.767766952966431937 ) ) ;
#16510 = EDGE_CURVE ( 'NONE', #9807, #6115, #22590, .T. ) ;
#16511 = EDGE_CURVE ( 'NONE', #5195, #899, #3892, .T. ) ;
#16512 = SURFACE_STYLE_USAGE ( .BOTH. , #7093 ) ;
#16513 = CARTESIAN_POINT ( 'NONE',  ( -5.196152422706601826, 2.999999999999975131, -112.5386751345948113 ) ) ;
#16514 = ORIENTED_EDGE ( 'NONE', *, *, #2046, .F. ) ;
#16515 = CARTESIAN_POINT ( 'NONE',  ( -4.763139720814407951, -2.750000000000016431, -53.49999999999999289 ) ) ;
#16516 = EDGE_CURVE ( 'NONE', #3077, #9966, #18722, .T. ) ;
#16517 = CARTESIAN_POINT ( 'NONE',  ( 3.464101615137852974, 5.999999999999884537, -121.3363248654051603 ) ) ;
#16518 = CARTESIAN_POINT ( 'NONE',  ( 6.000000000000000888, -1.607695154586752384, -151.6533121635129930 ) ) ;
#16519 = B_SPLINE_CURVE_WITH_KNOTS ( 'NONE', 3,
 ( #10223, #26618, #19293, #10070, #14835, #21889, #28921, #524, #5124, #7444 ),
 .UNSPECIFIED., .F., .F.,
 ( 4, 2, 2, 2, 4 ),
 ( 6.138082936578478530E-16, 0.0005289548070271558140, 0.001057909614053697970, 0.001586864421080240450, 0.002115819228106782714 ),
 .UNSPECIFIED. ) ;
#16520 = AXIS2_PLACEMENT_3D ( 'NONE', #10272, #12304, #14459 ) ;
#16521 = ORIENTED_EDGE ( 'NONE', *, *, #9891, .F. ) ;
#16522 = CARTESIAN_POINT ( 'NONE',  ( 105.3124999999998437, -1.035533905932598975, 2.500000000000265121 ) ) ;
#16523 = CARTESIAN_POINT ( 'NONE',  ( 141.5625000000000284, -4.242640687119298093, 4.242640687119298093 ) ) ;
#16524 = CARTESIAN_POINT ( 'NONE',  ( 2.775557561562891351E-14, 6.250000000000033751, -103.0669872981078186 ) ) ;
#16525 = CYLINDRICAL_SURFACE ( 'NONE', #16622, 6.000000000000000888 ) ;
#16526 =( BOUNDED_CURVE ( )  B_SPLINE_CURVE ( 2, ( #1750, #11149, #6208, #15628, #1445, #1904, #24937, #15935, #4203 ),
 .UNSPECIFIED., .F., .T. ) 
 B_SPLINE_CURVE_WITH_KNOTS ( ( 3, 2, 2, 2, 3 ),
 ( 0.5527777777777778123, 0.5537037037037036979, 0.5555555555555555802, 0.5574074074074074625, 0.5583333333333333481 ),
 .UNSPECIFIED. ) 
 CURVE ( )  GEOMETRIC_REPRESENTATION_ITEM ( )  RATIONAL_B_SPLINE_CURVE ( ( 0.9330127018922194093, 0.9330127018922234061, 1.000000000000000000, 0.8660254037844388186, 1.000000000000000000, 0.8660254037844388186, 1.000000000000000000, 0.9330127018922194093, 0.9330127018922194093 ) ) 
 REPRESENTATION_ITEM ( '' )  );
#16527 = CARTESIAN_POINT ( 'NONE',  ( 159.5476497308104342, 0.000000000000000000, -5.000000000000004441 ) ) ;
#16528 = CARTESIAN_POINT ( 'NONE',  ( 116.9999999999999005, 2.500000000000057732, 1.110223024625156540E-13 ) ) ;
#16529 = CARTESIAN_POINT ( 'NONE',  ( 4.763139720814407951, -2.749999999999988454, -137.0000000000000000 ) ) ;
#16530 = ORIENTED_EDGE ( 'NONE', *, *, #3720, .T. ) ;
#16531 = ORIENTED_EDGE ( 'NONE', *, *, #9815, .F. ) ;
#16532 = CARTESIAN_POINT ( 'NONE',  ( 0.000000000000000000, 5.499999999999991118, -64.50000000000000000 ) ) ;
#16533 = CARTESIAN_POINT ( 'NONE',  ( 5.196152422706629359, -2.999999999999988898, -179.2886751345948539 ) ) ;
#16534 = CARTESIAN_POINT ( 'NONE',  ( 116.0000000000000142, 6.735557395310442023E-16, 5.500000000000000000 ) ) ;
#16535 = CARTESIAN_POINT ( 'NONE',  ( -5.412658773652739619, 3.124999999999975131, -84.18301270189220986 ) ) ;
#16536 = CARTESIAN_POINT ( 'NONE',  ( 154.9761751345948255, 3.889087296526011706, 3.889087296526011706 ) ) ;
#16537 = VECTOR ( 'NONE', #18102, 1000.000000000000000 ) ;
#16538 = CARTESIAN_POINT ( 'NONE',  ( 105.2497167782374845, -1.308140751793585022, -1.308140751793640533 ) ) ;
#16539 = CARTESIAN_POINT ( 'NONE',  ( -5.999999999999962697, 3.323446944526963891E-14, -160.4136751345948255 ) ) ;
#16540 = EDGE_CURVE ( 'NONE', #1653, #19367, #27491, .T. ) ;
#16541 = DIRECTION ( 'NONE',  ( -7.147005652999508048E-36, 5.642372883946980038E-36, 1.000000000000000000 ) ) ;
#16542 = CARTESIAN_POINT ( 'NONE',  ( 118.9377832217621460, -1.849990392679472073, -0.7662911109077087390 ) ) ;
#16543 = AXIS2_PLACEMENT_3D ( 'NONE', #3282, #12708, #12859 ) ;
#16544 = ADVANCED_FACE ( 'NONE', ( #13827 ), #23174, .T. ) ;
#16545 = CARTESIAN_POINT ( 'NONE',  ( -4.763139720814407951, 2.749999999999946709, -145.2500000000000000 ) ) ;
#16546 = FACE_OUTER_BOUND ( 'NONE', #29606, .T. ) ;
#16547 = CARTESIAN_POINT ( 'NONE',  ( 3.608439182435180470, -6.249999999999997335, -161.5580127018921814 ) ) ;
#16548 = CARTESIAN_POINT ( 'NONE',  ( 5.999999999999999112, 2.951592740943527306E-14, -148.5863248654052313 ) ) ;
#16549 = CARTESIAN_POINT ( 'NONE',  ( 0.000000000000000000, 0.000000000000000000, -180.0000000000000568 ) ) ;
#16550 = AXIS2_PLACEMENT_3D ( 'NONE', #22251, #22562, #11049 ) ;
#16551 = CARTESIAN_POINT ( 'NONE',  ( 6.350852961086080661, -9.614813431917819062E-14, -81.37500000000001421 ) ) ;
#16552 = CARTESIAN_POINT ( 'NONE',  ( 6.000000000000000888, -1.859271017917181981E-14, -63.08632486540521711 ) ) ;
#16553 = CARTESIAN_POINT ( 'NONE',  ( -4.763139720814407951, -2.750000000000016431, -64.00000000000000000 ) ) ;
#16554 = CARTESIAN_POINT ( 'NONE',  ( 155.9062500000000568, 6.000000000000005329, -2.485281374238556218 ) ) ;
#16555 =( NAMED_UNIT ( * ) SI_UNIT ( $, .STERADIAN. ) SOLID_ANGLE_UNIT ( ) );
#16556 = CARTESIAN_POINT ( 'NONE',  ( 17.50000000000007105, -1.999999999999835243, -5.551115123125782702E-14 ) ) ;
#16557 = CARTESIAN_POINT ( 'NONE',  ( 116.0000000000000142, 0.000000000000000000, 0.000000000000000000 ) ) ;
#16558 = AXIS2_PLACEMENT_3D ( 'NONE', #14825, #3255, #5713 ) ;
#16559 = CARTESIAN_POINT ( 'NONE',  ( 119.1247167782375698, -1.849990392679412565, 1.110223024625156540E-13 ) ) ;
#16560 = EDGE_LOOP ( 'NONE', ( #25449, #11811, #19008, #26573 ) ) ;
#16561 = CARTESIAN_POINT ( 'NONE',  ( 151.1250000000000284, 0.000000000000000000, -6.000000000000005329 ) ) ;
#16562 = LINE ( 'NONE', #24435, #26359 ) ;
#16563 = ORIENTED_EDGE ( 'NONE', *, *, #28029, .T. ) ;
#16564 = CARTESIAN_POINT ( 'NONE',  ( 22.56250000000011724, -1.999999999999851674, -0.8284271247462354770 ) ) ;
#16565 = CARTESIAN_POINT ( 'NONE',  ( -7.216878364870328078, 0.000000000000000000, -152.1919872981077901 ) ) ;
#16566 = ORIENTED_EDGE ( 'NONE', *, *, #10409, .T. ) ;
#16567 = CARTESIAN_POINT ( 'NONE',  ( -4.763139720814407951, 2.749999999999946709, -88.25000000000005684 ) ) ;
#16568 = CARTESIAN_POINT ( 'NONE',  ( 5.412658773652712085, -3.125000000000086153, -102.9330127018922525 ) ) ;
#16569 = CARTESIAN_POINT ( 'NONE',  ( 3.677985992802582871, 10.37237449091584374, -20.24368265486284457 ) ) ;
#16570 = CARTESIAN_POINT ( 'NONE',  ( 157.9538997308104058, -2.071067811865468400, -4.999999999999989342 ) ) ;
#16571 = CARTESIAN_POINT ( 'NONE',  ( -2.775557561562891351E-14, -5.500000000000115463, -167.2500000000000000 ) ) ;
#16572 = CARTESIAN_POINT ( 'NONE',  ( 159.1800748654052029, -2.278174593052116670, 5.499999999999908518 ) ) ;
#16573 = CARTESIAN_POINT ( 'NONE',  ( 6.000000000000000888, -1.859271017917181981E-14, -93.66367513459481131 ) ) ;
#16574 = AXIS2_PLACEMENT_3D ( 'NONE', #12096, #16408, #9302 ) ;
#16575 = VECTOR ( 'NONE', #22140, 1000.000000000000000 ) ;
#16576 = SURFACE_SIDE_STYLE ('',( #16282 ) ) ;
#16577 = EDGE_CURVE ( 'NONE', #2721, #30412, #11981, .T. ) ;
#16578 = CARTESIAN_POINT ( 'NONE',  ( -3.175426480542816066, -5.500000000000057732, -174.8750000000000284 ) ) ;
#16579 = CARTESIAN_POINT ( 'NONE',  ( 23.28867513459498184, 2.500000000000113243, -2.220446049250313081E-13 ) ) ;
#16580 = CARTESIAN_POINT ( 'NONE',  ( -3.175426480542816510, -5.500000000000057732, -152.3750000000000000 ) ) ;
#16581 = AXIS2_PLACEMENT_3D ( 'NONE', #17562, #10330, #24282 ) ;
#16582 = CARTESIAN_POINT ( 'NONE',  ( 110.4999999999999432, -2.499999999999891198, 3.330669073875469621E-13 ) ) ;
#16583 = CARTESIAN_POINT ( 'NONE',  ( 4.763139720814407951, 2.750000000000002665, -103.7500000000000142 ) ) ;
#16584 = CARTESIAN_POINT ( 'NONE',  ( -3.464101615137725076, 5.999999999999979572, -59.58632486540520290 ) ) ;
#16586 = CARTESIAN_POINT ( 'NONE',  ( 4.763139720814407951, -2.749999999999988454, -92.00000000000002842 ) ) ;
#16585 = CARTESIAN_POINT ( 'NONE',  ( 3.175426480543072749, -5.500000000000105693, -156.6250000000000000 ) ) ;
#16587 = CARTESIAN_POINT ( 'NONE',  ( 13.89882486540516915, 1.035533905932809473, 2.499999999999964473 ) ) ;
#16588 = CARTESIAN_POINT ( 'NONE',  ( 6.000000000000000888, -1.607695154586752384, -135.7306624327025872 ) ) ;
#16589 = CIRCLE ( 'NONE', #29776, 0.5000000000000006661 ) ;
#16590 = ORIENTED_EDGE ( 'NONE', *, *, #21028, .F. ) ;
#16591 = CARTESIAN_POINT ( 'NONE',  ( 112.1874999999998295, 1.035533905932719101, 2.500000000000205169 ) ) ;
#16592 = CARTESIAN_POINT ( 'NONE',  ( -5.999999999999963585, -1.487416814333745711E-14, -66.83632486540523132 ) ) ;
#16593 = CARTESIAN_POINT ( 'NONE',  ( 108.4377832217621318, 1.849990392679532247, 0.7662911109080692285 ) ) ;
#16594 = CARTESIAN_POINT ( 'NONE',  ( 6.000000000000000888, 1.743066579297358182E-13, -85.58632486540523132 ) ) ;
#16595 = ORIENTED_EDGE ( 'NONE', *, *, #4699, .T. ) ;
#16596 = CARTESIAN_POINT ( 'NONE',  ( 15.39882486540520823, -1.035533905932568999, -2.500000000000024425 ) ) ;
#16597 = LINE ( 'NONE', #14297, #1524 ) ;
#16598 = CARTESIAN_POINT ( 'NONE',  ( 105.8747167782375271, -2.775557561562891351E-14, 1.849990392679523588 ) ) ;
#16599 = CARTESIAN_POINT ( 'NONE',  ( -5.999999999999963585, 8.134310703387671600E-14, -141.8363248654052029 ) ) ;
#16600 = ORIENTED_EDGE ( 'NONE', *, *, #25087, .F. ) ;
#16601 = CARTESIAN_POINT ( 'NONE',  ( 150.0937500000000284, 6.000000000000005329, 2.485281374238585972 ) ) ;
#16602 = EDGE_LOOP ( 'NONE', ( #12728, #10674, #27442, #29368 ) ) ;
#16603 = EDGE_CURVE ( 'NONE', #20340, #22119, #7058, .T. ) ;
#16604 = CARTESIAN_POINT ( 'NONE',  ( -3.175426480542816510, 5.499999999999865885, -112.3750000000000426 ) ) ;
#16605 = CARTESIAN_POINT ( 'NONE',  ( 22.62500000000011724, 5.551115123125782702E-14, 2.649519052838333888 ) ) ;
#16606 =( BOUNDED_CURVE ( )  B_SPLINE_CURVE ( 2, ( #6369, #23299, #20990, #18693, #6988, #16407, #11170, #8694, #20518 ),
 .UNSPECIFIED., .F., .F. ) 
 B_SPLINE_CURVE_WITH_KNOTS ( ( 3, 2, 2, 2, 3 ),
 ( 0.2124999999999988010, 0.2187499999999990008, 0.2249999999999992006, 0.2312499999999994282, 0.2374999999999997391 ),
 .UNSPECIFIED. ) 
 CURVE ( )  GEOMETRIC_REPRESENTATION_ITEM ( )  RATIONAL_B_SPLINE_CURVE ( ( 1.000000000000014877, 0.9238795325112718615, 1.000000000000000000, 0.9238795325112867385, 1.000000000000000000, 0.9238795325112867385, 1.000000000000000000, 0.9238795325112904022, 0.9999999999999963363 ) ) 
 REPRESENTATION_ITEM ( '' )  );
#16607 = CARTESIAN_POINT ( 'NONE',  ( 2.775557561562891351E-14, 6.250000000000033751, -130.9330127018922383 ) ) ;
#16608 = ORIENTED_EDGE ( 'NONE', *, *, #17566, .F. ) ;
#16609 = FACE_OUTER_BOUND ( 'NONE', #3615, .T. ) ;
#16610 = CARTESIAN_POINT ( 'NONE',  ( 2.775557561562891351E-14, -6.250000000000061284, -169.8169872981077901 ) ) ;
#16611 = CARTESIAN_POINT ( 'NONE',  ( 106.8749999999998437, 1.767766952966320915, -1.767766952966320915 ) ) ;
#16612 = AXIS2_PLACEMENT_3D ( 'NONE', #7946, #27135, #1913 ) ;
#16613 = ORIENTED_EDGE ( 'NONE', *, *, #1051, .F. ) ;
#16614 =( BOUNDED_SURFACE ( )  B_SPLINE_SURFACE ( 1, 2, ( 
 ( #25133, #6720, #2119, #30367, #18418, #18269, #21169, #16135, #18574, #27895, #18876, #111, #11522, #30059, #28198, #6868, #4098, #25441, #16291, #13521, #21018, #30214, #16438, #25763, #9493, #4709, #25611, #15980, #8882, #15834, #14142, #22861, #1798, #11204, #20550, #29902, #4564, #9029, #1960, #13830, #27581, #13990, #4251, #20864, #9177, #13673, #19317, #28639, #21472, #7173, #14711, #21314, #12277, #12420, #23913, #708, #26490, #19465, #26349, #21620, #14435, #23627, #257, #16733, #25909, #26200, #7610, #14285, #14566, #2560, #11984, #19032, #5298, #28349, #7325, #26057, #2702, #400, #19167, #28501, #16880, #5151, #15000, #24949, #24651, #3902, #20222, #22365, #3598, #7908, #22671, #29093, #13027, #29572, #17322, #8053, #6069, #8527, #26638, #17783, #26943, #12872, #5598, #24340, #17932, #8373, #10545, #22211, #27249, #15639, #15160, #26782, #24492, #19902, #1300, #3295, #1614, #12722, #10713, #3439, #3757, #19747, #29243, #8206, #17622, #20057, #15482, #11639, #13793, #30332, #27860, #20510, #16400, #6523, #18083, #13952, #25569, #13481, #20985, #25725, #1762, #11163, #27398, #6827, #15945, #22980, #22821, #4058, #9295, #25245, #8688, #6363, #25102, #4216, #2237, #4527, #11326, #20672, #30025, #18383, #16103, #16253, #2083, #25405, #11487, #24021, #16698, #2965, #364, #14827, #21581, #513, #19434, #16843, #24171, #26019, #12387, #9907, #28759, #19283, #11791, #14402, #14676, #23735, #28463, #21733, #69, #217, #26165, #9753, #12243, #5115, #26460, #5416, #7294, #672, #10058, #21132, #14535, #28163, #7133, #11951, #21277, #23875, #14249, #4824, #7575, #23587, #2524, #9603, #18993, #2820, #28604, #6302, #29949, #20300, #22021, #29646, #6156, #817, #7876, #17290, #16032, #3113, #20440, #19575, #8461, #11095, #24887, #8612, #18020, #12536, #27477, #22607, #6453, #6610, #22905, #13266, #22756, #24308, #20601, #14968, #18163, #15881, #29495, #1848, #27632, #11251, #25180, #20148, #13410, #21879, #10947, #957, #15572, #5565, #10213, #1697, #17868, #27337, #4144, #28910, #10358, #15724, #1542, #3988, #25033, #8928, #26610, #27185, #13567, #18319, #3257, #29799, #12688, #3838, #8776, #4305, #23065, #25330, #13724, #2006, #11415, #10295, #12188, #15061, #12775, #24108, #17228, #10449, #764, #2908, #10149, #17076, #21529, #19220, #28551, #26840, #14486, #898, #454, #19373, #21965, #5357, #19521, #28853, #23820, #7966, #3056, #17374, #17526, #3346, #12479, #3197, #5207, #1057, #26256, #28999, #26690, #9997, #22116 ),
 ( #9842, #12622, #24249, #14621, #19803, #609, #7519, #5653, #19660, #16930, #24405, #29148, #23971, #12328, #21674, #8106, #28695, #7667, #26405, #14765, #2760, #21818, #7812, #26553, #5499, #14909, #18131, #11063, #15851, #29459, #27446, #22420, #15383, #3956, #8583, #13088, #5802, #6417, #10768, #25151, #27155, #8896, #15692, #25002, #13535, #10921, #18287, #20116, #4113, #13382, #22875, #22725, #15218, #8431, #20408, #1358, #3500, #29769, #8746, #29308, #1815, #11221, #17677, #27000, #12930, #1668, #17838, #6125, #8263, #19955, #20569, #24708, #29919, #24550, #22267, #1196, #10602, #5963, #3652, #15540, #24858, #3806, #13235, #22579, #17987, #1509, #20272, #29618, #27303, #6272, #18586, #273, #7040, #16453, #4871, #2288, #9655, #2135, #9510, #25779, #14302, #4727, #27598, #11535, #2436, #20876, #4578, #125, #16000, #16150, #11693, #25630, #28064, #14004, #23642, #21331, #23190, #28217, #21185, #6577, #23346, #18897, #25300, #27754, #6731, #30383, #30075, #16601, #23493, #11382, #11848, #4271, #7191, #25924, #6881, #9351, #2575, #21038, #25456, #18743, #30230, #13692, #1975, #20726, #23031, #9044, #14156, #18434, #9193, #11997, #27906, #4422, #13850, #16307, #21926, #26365, #858, #1008, #7922, #5314, #24210, #9801, #15019, #413, #3159, #28961, #14578, #24361, #19046, #3309, #14446, #2867, #23780, #2714, #21779, #26211, #722, #21487, #12142, #12288, #10106, #1399, #18331, #8623, #29509, #13275, #3693, #29346, #29811, #11105, #10808, #27644, #17879, #8308, #25191, #6466, #24754, #22918, #6622, #13125, #22463, #17717, #18176, #27195, #24896, #20159, #15425, #1859, #8471, #16044, #11264, #25342, #4316, #13578, #15892, #20614, #3845, #29960, #6171, #15583, #8789, #4001, #22618, #1237, #8941, #1555, #13734, #10961, #10645, #20452, #27488, #19994, #6310, #27041, #20310, #6008, #4155, #29656, #18032, #27348, #15733, #25043, #13420, #22765, #1708, #11427, #11576, #7079, #21074, #23531, #9389, #311, #16789, #18626, #23679, #16642, #5055, #18782, #14339, #23079, #23234, #2175, #25819, #25502, #12033, #18939, #6774, #28257, #20772, #2615, #21374, #2330, #4767, #19082, #28104, #20922, #16493, #25666, #30119, #27798, #16193, #2019, #9083, #9547, #18478, #27947, #167, #14045, #14194, #2473, #4468, #25963, #11731, #4911, #26111, #9699, #4, #11889, #13894, #28404, #30271, #7234, #7382, #6921, #9233, #16346, #4615, #23383, #21225, #5356, #21528, #26255, #7811, #23970, #9841, #21817, #12478, #16929, #10148, #17227, #5206 ) ),
 .UNSPECIFIED., .F., .F., .T. ) 
 B_SPLINE_SURFACE_WITH_KNOTS ( ( 2, 2 ),
 ( 3, 2, 2, 2, 2, 2, 2, 2, 2, 2, 2, 2, 2, 2, 2, 2, 2, 2, 2, 2, 2, 2, 2, 2, 2, 2, 2, 2, 2, 2, 2, 2, 2, 2, 2, 2, 2, 2, 2, 2, 2, 2, 2, 2, 2, 2, 2, 2, 2, 2, 2, 2, 2, 2, 2, 2, 2, 2, 2, 2, 2, 2, 2, 2, 2, 2, 2, 2, 2, 2, 2, 2, 2, 2, 2, 2, 2, 2, 2, 2, 2, 2, 2, 2, 2, 2, 2, 2, 2, 2, 2, 2, 2, 2, 2, 2, 2, 2, 2, 2, 2, 2, 2, 2, 2, 2, 2, 2, 2, 2, 2, 2, 2, 2, 2, 2, 2, 2, 2, 2, 2, 2, 2, 2, 2, 2, 2, 2, 2, 2, 2, 2, 2, 2, 2, 2, 2, 2, 2, 2, 2, 2, 2, 2, 2, 2, 2, 2, 2, 2, 2, 2, 2, 2, 2, 2, 2, 2, 2, 2, 3 ),
 ( 0.000000000000000000, 1.000000000000000000 ),
 ( 0.000000000000000000, 0.006250000000000000347, 0.01250000000000000069, 0.01874999999999999931, 0.02500000000000000139, 0.03125000000000000000, 0.03749999999999999861, 0.04374999999999999722, 0.05000000000000000278, 0.05625000000000000139, 0.06250000000000000000, 0.06875000000000000555, 0.07499999999999999722, 0.08125000000000000278, 0.08749999999999999445, 0.09375000000000000000, 0.1000000000000000056, 0.1062499999999999972, 0.1125000000000000028, 0.1187499999999999944, 0.1250000000000000000, 0.1312500000000000056, 0.1375000000000000111, 0.1437499999999999889, 0.1499999999999999944, 0.1562500000000000000, 0.1625000000000000056, 0.1687500000000000111, 0.1749999999999999889, 0.1812499999999999944, 0.1875000000000000000, 0.1937500000000000056, 0.2000000000000000111, 0.2062499999999999889, 0.2124999999999999944, 0.2187500000000000000, 0.2250000000000000056, 0.2312500000000000111, 0.2374999999999999889, 0.2437499999999999944, 0.2500000000000000000, 0.2562499999999999778, 0.2625000000000000111, 0.2687499999999999889, 0.2750000000000000222, 0.2812500000000000000, 0.2874999999999999778, 0.2937500000000000111, 0.2999999999999999889, 0.3062500000000000222, 0.3125000000000000000, 0.3187499999999999778, 0.3250000000000000111, 0.3312499999999999889, 0.3375000000000000222, 0.3437500000000000000, 0.3499999999999999778, 0.3562500000000000111, 0.3624999999999999889, 0.3687500000000000222, 0.3750000000000000000, 0.3812499999999999778, 0.3875000000000000111, 0.3937499999999999889, 0.4000000000000000222, 0.4062500000000000000, 0.4124999999999999778, 0.4187500000000000111, 0.4249999999999999889, 0.4312500000000000222, 0.4375000000000000000, 0.4437499999999999778, 0.4500000000000000111, 0.4562499999999999889, 0.4625000000000000222, 0.4687500000000000000, 0.4749999999999999778, 0.4812500000000000111, 0.4874999999999999889, 0.4937500000000000222, 0.5000000000000000000, 0.5062499999999999778, 0.5124999999999999556, 0.5187500000000000444, 0.5250000000000000222, 0.5312500000000000000, 0.5374999999999999778, 0.5437499999999999556, 0.5500000000000000444, 0.5562500000000000222, 0.5625000000000000000, 0.5687499999999999778, 0.5749999999999999556, 0.5812500000000000444, 0.5875000000000000222, 0.5937500000000000000, 0.5999999999999999778, 0.6062499999999999556, 0.6125000000000000444, 0.6187500000000000222, 0.6250000000000000000, 0.6312499999999999778, 0.6374999999999999556, 0.6437500000000000444, 0.6500000000000000222, 0.6562500000000000000, 0.6624999999999999778, 0.6687499999999999556, 0.6750000000000000444, 0.6812500000000000222, 0.6875000000000000000, 0.6937499999999999778, 0.6999999999999999556, 0.7062500000000000444, 0.7125000000000000222, 0.7187500000000000000, 0.7249999999999999778, 0.7312499999999999556, 0.7375000000000000444, 0.7437500000000000222, 0.7500000000000000000, 0.7562499999999999778, 0.7624999999999999556, 0.7687500000000000444, 0.7750000000000000222, 0.7812500000000000000, 0.7874999999999999778, 0.7937499999999999556, 0.8000000000000000444, 0.8062500000000000222, 0.8125000000000000000, 0.8187499999999999778, 0.8249999999999999556, 0.8312500000000000444, 0.8375000000000000222, 0.8437500000000000000, 0.8499999999999999778, 0.8562499999999999556, 0.8625000000000000444, 0.8687500000000000222, 0.8750000000000000000, 0.8812499999999999778, 0.8874999999999999556, 0.8937500000000000444, 0.9000000000000000222, 0.9062500000000000000, 0.9124999999999999778, 0.9187499999999999556, 0.9250000000000000444, 0.9312500000000000222, 0.9375000000000000000, 0.9437499999999999778, 0.9499999999999999556, 0.9562500000000000444, 0.9625000000000000222, 0.9687500000000000000, 0.9749999999999999778, 0.9812499999999999556, 0.9875000000000000444, 0.9937500000000000222, 1.000000000000000000 ),
 .UNSPECIFIED. ) 
 GEOMETRIC_REPRESENTATION_ITEM ( )  RATIONAL_B_SPLINE_SURFACE ( (
 ( 1.000000000000000000, 0.9238795325112867385, 1.000000000000000000, 0.9238795325112867385, 1.000000000000000000, 0.9238795325112867385, 1.000000000000000000, 0.9238795325112867385, 1.000000000000000000, 0.9238795325112867385, 1.000000000000000000, 0.9238795325112867385, 1.000000000000000000, 0.9238795325112867385, 1.000000000000000000, 0.9238795325112867385, 1.000000000000000000, 0.9238795325112867385, 1.000000000000000000, 0.9238795325112867385, 1.000000000000000000, 0.9238795325112867385, 1.000000000000000000, 0.9238795325112867385, 1.000000000000000000, 0.9238795325112867385, 1.000000000000000000, 0.9238795325112867385, 1.000000000000000000, 0.9238795325112867385, 1.000000000000000000, 0.9238795325112867385, 1.000000000000000000, 0.9238795325112867385, 1.000000000000000000, 0.9238795325112867385, 1.000000000000000000, 0.9238795325112867385, 1.000000000000000000, 0.9238795325112867385, 1.000000000000000000, 0.9238795325112867385, 1.000000000000000000, 0.9238795325112867385, 1.000000000000000000, 0.9238795325112867385, 1.000000000000000000, 0.9238795325112867385, 1.000000000000000000, 0.9238795325112867385, 1.000000000000000000, 0.9238795325112867385, 1.000000000000000000, 0.9238795325112867385, 1.000000000000000000, 0.9238795325112867385, 1.000000000000000000, 0.9238795325112867385, 1.000000000000000000, 0.9238795325112867385, 1.000000000000000000, 0.9238795325112867385, 1.000000000000000000, 0.9238795325112867385, 1.000000000000000000, 0.9238795325112867385, 1.000000000000000000, 0.9238795325112867385, 1.000000000000000000, 0.9238795325112867385, 1.000000000000000000, 0.9238795325112867385, 1.000000000000000000, 0.9238795325112867385, 1.000000000000000000, 0.9238795325112867385, 1.000000000000000000, 0.9238795325112867385, 1.000000000000000000, 0.9238795325112867385, 1.000000000000000000, 0.9238795325112867385, 1.000000000000000000, 0.9238795325112867385, 1.000000000000000000, 0.9238795325112867385, 1.000000000000000000, 0.9238795325112867385, 1.000000000000000000, 0.9238795325112867385, 1.000000000000000000, 0.9238795325112867385, 1.000000000000000000, 0.9238795325112867385, 1.000000000000000000, 0.9238795325112867385, 1.000000000000000000, 0.9238795325112867385, 1.000000000000000000, 0.9238795325112867385, 1.000000000000000000, 0.9238795325112867385, 1.000000000000000000, 0.9238795325112867385, 1.000000000000000000, 0.9238795325112867385, 1.000000000000000000, 0.9238795325112867385, 1.000000000000000000, 0.9238795325112867385, 1.000000000000000000, 0.9238795325112867385, 1.000000000000000000, 0.9238795325112867385, 1.000000000000000000, 0.9238795325112867385, 1.000000000000000000, 0.9238795325112867385, 1.000000000000000000, 0.9238795325112867385, 1.000000000000000000, 0.9238795325112867385, 1.000000000000000000, 0.9238795325112867385, 1.000000000000000000, 0.9238795325112867385, 1.000000000000000000, 0.9238795325112867385, 1.000000000000000000, 0.9238795325112867385, 1.000000000000000000, 0.9238795325112867385, 1.000000000000000000, 0.9238795325112867385, 1.000000000000000000, 0.9238795325112867385, 1.000000000000000000, 0.9238795325112867385, 1.000000000000000000, 0.9238795325112867385, 1.000000000000000000, 0.9238795325112867385, 1.000000000000000000, 0.9238795325112867385, 1.000000000000000000, 0.9238795325112867385, 1.000000000000000000, 0.9238795325112867385, 1.000000000000000000, 0.9238795325112867385, 1.000000000000000000, 0.9238795325112867385, 1.000000000000000000, 0.9238795325112867385, 1.000000000000000000, 0.9238795325112867385, 1.000000000000000000, 0.9238795325112867385, 1.000000000000000000, 0.9238795325112867385, 1.000000000000000000, 0.9238795325112867385, 1.000000000000000000, 0.9238795325112867385, 1.000000000000000000, 0.9238795325112867385, 1.000000000000000000, 0.9238795325112867385, 1.000000000000000000, 0.9238795325112867385, 1.000000000000000000, 0.9238795325112867385, 1.000000000000000000, 0.9238795325112867385, 1.000000000000000000, 0.9238795325112867385, 1.000000000000000000, 0.9238795325112867385, 1.000000000000000000, 0.9238795325112867385, 1.000000000000000000, 0.9238795325112867385, 1.000000000000000000, 0.9238795325112867385, 1.000000000000000000, 0.9238795325112867385, 1.000000000000000000, 0.9238795325112867385, 1.000000000000000000, 0.9238795325112867385, 1.000000000000000000, 0.9238795325112867385, 1.000000000000000000, 0.9238795325112867385, 1.000000000000000000, 0.9238795325112867385, 1.000000000000000000, 0.9238795325112867385, 1.000000000000000000, 0.9238795325112867385, 1.000000000000000000, 0.9238795325112867385, 1.000000000000000000, 0.9238795325112867385, 1.000000000000000000, 0.9238795325112867385, 1.000000000000000000, 0.9238795325112867385, 1.000000000000000000, 0.9238795325112867385, 1.000000000000000000, 0.9238795325112867385, 1.000000000000000000, 0.9238795325112867385, 1.000000000000000000, 0.9238795325112867385, 1.000000000000000000, 0.9238795325112867385, 1.000000000000000000, 0.9238795325112867385, 1.000000000000000000, 0.9238795325112867385, 1.000000000000000000, 0.9238795325112867385, 1.000000000000000000, 0.9238795325112867385, 1.000000000000000000, 0.9238795325112867385, 1.000000000000000000, 0.9238795325112867385, 1.000000000000000000, 0.9238795325112867385, 1.000000000000000000, 0.9238795325112867385, 1.000000000000000000, 0.9238795325112867385, 1.000000000000000000, 0.9238795325112867385, 1.000000000000000000, 0.9238795325112867385, 1.000000000000000000, 0.9238795325112867385, 1.000000000000000000, 0.9238795325112867385, 1.000000000000000000, 0.9238795325112867385, 1.000000000000000000, 0.9238795325112867385, 1.000000000000000000, 0.9238795325112867385, 1.000000000000000000, 0.9238795325112867385, 1.000000000000000000, 0.9238795325112867385, 1.000000000000000000, 0.9238795325112867385, 1.000000000000000000, 0.9238795325112867385, 1.000000000000000000, 0.9238795325112867385, 1.000000000000000000, 0.9238795325112867385, 1.000000000000000000, 0.9238795325112867385, 1.000000000000000000, 0.9238795325112867385, 1.000000000000000000, 0.9238795325112867385, 1.000000000000000000, 0.9238795325112867385, 1.000000000000000000, 0.9238795325112867385, 1.000000000000000000, 0.9238795325112867385, 1.000000000000000000, 0.9238795325112867385, 1.000000000000000000, 0.9238795325112867385, 1.000000000000000000, 0.9238795325112867385, 1.000000000000000000, 0.9238795325112867385, 1.000000000000000000, 0.9238795325112867385, 1.000000000000000000, 0.9238795325112867385, 1.000000000000000000, 0.9238795325112867385, 1.000000000000000000, 0.9238795325112867385, 1.000000000000000000, 0.9238795325112867385, 1.000000000000000000, 0.9238795325112867385, 1.000000000000000000, 0.9238795325112867385, 1.000000000000000000, 0.9238795325112867385, 1.000000000000000000, 0.9238795325112867385, 1.000000000000000000, 0.9238795325112867385, 1.000000000000000000, 0.9238795325112867385, 1.000000000000000000, 0.9238795325112867385, 1.000000000000000000, 0.9238795325112867385, 1.000000000000000000, 0.9238795325112867385, 1.000000000000000000, 0.9238795325112867385, 1.000000000000000000, 0.9238795325112867385, 1.000000000000000000, 0.9238795325112867385, 1.000000000000000000, 0.9238795325112867385, 1.000000000000000000, 0.9238795325112867385, 1.000000000000000000),
 ( 1.000000000000000000, 0.9238795325112867385, 1.000000000000000000, 0.9238795325112867385, 1.000000000000000000, 0.9238795325112867385, 1.000000000000000000, 0.9238795325112867385, 1.000000000000000000, 0.9238795325112867385, 1.000000000000000000, 0.9238795325112867385, 1.000000000000000000, 0.9238795325112867385, 1.000000000000000000, 0.9238795325112867385, 1.000000000000000000, 0.9238795325112867385, 1.000000000000000000, 0.9238795325112867385, 1.000000000000000000, 0.9238795325112867385, 1.000000000000000000, 0.9238795325112867385, 1.000000000000000000, 0.9238795325112867385, 1.000000000000000000, 0.9238795325112867385, 1.000000000000000000, 0.9238795325112867385, 1.000000000000000000, 0.9238795325112867385, 1.000000000000000000, 0.9238795325112867385, 1.000000000000000000, 0.9238795325112867385, 1.000000000000000000, 0.9238795325112867385, 1.000000000000000000, 0.9238795325112867385, 1.000000000000000000, 0.9238795325112867385, 1.000000000000000000, 0.9238795325112867385, 1.000000000000000000, 0.9238795325112867385, 1.000000000000000000, 0.9238795325112867385, 1.000000000000000000, 0.9238795325112867385, 1.000000000000000000, 0.9238795325112867385, 1.000000000000000000, 0.9238795325112867385, 1.000000000000000000, 0.9238795325112867385, 1.000000000000000000, 0.9238795325112867385, 1.000000000000000000, 0.9238795325112867385, 1.000000000000000000, 0.9238795325112867385, 1.000000000000000000, 0.9238795325112867385, 1.000000000000000000, 0.9238795325112867385, 1.000000000000000000, 0.9238795325112867385, 1.000000000000000000, 0.9238795325112867385, 1.000000000000000000, 0.9238795325112867385, 1.000000000000000000, 0.9238795325112867385, 1.000000000000000000, 0.9238795325112867385, 1.000000000000000000, 0.9238795325112867385, 1.000000000000000000, 0.9238795325112867385, 1.000000000000000000, 0.9238795325112867385, 1.000000000000000000, 0.9238795325112867385, 1.000000000000000000, 0.9238795325112867385, 1.000000000000000000, 0.9238795325112867385, 1.000000000000000000, 0.9238795325112867385, 1.000000000000000000, 0.9238795325112867385, 1.000000000000000000, 0.9238795325112867385, 1.000000000000000000, 0.9238795325112867385, 1.000000000000000000, 0.9238795325112867385, 1.000000000000000000, 0.9238795325112867385, 1.000000000000000000, 0.9238795325112867385, 1.000000000000000000, 0.9238795325112867385, 1.000000000000000000, 0.9238795325112867385, 1.000000000000000000, 0.9238795325112867385, 1.000000000000000000, 0.9238795325112867385, 1.000000000000000000, 0.9238795325112867385, 1.000000000000000000, 0.9238795325112867385, 1.000000000000000000, 0.9238795325112867385, 1.000000000000000000, 0.9238795325112867385, 1.000000000000000000, 0.9238795325112867385, 1.000000000000000000, 0.9238795325112867385, 1.000000000000000000, 0.9238795325112867385, 1.000000000000000000, 0.9238795325112867385, 1.000000000000000000, 0.9238795325112867385, 1.000000000000000000, 0.9238795325112867385, 1.000000000000000000, 0.9238795325112867385, 1.000000000000000000, 0.9238795325112867385, 1.000000000000000000, 0.9238795325112867385, 1.000000000000000000, 0.9238795325112867385, 1.000000000000000000, 0.9238795325112867385, 1.000000000000000000, 0.9238795325112867385, 1.000000000000000000, 0.9238795325112867385, 1.000000000000000000, 0.9238795325112867385, 1.000000000000000000, 0.9238795325112867385, 1.000000000000000000, 0.9238795325112867385, 1.000000000000000000, 0.9238795325112867385, 1.000000000000000000, 0.9238795325112867385, 1.000000000000000000, 0.9238795325112867385, 1.000000000000000000, 0.9238795325112867385, 1.000000000000000000, 0.9238795325112867385, 1.000000000000000000, 0.9238795325112867385, 1.000000000000000000, 0.9238795325112867385, 1.000000000000000000, 0.9238795325112867385, 1.000000000000000000, 0.9238795325112867385, 1.000000000000000000, 0.9238795325112867385, 1.000000000000000000, 0.9238795325112867385, 1.000000000000000000, 0.9238795325112867385, 1.000000000000000000, 0.9238795325112867385, 1.000000000000000000, 0.9238795325112867385, 1.000000000000000000, 0.9238795325112867385, 1.000000000000000000, 0.9238795325112867385, 1.000000000000000000, 0.9238795325112867385, 1.000000000000000000, 0.9238795325112867385, 1.000000000000000000, 0.9238795325112867385, 1.000000000000000000, 0.9238795325112867385, 1.000000000000000000, 0.9238795325112867385, 1.000000000000000000, 0.9238795325112867385, 1.000000000000000000, 0.9238795325112867385, 1.000000000000000000, 0.9238795325112867385, 1.000000000000000000, 0.9238795325112867385, 1.000000000000000000, 0.9238795325112867385, 1.000000000000000000, 0.9238795325112867385, 1.000000000000000000, 0.9238795325112867385, 1.000000000000000000, 0.9238795325112867385, 1.000000000000000000, 0.9238795325112867385, 1.000000000000000000, 0.9238795325112867385, 1.000000000000000000, 0.9238795325112867385, 1.000000000000000000, 0.9238795325112867385, 1.000000000000000000, 0.9238795325112867385, 1.000000000000000000, 0.9238795325112867385, 1.000000000000000000, 0.9238795325112867385, 1.000000000000000000, 0.9238795325112867385, 1.000000000000000000, 0.9238795325112867385, 1.000000000000000000, 0.9238795325112867385, 1.000000000000000000, 0.9238795325112867385, 1.000000000000000000, 0.9238795325112867385, 1.000000000000000000, 0.9238795325112867385, 1.000000000000000000, 0.9238795325112867385, 1.000000000000000000, 0.9238795325112867385, 1.000000000000000000, 0.9238795325112867385, 1.000000000000000000, 0.9238795325112867385, 1.000000000000000000, 0.9238795325112867385, 1.000000000000000000, 0.9238795325112867385, 1.000000000000000000, 0.9238795325112867385, 1.000000000000000000, 0.9238795325112867385, 1.000000000000000000, 0.9238795325112867385, 1.000000000000000000, 0.9238795325112867385, 1.000000000000000000, 0.9238795325112867385, 1.000000000000000000, 0.9238795325112867385, 1.000000000000000000, 0.9238795325112867385, 1.000000000000000000, 0.9238795325112867385, 1.000000000000000000, 0.9238795325112867385, 1.000000000000000000, 0.9238795325112867385, 1.000000000000000000, 0.9238795325112867385, 1.000000000000000000, 0.9238795325112867385, 1.000000000000000000, 0.9238795325112867385, 1.000000000000000000, 0.9238795325112867385, 1.000000000000000000, 0.9238795325112867385, 1.000000000000000000, 0.9238795325112867385, 1.000000000000000000, 0.9238795325112867385, 1.000000000000000000, 0.9238795325112867385, 1.000000000000000000, 0.9238795325112867385, 1.000000000000000000, 0.9238795325112867385, 1.000000000000000000, 0.9238795325112867385, 1.000000000000000000, 0.9238795325112867385, 1.000000000000000000, 0.9238795325112867385, 1.000000000000000000, 0.9238795325112867385, 1.000000000000000000, 0.9238795325112867385, 1.000000000000000000, 0.9238795325112867385, 1.000000000000000000, 0.9238795325112867385, 1.000000000000000000, 0.9238795325112867385, 1.000000000000000000, 0.9238795325112867385, 1.000000000000000000, 0.9238795325112867385, 1.000000000000000000, 0.9238795325112867385, 1.000000000000000000, 0.9238795325112867385, 1.000000000000000000, 0.9238795325112867385, 1.000000000000000000, 0.9238795325112867385, 1.000000000000000000, 0.9238795325112867385, 1.000000000000000000, 0.9238795325112867385, 1.000000000000000000, 0.9238795325112867385, 1.000000000000000000) ) ) 
 REPRESENTATION_ITEM ( '' )  SURFACE ( )  );
#16615 = CARTESIAN_POINT ( 'NONE',  ( 109.7886751345948255, -2.000000000000001776, 0.000000000000000000 ) ) ;
#16616 = CARTESIAN_POINT ( 'NONE',  ( -6.350852961085760029, -1.281975124255709124E-13, -181.1249999999999716 ) ) ;
#16617 = CARTESIAN_POINT ( 'NONE',  ( 107.1252832217622455, 0.000000000000000000, -1.849990392679523588 ) ) ;
#16618 = CARTESIAN_POINT ( 'NONE',  ( -5.412658773652739619, 3.124999999999975131, -174.1830127018922383 ) ) ;
#16619 = CARTESIAN_POINT ( 'NONE',  ( -4.996003610813206404E-16, -1.249000902703301601E-16, 6.000000000000001776 ) ) ;
#16620 = CARTESIAN_POINT ( 'NONE',  ( -20.99999999999998224, -25.00000000000010658, -5.000000000000004441 ) ) ;
#16621 = AXIS2_PLACEMENT_3D ( 'NONE', #9281, #4047, #20818 ) ;
#16622 = AXIS2_PLACEMENT_3D ( 'NONE', #23109, #20804, #28137 ) ;
#16623 = CARTESIAN_POINT ( 'NONE',  ( -3.464101615137757051, -5.999999999999979572, -53.66367513459480421 ) ) ;
#16624 = CARTESIAN_POINT ( 'NONE',  ( -3.175426480542816510, 5.499999999999865885, -110.8750000000000426 ) ) ;
#16625 = CARTESIAN_POINT ( 'NONE',  ( 3.464101615137852974, 5.999999999999884537, -166.3363248654052029 ) ) ;
#16626 = CARTESIAN_POINT ( 'NONE',  ( 0.000000000000000000, 5.999999999999977796, -145.7886751345948255 ) ) ;
#16627 = ORIENTED_EDGE ( 'NONE', *, *, #15131, .T. ) ;
#16628 = CARTESIAN_POINT ( 'NONE',  ( 21.81250000000003908, 1.097466725451619718, 2.649519052838358757 ) ) ;
#16629 = CARTESIAN_POINT ( 'NONE',  ( 0.000000000000000000, 0.000000000000000000, -44.99152654425658682 ) ) ;
#16630 = DIRECTION ( 'NONE',  ( -1.000000000000000000, -1.665334536937736783E-16, -2.220446049250315546E-16 ) ) ;
#16631 = CARTESIAN_POINT ( 'NONE',  ( 18.27382486540526330, -2.499999999999844569, -1.035533905932809473 ) ) ;
#16632 = EDGE_LOOP ( 'NONE', ( #9536, #4232, #1845, #4276 ) ) ;
#16633 = CIRCLE ( 'NONE', #7271, 12.00000000000000178 ) ;
#16634 = CARTESIAN_POINT ( 'NONE',  ( 111.7261751345945555, -1.999999999999971800, 0.8284271247464759513 ) ) ;
#16635 = CARTESIAN_POINT ( 'NONE',  ( 3.175426480543072749, 5.499999999999865885, -178.6250000000000284 ) ) ;
#16636 = ORIENTED_EDGE ( 'NONE', *, *, #1535, .T. ) ;
#16637 = DIRECTION ( 'NONE',  ( -7.147005652999508048E-36, 5.642372883946980038E-36, 1.000000000000000000 ) ) ;
#16638 = CARTESIAN_POINT ( 'NONE',  ( 6.000000000000000000, 2.951592740943527306E-14, -163.5863248654052313 ) ) ;
#16639 = ORIENTED_EDGE ( 'NONE', *, *, #27824, .T. ) ;
#16640 = EDGE_LOOP ( 'NONE', ( #6606, #2586 ) ) ;
#16641 = CARTESIAN_POINT ( 'NONE',  ( -3.464101615137757051, -5.999999999999979572, -142.1636751345948255 ) ) ;
#16642 = CARTESIAN_POINT ( 'NONE',  ( 138.0937500000000284, 6.000000000000005329, 2.485281374238585972 ) ) ;
#16643 = ADVANCED_FACE ( 'NONE', ( #14707 ), #3942, .T. ) ;
#16644 = CARTESIAN_POINT ( 'NONE',  ( -5.412658773652739619, 3.124999999999975131, -141.8169872981078186 ) ) ;
#16645 = FACE_OUTER_BOUND ( 'NONE', #25301, .T. ) ;
#16646 = DIRECTION ( 'NONE',  ( 0.000000000000000000, 0.000000000000000000, -1.000000000000000000 ) ) ;
#16647 = DIRECTION ( 'NONE',  ( -7.147005652999508048E-36, 5.642372883946980038E-36, 1.000000000000000000 ) ) ;
#16648 = CARTESIAN_POINT ( 'NONE',  ( 0.000000000000000000, 0.000000000000000000, 0.000000000000000000 ) ) ;
#16649 = CARTESIAN_POINT ( 'NONE',  ( 19.62500000000008527, -1.414213562372979016, -1.414213562373145550 ) ) ;
#16650 = CARTESIAN_POINT ( 'NONE',  ( -0.04562205425659145164, -14.50000000000004619, 8.291335958003871909 ) ) ;
#16651 = ADVANCED_FACE ( 'NONE', ( #16731 ), #23622, .F. ) ;
#16652 = CARTESIAN_POINT ( 'NONE',  ( 2.081668171172167281E-16, 3.582034040661430693E-16, -2.499999999999999112 ) ) ;
#16653 = CARTESIAN_POINT ( 'NONE',  ( 146.2351497308104342, 3.535533905932725318, -3.535533905932725318 ) ) ;
#16654 = CARTESIAN_POINT ( 'NONE',  ( 5.196152422706629359, 3.000000000000002665, -74.03867513459483973 ) ) ;
#16655 = SURFACE_SIDE_STYLE ('',( #7825 ) ) ;
#16656 = CARTESIAN_POINT ( 'NONE',  ( 24.71049160502954223, -2.207904618590463386, -0.6243674924216627842 ) ) ;
#16657 = CARTESIAN_POINT ( 'NONE',  ( 6.000000000000000888, 1.607695154586715303, -114.0193375672974412 ) ) ;
#16658 = CARTESIAN_POINT ( 'NONE',  ( 110.8749999999998721, 1.767766952966431937, -1.767766952966209892 ) ) ;
#16659 = CARTESIAN_POINT ( 'NONE',  ( 115.2886751345946550, 2.000000000000112799, 3.330669073875469621E-13 ) ) ;
#16660 = CARTESIAN_POINT ( 'NONE',  ( 6.000000000000000888, 1.743066579297358182E-13, -113.1636751345948397 ) ) ;
#16661 = ORIENTED_EDGE ( 'NONE', *, *, #11223, .F. ) ;
#16662 =( BOUNDED_CURVE ( )  B_SPLINE_CURVE ( 2, ( #19893, #26934, #24334, #29237, #23907, #2850, #12269, #545, #19311 ),
 .UNSPECIFIED., .F., .F. ) 
 B_SPLINE_CURVE_WITH_KNOTS ( ( 3, 2, 2, 2, 3 ),
 ( 0.7750000000000000222, 0.7759259259259259078, 0.7777777777777777901, 0.7796296296296296724, 0.7805555555555555580 ),
 .UNSPECIFIED. ) 
 CURVE ( )  GEOMETRIC_REPRESENTATION_ITEM ( )  RATIONAL_B_SPLINE_CURVE ( ( 0.9330127018922194093, 0.9330127018922234061, 1.000000000000000000, 0.8660254037844388186, 1.000000000000000000, 0.8660254037844388186, 1.000000000000000000, 0.9330127018922194093, 0.9330127018922194093 ) ) 
 REPRESENTATION_ITEM ( '' )  );
#16663 = CARTESIAN_POINT ( 'NONE',  ( 3.175426480543072749, -5.500000000000105693, -50.12500000000001421 ) ) ;
#16664 = CARTESIAN_POINT ( 'NONE',  ( 5.999999999999949374, 1.607695154586804565, -53.09668783648702117 ) ) ;
#16665 = CARTESIAN_POINT ( 'NONE',  ( 6.000000000000000888, -1.859271017917181981E-14, -63.08632486540521711 ) ) ;
#16666 = CARTESIAN_POINT ( 'NONE',  ( -5.999999999999956479, -1.607695154586745057, -152.2693375672974412 ) ) ;
#16667 = ORIENTED_EDGE ( 'NONE', *, *, #13799, .F. ) ;
#16668 = CARTESIAN_POINT ( 'NONE',  ( 116.7497167782375413, 1.308140751793585022, 1.308140751793751555 ) ) ;
#16669 = CARTESIAN_POINT ( 'NONE',  ( 139.7812500000000284, 2.485281374238585972, 6.000000000000005329 ) ) ;
#16670 = CARTESIAN_POINT ( 'NONE',  ( -5.412658773652739619, 3.124999999999975131, -105.8169872981078470 ) ) ;
#16671 = CARTESIAN_POINT ( 'NONE',  ( 138.2738248654052313, -3.889087296526011706, 3.889087296526011706 ) ) ;
#16672 = CARTESIAN_POINT ( 'NONE',  ( 159.1726497308104058, -5.000000000000004441, 0.000000000000000000 ) ) ;
#16673 = CARTESIAN_POINT ( 'NONE',  ( 116.9374999999998295, 2.500000000000024425, -1.035533905932629173 ) ) ;
#16674 = ADVANCED_FACE ( 'NONE', ( #26055 ), #397, .T. ) ;
#16675 = CARTESIAN_POINT ( 'NONE',  ( -2.775557561562891351E-14, -5.500000000000115463, -129.7500000000000284 ) ) ;
#16676 = ORIENTED_EDGE ( 'NONE', *, *, #17393, .T. ) ;
#16677 = VERTEX_POINT ( 'NONE', #7169 ) ;
#16678 = CARTESIAN_POINT ( 'NONE',  ( -3.175426480542816510, 5.499999999999865885, -62.87500000000001421 ) ) ;
#16679 = TOROIDAL_SURFACE ( 'NONE', #10794, 29.00000000000000000, 1.000000000000000000 ) ;
#16680 = CARTESIAN_POINT ( 'NONE',  ( -5.999999999999959144, -1.607695154586737951, -179.8466878364870354 ) ) ;
#16681 = DIRECTION ( 'NONE',  ( 1.000000000000000000, 0.000000000000000000, 0.000000000000000000 ) ) ;
#16682 = EDGE_CURVE ( 'NONE', #4758, #23459, #26347, .T. ) ;
#16683 = CARTESIAN_POINT ( 'NONE',  ( 2.775557561562891351E-14, 6.250000000000033751, -85.93301270189223828 ) ) ;
#16684 = CARTESIAN_POINT ( 'NONE',  ( 152.2574251345947971, -2.278174593051795149, 5.500000000000228262 ) ) ;
#16685 = CARTESIAN_POINT ( 'NONE',  ( 104.3122167782373992, -0.7662911109076785410, -1.849990392679291551 ) ) ;
#16686 = CARTESIAN_POINT ( 'NONE',  ( -5.999999999999956479, -1.607695154586745057, -176.2693375672974412 ) ) ;
#16687 = CARTESIAN_POINT ( 'NONE',  ( 119.9377832217623023, -1.849990392679501827, -0.7662911109076485650 ) ) ;
#16688 = CARTESIAN_POINT ( 'NONE',  ( 3.175426480543072749, 5.499999999999865885, -141.1250000000000000 ) ) ;
#16689 = CARTESIAN_POINT ( 'NONE',  ( 140.2041261978397984, -9.046524830661697436, 7.884417203574004773 ) ) ;
#16690 = CARTESIAN_POINT ( 'NONE',  ( 2.775557561562891351E-14, 6.250000000000033751, -153.4330127018922383 ) ) ;
#16691 = DIRECTION ( 'NONE',  ( 1.000000000000000000, 6.938893903907221278E-15, 0.000000000000000000 ) ) ;
#16692 = CARTESIAN_POINT ( 'NONE',  ( -5.196152422706573404, -3.000000000000002665, -73.28867513459481131 ) ) ;
#16693 = CARTESIAN_POINT ( 'NONE',  ( -3.175426480542816066, 5.499999999999865885, -77.87500000000001421 ) ) ;
#16694 = CARTESIAN_POINT ( 'NONE',  ( 13.33632486540539652, -1.767766952966320915, -1.767766952966542959 ) ) ;
#16695 = CARTESIAN_POINT ( 'NONE',  ( -4.763139720814407951, 2.749999999999946709, -68.75000000000002842 ) ) ;
#16696 =( BOUNDED_CURVE ( )  B_SPLINE_CURVE ( 2, ( #15670, #29600, #3627, #15192, #8721, #1334, #6395, #8405, #22243 ),
 .UNSPECIFIED., .F., .T. ) 
 B_SPLINE_CURVE_WITH_KNOTS ( ( 3, 2, 2, 2, 3 ),
 ( 0.8249999999999999556, 0.8259259259259259522, 0.8277777777777777235, 0.8296296296296296058, 0.8305555555555556024 ),
 .UNSPECIFIED. ) 
 CURVE ( )  GEOMETRIC_REPRESENTATION_ITEM ( )  RATIONAL_B_SPLINE_CURVE ( ( 0.9330127018922194093, 0.9330127018922154125, 1.000000000000000000, 0.8660254037844388186, 1.000000000000000000, 0.8660254037844388186, 1.000000000000000000, 0.9330127018922154125, 0.9330127018922194093 ) ) 
 REPRESENTATION_ITEM ( '' )  );
#16697 = CARTESIAN_POINT ( 'NONE',  ( 139.8596287541092522, -9.431323395269577858, 7.852286093092132546 ) ) ;
#16698 = CARTESIAN_POINT ( 'NONE',  ( 147.0148502691896510, -3.535533905932725318, -3.535533905932725318 ) ) ;
#16699 = CARTESIAN_POINT ( 'NONE',  ( 161.0625000000000284, -4.242640687119298093, 4.242640687119298093 ) ) ;
#16700 = CARTESIAN_POINT ( 'NONE',  ( 0.000000000000000000, 5.999999999999977796, -127.2113248654052029 ) ) ;
#16701 =( NAMED_UNIT ( * ) PLANE_ANGLE_UNIT ( ) SI_UNIT ( $, .RADIAN. ) );
#16702 = CIRCLE ( 'NONE', #6358, 0.5000000000000004441 ) ;
#16703 = CARTESIAN_POINT ( 'NONE',  ( -6.000000000000000888, 1.067854986875958443E-15, 7.560779664488942560E-35 ) ) ;
#16704 = CARTESIAN_POINT ( 'NONE',  ( 114.8747167782375840, -5.551115123125782702E-14, 1.849990392679523588 ) ) ;
#16705 = VERTEX_POINT ( 'NONE', #21762 ) ;
#16706 = AXIS2_PLACEMENT_3D ( 'NONE', #25103, #24808, #3903 ) ;
#16707 = CARTESIAN_POINT ( 'NONE',  ( 150.7500000000000284, -6.000000000000005329, 0.000000000000000000 ) ) ;
#16708 = CARTESIAN_POINT ( 'NONE',  ( 119.1011751345947260, 0.8284271247463257382, -1.999999999999851674 ) ) ;
#16709 = CARTESIAN_POINT ( 'NONE',  ( 114.7502832217623592, -1.308140751793640533, 1.308140751793640533 ) ) ;
#16710 = EDGE_CURVE ( 'NONE', #3485, #3730, #4890, .T. ) ;
#16711 = EDGE_CURVE ( 'NONE', #14122, #14750, #10210, .T. ) ;
#16712 = CARTESIAN_POINT ( 'NONE',  ( 19.68750000000015632, -0.8284271247461153509, -1.999999999999971800 ) ) ;
#16713 = CARTESIAN_POINT ( 'NONE',  ( 2.775557561562891351E-14, -6.250000000000061284, -156.3169872981078470 ) ) ;
#16714 = ORIENTED_EDGE ( 'NONE', *, *, #7414, .T. ) ;
#16715 = CARTESIAN_POINT ( 'NONE',  ( 0.000000000000000000, 5.499999999999991118, -88.50000000000002842 ) ) ;
#16716 = CARTESIAN_POINT ( 'NONE',  ( 2.775557561562891351E-14, 6.250000000000033751, -102.4330127018922525 ) ) ;
#16717 = ORIENTED_EDGE ( 'NONE', *, *, #6051, .F. ) ;
#16718 = DIRECTION ( 'NONE',  ( 1.000000000000000000, -5.551115123125774074E-17, -1.260129944081490338E-35 ) ) ;
#16719 = CARTESIAN_POINT ( 'NONE',  ( 154.2038997308104342, 2.071067811865468400, 4.999999999999989342 ) ) ;
#16720 = CARTESIAN_POINT ( 'NONE',  ( -6.350852961085760029, -1.281975124255709124E-13, -167.6249999999999716 ) ) ;
#16721 = CARTESIAN_POINT ( 'NONE',  ( 109.7113248654051176, 2.000000000000057288, 0.000000000000000000 ) ) ;
#16722 = CARTESIAN_POINT ( 'NONE',  ( 0.000000000000000000, 5.999999999999977796, -58.78867513459484684 ) ) ;
#16723 = PRESENTATION_LAYER_ASSIGNMENT (  '', '', ( #13788 ) ) ;
#16724 = CARTESIAN_POINT ( 'NONE',  ( 146.3363248654052029, 0.000000000000000000, -5.500000000000005329 ) ) ;
#16725 = VECTOR ( 'NONE', #10932, 1000.000000000000000 ) ;
#16726 = CARTESIAN_POINT ( 'NONE',  ( 4.763139720814407951, -2.749999999999988454, -171.5000000000000000 ) ) ;
#16727 = CARTESIAN_POINT ( 'NONE',  ( -6.000000000000007105, -1.607695154586655129, -60.76933756729742697 ) ) ;
#16728 = CARTESIAN_POINT ( 'NONE',  ( -2.775557561562891351E-14, -5.500000000000115463, -153.7500000000000568 ) ) ;
#16729 = CARTESIAN_POINT ( 'NONE',  ( 141.0000000000000284, -12.00000000000001066, 4.000000000000003553 ) ) ;
#16730 = CARTESIAN_POINT ( 'NONE',  ( 6.350852961086080661, -9.614813431917819062E-14, -102.3750000000000142 ) ) ;
#16731 = FACE_OUTER_BOUND ( 'NONE', #5689, .T. ) ;
#16732 = CARTESIAN_POINT ( 'NONE',  ( 4.763139720814407951, -2.749999999999988454, -87.50000000000002842 ) ) ;
#16733 = CARTESIAN_POINT ( 'NONE',  ( 156.6711002691896510, 4.999999999999989342, 2.071067811865468400 ) ) ;
#16734 = CARTESIAN_POINT ( 'NONE',  ( 109.7113248654051176, 2.000000000000057288, 0.000000000000000000 ) ) ;
#16735 = VERTEX_POINT ( 'NONE', #14432 ) ;
#16736 = UNCERTAINTY_MEASURE_WITH_UNIT (LENGTH_MEASURE( 1.000000000000000082E-05 ), #21866, 'distance_accuracy_value', 'NONE');
#16737 = CARTESIAN_POINT ( 'NONE',  ( 112.9999999999998579, 2.500000000000057732, 0.000000000000000000 ) ) ;
#16738 = CARTESIAN_POINT ( 'NONE',  ( 112.0863248654050324, -1.414213562373117794, 1.414213562373256572 ) ) ;
#16739 = CARTESIAN_POINT ( 'NONE',  ( 106.0002832217622029, -1.308140751793585022, -1.308140751793640533 ) ) ;
#16740 = CARTESIAN_POINT ( 'NONE',  ( -5.999999999999963585, 1.780251999655701777E-13, -112.4136751345948255 ) ) ;
#16741 = VERTEX_POINT ( 'NONE', #12126 ) ;
#16742 = DIRECTION ( 'NONE',  ( -7.147005652999508048E-36, 5.642372883946980038E-36, 1.000000000000000000 ) ) ;
#16743 = CARTESIAN_POINT ( 'NONE',  ( 140.1636751345948255, 0.000000000000000000, 5.500000000000005329 ) ) ;
#16744 = CIRCLE ( 'NONE', #27489, 2.499999999999999112 ) ;
#16745 = CARTESIAN_POINT ( 'NONE',  ( 110.7113248654050182, 2.000000000000057288, 0.000000000000000000 ) ) ;
#16746 = EDGE_LOOP ( 'NONE', ( #21669, #30163 ) ) ;
#16747 = EDGE_CURVE ( 'NONE', #7693, #1194, #5067, .T. ) ;
#16748 = ORIENTED_EDGE ( 'NONE', *, *, #15154, .T. ) ;
#16749 = CARTESIAN_POINT ( 'NONE',  ( 4.763139720814407951, 2.750000000000002665, -115.7500000000000142 ) ) ;
#16750 = CARTESIAN_POINT ( 'NONE',  ( 17.62500000000005684, 5.551115123125782702E-14, 2.649519052838333888 ) ) ;
#16751 = CARTESIAN_POINT ( 'NONE',  ( -5.412658773652739619, 3.124999999999975131, -120.1830127018922383 ) ) ;
#16752 = UNCERTAINTY_MEASURE_WITH_UNIT (LENGTH_MEASURE( 1.000000000000000082E-05 ), #17509, 'distance_accuracy_value', 'NONE');
#16753 = EDGE_LOOP ( 'NONE', ( #22698, #29695, #18924, #26224 ) ) ;
#16754 = CARTESIAN_POINT ( 'NONE',  ( 3.175426480543072749, -5.500000000000105693, -152.1250000000000568 ) ) ;
#16755 = CARTESIAN_POINT ( 'NONE',  ( 158.7113248654052313, 5.500000000000005329, 0.000000000000000000 ) ) ;
#16756 = CARTESIAN_POINT ( 'NONE',  ( -5.412658773652684552, -3.125000000000099920, -162.5669872981078186 ) ) ;
#16757 = CARTESIAN_POINT ( 'NONE',  ( 108.3749999999998437, -1.767766952966209892, 1.767766952966431937 ) ) ;
#16758 = VERTEX_POINT ( 'NONE', #20219 ) ;
#16759 = CARTESIAN_POINT ( 'NONE',  ( 0.7576871283314742245, -15.57034058591134063, -7.988420828365927484 ) ) ;
#16760 = FACE_OUTER_BOUND ( 'NONE', #18365, .T. ) ;
#16761 = DIRECTION ( 'NONE',  ( 0.000000000000000000, 0.000000000000000000, -1.000000000000000000 ) ) ;
#16762 = CARTESIAN_POINT ( 'NONE',  ( 6.350852961086080661, -9.614813431917819062E-14, -175.8750000000000284 ) ) ;
#16763 = CARTESIAN_POINT ( 'NONE',  ( 106.8127832217621602, -1.849990392679441875, 0.7662911109078888172 ) ) ;
#16764 = CARTESIAN_POINT ( 'NONE',  ( 3.608439182435180470, -6.249999999999997335, -176.5580127018922667 ) ) ;
#16765 = CARTESIAN_POINT ( 'NONE',  ( 119.7886751345947829, -1.999999999999946265, 3.330669073875469621E-13 ) ) ;
#16766 = CARTESIAN_POINT ( 'NONE',  ( 0.000000000000000000, 9.000000000000007105, 5.000000000000004441 ) ) ;
#16767 = AXIS2_PLACEMENT_3D ( 'NONE', #24908, #11116, #19850 ) ;
#16768 = CARTESIAN_POINT ( 'NONE',  ( 3.175426480543072749, 5.499999999999865885, -127.6249999999999858 ) ) ;
#16769 = DIRECTION ( 'NONE',  ( -7.147005652999508048E-36, 5.642372883946980038E-36, 1.000000000000000000 ) ) ;
#16770 = UNCERTAINTY_MEASURE_WITH_UNIT (LENGTH_MEASURE( 1.000000000000000082E-05 ), #4619, 'distance_accuracy_value', 'NONE');
#16771 = CARTESIAN_POINT ( 'NONE',  ( 6.350852961086080661, -9.614813431917819062E-14, -114.3750000000000000 ) ) ;
#16772 = AXIS2_PLACEMENT_3D ( 'NONE', #11727, #21221, #21071 ) ;
#16773 = CARTESIAN_POINT ( 'NONE',  ( -5.999999999999963585, 1.780251999655701777E-13, -100.4136751345948255 ) ) ;
#16774 = ORIENTED_EDGE ( 'NONE', *, *, #4182, .F. ) ;
#16775 = CARTESIAN_POINT ( 'NONE',  ( 16.93750000000007816, -1.097466725451499370, 2.649519052838178457 ) ) ;
#16776 = ADVANCED_FACE ( 'NONE', ( #26780 ), #5899, .F. ) ;
#16777 = CARTESIAN_POINT ( 'NONE',  ( -6.000000000000000888, 1.067854986875958443E-15, 7.560779664488942560E-35 ) ) ;
#16778 = CARTESIAN_POINT ( 'NONE',  ( 5.196152422706629359, 3.000000000000002665, -86.96132486540520290 ) ) ;
#16779 = CARTESIAN_POINT ( 'NONE',  ( 6.000000000000000888, -1.859271017917181981E-14, -126.0863248654052171 ) ) ;
#16780 = AXIS2_PLACEMENT_3D ( 'NONE', #29200, #17892, #22631 ) ;
#16781 = CARTESIAN_POINT ( 'NONE',  ( -2.775557561562891351E-14, -5.500000000000115463, -179.2500000000000284 ) ) ;
#16782 = EDGE_LOOP ( 'NONE', ( #13758, #3799, #25582, #20413 ) ) ;
#16783 = DIRECTION ( 'NONE',  ( -1.734723475976824844E-16, 1.000000000000000000, -0.000000000000000000 ) ) ;
#16784 =( BOUNDED_SURFACE ( )  B_SPLINE_SURFACE ( 3, 2, ( 
 ( #30166, #22965, #4204 ),
 ( #13619, #27997, #9130 ),
 ( #20661, #27846, #6815 ),
 ( #25553, #24158, #23721 ),
 ( #662, #12372, #12080 ),
 ( #7562, #19421, #18980 ),
 ( #24011, #2657, #350 ),
 ( #21266, #7718, #5257 ) ),
 .UNSPECIFIED., .F., .F., .F. ) 
 B_SPLINE_SURFACE_WITH_KNOTS ( ( 4, 2, 2, 4 ),
 ( 3, 3 ),
 ( 3.536383773289560661, 3.830385075063342804, 4.124386376837125390, 4.712388980384689674 ),
 ( 0.000000000000000000, 1.000000000000000000 ),
 .UNSPECIFIED. ) 
 GEOMETRIC_REPRESENTATION_ITEM ( )  RATIONAL_B_SPLINE_SURFACE ( (
 ( 1.000000000000000000, 0.7576044462920088485, 1.000000000000000000),
 ( 1.000000000000000000, 0.7805842023125117990, 1.000000000000000000),
 ( 1.000000000000000000, 0.8091552864627948871, 1.000000000000000000),
 ( 1.000000000000000000, 0.8665500556586516190, 1.000000000000000000),
 ( 1.000000000000000000, 0.8952806170300977584, 1.000000000000000000),
 ( 1.000000000000000000, 0.9690373989632083962, 1.000000000000000000),
 ( 1.000000000000000000, 1.000817594376246511, 1.000000000000000000),
 ( 1.000000000000000000, 1.000000000000000000, 1.000000000000000000) ) ) 
 REPRESENTATION_ITEM ( '' )  SURFACE ( )  );
#16785 = EDGE_CURVE ( 'NONE', #25773, #12739, #19617, .T. ) ;
#16786 = ORIENTED_EDGE ( 'NONE', *, *, #24703, .T. ) ;
#16787 = ORIENTED_EDGE ( 'NONE', *, *, #12614, .F. ) ;
#16788 = CARTESIAN_POINT ( 'NONE',  ( 6.000000000000000888, -1.859271017917181981E-14, -141.6636751345948255 ) ) ;
#16789 = CARTESIAN_POINT ( 'NONE',  ( 138.3750000000000284, 0.000000000000000000, 6.000000000000005329 ) ) ;
#16790 =( BOUNDED_CURVE ( )  B_SPLINE_CURVE ( 2, ( #8009, #17416, #26730, #5695, #25195, #11580, #20775, #11431, #15897 ),
 .UNSPECIFIED., .F., .T. ) 
 B_SPLINE_CURVE_WITH_KNOTS ( ( 3, 2, 2, 2, 3 ),
 ( 0.5468750000000000000, 0.5546875000000000000, 0.5625000000000000000, 0.5703125000000000000, 0.5781250000000000000 ),
 .UNSPECIFIED. ) 
 CURVE ( )  GEOMETRIC_REPRESENTATION_ITEM ( )  RATIONAL_B_SPLINE_CURVE ( ( 1.000000000000000000, 0.9238795325112867385, 1.000000000000000000, 0.9238795325112867385, 1.000000000000000000, 0.9238795325112867385, 1.000000000000000000, 0.9238795325112867385, 1.000000000000000000 ) ) 
 REPRESENTATION_ITEM ( '' )  );
#16791 = VERTEX_POINT ( 'NONE', #29241 ) ;
#16792 = CARTESIAN_POINT ( 'NONE',  ( 5.412658773652739619, 3.124999999999988898, -137.8169872981078186 ) ) ;
#16793 = CARTESIAN_POINT ( 'NONE',  ( 24.33632486540526685, -1.767766952966209892, -1.767766952966487448 ) ) ;
#16794 = VECTOR ( 'NONE', #24010, 1000.000000000000000 ) ;
#16795 = CIRCLE ( 'NONE', #3487, 1.000000000000000000 ) ;
#16796 = CARTESIAN_POINT ( 'NONE',  ( -5.999999999999919176, 1.607695154586804565, -174.9033121635129930 ) ) ;
#16797 = CARTESIAN_POINT ( 'NONE',  ( 5.999999999999974243, 1.607695154586759934, -129.5966878364870354 ) ) ;
#16798 = CARTESIAN_POINT ( 'NONE',  ( 17.50000000000007105, -1.999999999999835243, -5.551115123125782702E-14 ) ) ;
#16799 = CARTESIAN_POINT ( 'NONE',  ( -5.999999999999963585, 8.134310703387671600E-14, -130.4136751345948539 ) ) ;
#16800 = DIRECTION ( 'NONE',  ( -7.147005652999508048E-36, 5.642372883946980038E-36, 1.000000000000000000 ) ) ;
#16801 = LINE ( 'NONE', #16652, #13773 ) ;
#16802 = CARTESIAN_POINT ( 'NONE',  ( 135.8288997308104058, 4.999999999999989342, -2.071067811865468400 ) ) ;
#16803 = CARTESIAN_POINT ( 'NONE',  ( 0.000000000000000000, 5.999999999999977796, -99.28867513459482552 ) ) ;
#16804 = CARTESIAN_POINT ( 'NONE',  ( -5.999999999999963585, 1.780251999655701777E-13, -108.8363248654052313 ) ) ;
#16805 = CARTESIAN_POINT ( 'NONE',  ( 15.41367513459490723, 1.767766952966431937, 1.767766952966209892 ) ) ;
#16806 = CARTESIAN_POINT ( 'NONE',  ( 24.81367708707497144, -0.6026874312555234869, -2.107048546424427737 ) ) ;
#16807 = CARTESIAN_POINT ( 'NONE',  ( 104.9374999999997726, 2.500000000000115019, -1.035533905932448873 ) ) ;
#16808 = CARTESIAN_POINT ( 'NONE',  ( 137.9136751345948539, 0.000000000000000000, -5.500000000000005329 ) ) ;
#16809 = ORIENTED_EDGE ( 'NONE', *, *, #24839, .T. ) ;
#16810 = ADVANCED_FACE ( 'NONE', ( #5745 ), #26487, .F. ) ;
#16811 = CARTESIAN_POINT ( 'NONE',  ( -3.175426480542816066, -5.500000000000057732, -48.87500000000000000 ) ) ;
#16812 = CARTESIAN_POINT ( 'NONE',  ( -5.999999999999919176, 1.607695154586804565, -52.48066243270259434 ) ) ;
#16813 = ORIENTED_EDGE ( 'NONE', *, *, #7157, .F. ) ;
#16814 = CARTESIAN_POINT ( 'NONE',  ( 119.3747167782375413, -5.551115123125782702E-14, -1.849990392679523588 ) ) ;
#16815 = CARTESIAN_POINT ( 'NONE',  ( 118.2886751345946976, 2.000000000000085265, 0.000000000000000000 ) ) ;
#16816 = CARTESIAN_POINT ( 'NONE',  ( -5.412658773652684552, -3.125000000000099920, -102.5669872981078186 ) ) ;
#16817 = CARTESIAN_POINT ( 'NONE',  ( -5.196152422706601826, 2.999999999999975131, -176.4613248654052313 ) ) ;
#16818 = ADVANCED_FACE ( 'NONE', ( #15327 ), #24338, .T. ) ;
#16819 = CARTESIAN_POINT ( 'NONE',  ( 134.3437500000000568, -6.000000000000005329, -2.485281374238555774 ) ) ;
#16820 = CARTESIAN_POINT ( 'NONE',  ( 119.2499999999999574, -5.551115123125782702E-14, 2.500000000000168754 ) ) ;
#16821 = VECTOR ( 'NONE', #15127, 1000.000000000000114 ) ;
#16822 = CARTESIAN_POINT ( 'NONE',  ( 6.350852961086080661, -9.614813431917819062E-14, -130.8750000000000284 ) ) ;
#16823 = VERTEX_POINT ( 'NONE', #1143 ) ;
#16824 = SURFACE_STYLE_USAGE ( .BOTH. , #14085 ) ;
#16825 = CARTESIAN_POINT ( 'NONE',  ( -6.350852961085760029, -1.281975124255709124E-13, -55.12500000000003553 ) ) ;
#16826 = CARTESIAN_POINT ( 'NONE',  ( 2.775557561562891351E-14, 5.874999999999977796, -46.71650635094615467 ) ) ;
#16827 = CARTESIAN_POINT ( 'NONE',  ( 116.0000000000000142, 6.735557395310442023E-16, 5.500000000000000000 ) ) ;
#16828 = CARTESIAN_POINT ( 'NONE',  ( 7.216878364870455975, -6.409875621278545621E-14, -86.30801270189222407 ) ) ;
#16829 = UNCERTAINTY_MEASURE_WITH_UNIT (LENGTH_MEASURE( 1.000000000000000082E-05 ), #13979, 'distance_accuracy_value', 'NONE');
#16830 = CARTESIAN_POINT ( 'NONE',  ( -6.000000000000023093, 1.607695154586625819, -149.4033121635129362 ) ) ;
#16831 = CARTESIAN_POINT ( 'NONE',  ( 106.4372167782374419, 0.7662911109078588412, -1.849990392679231599 ) ) ;
#16832 = DIRECTION ( 'NONE',  ( 0.000000000000000000, 0.000000000000000000, -1.000000000000000000 ) ) ;
#16833 = CARTESIAN_POINT ( 'NONE',  ( 115.4377832217621744, 1.849990392679591977, 0.7662911109078888172 ) ) ;
#16834 = CARTESIAN_POINT ( 'NONE',  ( 0.000000000000000000, 5.499999999999991118, -138.0000000000000000 ) ) ;
#16835 = CARTESIAN_POINT ( 'NONE',  ( -5.999999999999963585, -1.487416814333745711E-14, -105.8363248654052313 ) ) ;
#16836 = CARTESIAN_POINT ( 'NONE',  ( 2.775557561562891351E-14, -6.250000000000061284, -154.1830127018922667 ) ) ;
#16837 = CARTESIAN_POINT ( 'NONE',  ( 3.464101615137852974, 5.999999999999884537, -116.8363248654052171 ) ) ;
#16838 = CARTESIAN_POINT ( 'NONE',  ( 0.000000000000000000, 5.999999999999977796, -51.28867513459483973 ) ) ;
#16839 = ADVANCED_FACE ( 'NONE', ( #10710 ), #12567, .T. ) ;
#16840 = CARTESIAN_POINT ( 'NONE',  ( -6.350852961085760029, -1.281975124255709124E-13, -74.62500000000000000 ) ) ;
#16841 = CARTESIAN_POINT ( 'NONE',  ( -3.175426480542816510, -5.500000000000057732, -68.37500000000002842 ) ) ;
#16842 =( LENGTH_UNIT ( ) NAMED_UNIT ( * ) SI_UNIT ( .MILLI., .METRE. ) );
#16843 = CARTESIAN_POINT ( 'NONE',  ( 146.3586002691896510, 2.071067811865468400, 4.999999999999989342 ) ) ;
#16844 = CARTESIAN_POINT ( 'NONE',  ( 150.8437500000000284, -6.000000000000005329, -2.485281374238556218 ) ) ;
#16845 = CARTESIAN_POINT ( 'NONE',  ( 16.93750000000001421, 2.000000000000151879, -0.8284271247462354770 ) ) ;
#16846 = CARTESIAN_POINT ( 'NONE',  ( 114.7497167782374561, 1.308140751793751555, 1.308140751793973600 ) ) ;
#16847 = EDGE_CURVE ( 'NONE', #9068, #9271, #844, .T. ) ;
#16848 = FACE_OUTER_BOUND ( 'NONE', #3051, .T. ) ;
#16849 = ORIENTED_EDGE ( 'NONE', *, *, #24974, .F. ) ;
#16850 = CARTESIAN_POINT ( 'NONE',  ( 150.0000000000000284, 6.000000000000005329, 0.000000000000000000 ) ) ;
#16851 = CARTESIAN_POINT ( 'NONE',  ( 112.8127832217621886, -1.849990392679441875, 0.7662911109079489913 ) ) ;
#16852 = CARTESIAN_POINT ( 'NONE',  ( 153.8363248654052029, 0.000000000000000000, -5.500000000000005329 ) ) ;
#16853 = UNCERTAINTY_MEASURE_WITH_UNIT (LENGTH_MEASURE( 1.000000000000000082E-05 ), #16924, 'distance_accuracy_value', 'NONE');
#16854 = CARTESIAN_POINT ( 'NONE',  ( 5.196152422706629359, 3.000000000000002665, -64.46132486540523132 ) ) ;
#16855 =( GEOMETRIC_REPRESENTATION_CONTEXT ( 3 ) GLOBAL_UNCERTAINTY_ASSIGNED_CONTEXT ( ( #5036 ) ) GLOBAL_UNIT_ASSIGNED_CONTEXT ( ( #25270, #18105, #8716 ) ) REPRESENTATION_CONTEXT ( 'NONE', 'WORKASPACE' ) );
#16856 = CARTESIAN_POINT ( 'NONE',  ( 3.175426480543072749, 5.499999999999865885, -178.6250000000000284 ) ) ;
#16857 = CARTESIAN_POINT ( 'NONE',  ( 20.56250000000014211, -1.999999999999911626, -0.8284271247462354770 ) ) ;
#16858 = ORIENTED_EDGE ( 'NONE', *, *, #5271, .F. ) ;
#16859 = CARTESIAN_POINT ( 'NONE',  ( -3.608439182435052128, -6.250000000000110134, -154.9419872981078470 ) ) ;
#16860 = VERTEX_POINT ( 'NONE', #10542 ) ;
#16861 = CARTESIAN_POINT ( 'NONE',  ( 4.763139720814407951, 2.750000000000002665, -84.25000000000004263 ) ) ;
#16862 = ORIENTED_EDGE ( 'NONE', *, *, #22328, .T. ) ;
#16863 = SURFACE_STYLE_FILL_AREA ( #27765 ) ;
#16864 = DIRECTION ( 'NONE',  ( -0.000000000000000000, -0.000000000000000000, -1.000000000000000000 ) ) ;
#16865 = CARTESIAN_POINT ( 'NONE',  ( 0.4007817556720155161, -11.00000000000000355, -19.00000000000000355 ) ) ;
#16866 = FACE_OUTER_BOUND ( 'NONE', #6576, .T. ) ;
#16867 = CARTESIAN_POINT ( 'NONE',  ( 140.0256844536734206, -11.04862469602420916, 4.684420475250495208 ) ) ;
#16868 =( BOUNDED_CURVE ( )  B_SPLINE_CURVE ( 2, ( #4287, #14168, #21047, #141, #23506, #25935, #4742, #9362, #16167 ),
 .UNSPECIFIED., .F., .T. ) 
 B_SPLINE_CURVE_WITH_KNOTS ( ( 3, 2, 2, 2, 3 ),
 ( 0.3638888888888889284, 0.3648148148148148140, 0.3666666666666666963, 0.3685185185185184675, 0.3694444444444443532 ),
 .UNSPECIFIED. ) 
 CURVE ( )  GEOMETRIC_REPRESENTATION_ITEM ( )  RATIONAL_B_SPLINE_CURVE ( ( 0.9330127018922194093, 0.9330127018922234061, 1.000000000000000000, 0.8660254037844388186, 1.000000000000000000, 0.8660254037844388186, 1.000000000000000000, 0.9330127018922234061, 0.9330127018922194093 ) ) 
 REPRESENTATION_ITEM ( '' )  );
#16869 = CIRCLE ( 'NONE', #28568, 5.999999999999998224 ) ;
#16870 = CARTESIAN_POINT ( 'NONE',  ( 0.000000000000000000, 5.499999999999991118, -168.0000000000000284 ) ) ;
#16871 = CARTESIAN_POINT ( 'NONE',  ( 161.0000000000000284, 3.467572205841706889, 4.269185284954735593 ) ) ;
#16872 = CARTESIAN_POINT ( 'NONE',  ( 4.763139720814407951, 2.750000000000002665, -153.2500000000000000 ) ) ;
#16873 = CARTESIAN_POINT ( 'NONE',  ( 111.8749999999998437, 1.767766952966348670, -1.767766952966209892 ) ) ;
#16874 = EDGE_CURVE ( 'NONE', #9617, #17636, #8203, .T. ) ;
#16875 = CARTESIAN_POINT ( 'NONE',  ( 6.350852961086080661, -9.614813431917819062E-14, -93.37500000000001421 ) ) ;
#16876 = CARTESIAN_POINT ( 'NONE',  ( 24.22617513459492145, 2.500000000000205169, -1.035533905932869425 ) ) ;
#16877 = EDGE_CURVE ( 'NONE', #4494, #29584, #6633, .T. ) ;
#16878 = CARTESIAN_POINT ( 'NONE',  ( -4.763139720814407951, 2.749999999999946709, -92.75000000000000000 ) ) ;
#16879 = CARTESIAN_POINT ( 'NONE',  ( 13.52382486540523310, 1.035533905932809473, -2.499999999999904521 ) ) ;
#16880 = CARTESIAN_POINT ( 'NONE',  ( 155.0773502691896510, 5.000000000000004441, 0.000000000000000000 ) ) ;
#16881 = CARTESIAN_POINT ( 'NONE',  ( -6.000000000000007105, -1.607695154586655129, -72.76933756729744118 ) ) ;
#16882 = DIRECTION ( 'NONE',  ( 1.000000000000000000, -5.551115123125773458E-17, -1.260129944081490338E-35 ) ) ;
#16883 = CARTESIAN_POINT ( 'NONE',  ( 9.125000000000049738, -2.649519052838111843, 0.000000000000000000 ) ) ;
#16884 = CARTESIAN_POINT ( 'NONE',  ( 114.1874999999998295, 1.035533905932779275, 2.500000000000445421 ) ) ;
#16885 = DIRECTION ( 'NONE',  ( 0.000000000000000000, 0.000000000000000000, -1.000000000000000000 ) ) ;
#16886 = CARTESIAN_POINT ( 'NONE',  ( 20.16367513459488237, 1.767766952966376426, -1.767766952966431937 ) ) ;
#16887 = ORIENTED_EDGE ( 'NONE', *, *, #14049, .T. ) ;
#16888 = CARTESIAN_POINT ( 'NONE',  ( 0.000000000000000000, 0.000000000000000000, 0.000000000000000000 ) ) ;
#16889 = CARTESIAN_POINT ( 'NONE',  ( 135.0000000000000284, -9.165151389911669000, -8.500000000000007105 ) ) ;
#16890 = CARTESIAN_POINT ( 'NONE',  ( 105.1247167782375840, -1.849990392679468076, 0.000000000000000000 ) ) ;
#16891 = ORIENTED_EDGE ( 'NONE', *, *, #10297, .F. ) ;
#16892 = EDGE_LOOP ( 'NONE', ( #13502, #12835, #18328, #25960 ) ) ;
#16893 = CARTESIAN_POINT ( 'NONE',  ( -3.175426480542816510, -5.500000000000057732, -116.3750000000000142 ) ) ;
#16894 = CARTESIAN_POINT ( 'NONE',  ( 19.93750000000006040, -2.649519052838178457, -1.097466725451619718 ) ) ;
#16895 = CARTESIAN_POINT ( 'NONE',  ( 3.608439182435180470, 6.249999999999982236, -126.5580127018922383 ) ) ;
#16896 = ORIENTED_EDGE ( 'NONE', *, *, #21885, .T. ) ;
#16897 = CARTESIAN_POINT ( 'NONE',  ( 6.000000000000000888, -1.607695154586752384, -68.23066243270258724 ) ) ;
#16898 = CARTESIAN_POINT ( 'NONE',  ( -3.608439182435052128, -6.250000000000110134, -157.9419872981077617 ) ) ;
#16899 = CARTESIAN_POINT ( 'NONE',  ( 109.6249999999999858, -1.767766952966376426, -1.767766952966320915 ) ) ;
#16900 = CARTESIAN_POINT ( 'NONE',  ( 136.0000000000000284, 0.000000000000000000, 0.000000000000000000 ) ) ;
#16901 = ORIENTED_EDGE ( 'NONE', *, *, #25044, .T. ) ;
#16902 = CARTESIAN_POINT ( 'NONE',  ( -0.08066462393745461867, -15.01489640285979910, -8.018075067159342595 ) ) ;
#16903 = CARTESIAN_POINT ( 'NONE',  ( -3.464101615137757051, -5.999999999999979572, -132.5863248654052313 ) ) ;
#16904 = CARTESIAN_POINT ( 'NONE',  ( -4.999999999999886313, -69.50000000000001421, -8.000000000000007105 ) ) ;
#16905 = CARTESIAN_POINT ( 'NONE',  ( 0.000000000000000000, 5.499999999999991118, -175.5000000000000000 ) ) ;
#16906 = CARTESIAN_POINT ( 'NONE',  ( 106.9377832217621318, -1.849990392679441875, -0.7662911109075883909 ) ) ;
#16907 = CYLINDRICAL_SURFACE ( 'NONE', #7834, 17.50000000000000355 ) ;
#16908 = CARTESIAN_POINT ( 'NONE',  ( -7.216878364870328078, 0.000000000000000000, -177.0580127018922667 ) ) ;
#16909 = CARTESIAN_POINT ( 'NONE',  ( 13.99999999999999822, 2.020667218593133494E-15, 16.50000000000000355 ) ) ;
#16910 = CARTESIAN_POINT ( 'NONE',  ( -3.175426480542816066, -5.500000000000057732, -122.3749999999999716 ) ) ;
#16911 = DIRECTION ( 'NONE',  ( 0.000000000000000000, 0.000000000000000000, -1.000000000000000000 ) ) ;
#16912 = EDGE_CURVE ( 'NONE', #14487, #1738, #25710, .T. ) ;
#16913 = CARTESIAN_POINT ( 'NONE',  ( -2.775557561562891351E-14, -5.500000000000115463, -110.2500000000000142 ) ) ;
#16914 = DIRECTION ( 'NONE',  ( -7.147005652999508048E-36, 5.642372883946980038E-36, 1.000000000000000000 ) ) ;
#16915 = DIRECTION ( 'NONE',  ( 0.000000000000000000, 0.000000000000000000, -1.000000000000000000 ) ) ;
#16916 = ORIENTED_EDGE ( 'NONE', *, *, #4031, .F. ) ;
#16917 = CARTESIAN_POINT ( 'NONE',  ( 16.68750000000004974, 2.649519052838478661, 1.097466725451499370 ) ) ;
#16918 =( BOUNDED_SURFACE ( )  B_SPLINE_SURFACE ( 1, 2, ( 
 ( #11007, #20351, #29705, #8676, #20662, #2224, #23284, #18982, #25866, #18826, #23575, #11476, #30011, #20972, #22967, #11779, #16388, #20819, #13621, #4814, #18523, #14241, #4517, #16687, #23430, #2375, #21267, #13781, #25709, #4355, #16242, #21120, #206, #55, #1907, #9131, #11940, #18375, #30167, #16542, #11314, #2073, #28000, #16089, #4662, #14095, #8984, #7284, #27847, #2512, #7121, #27690, #9282, #9593, #25393, #6816, #23125, #9444, #25556, #13939, #11628, #30321, #18676, #6970, #28152, #28304, #13102, #663, #2658, #17126, #8447, #19121, #27019, #7719, #5984, #24012, #14817, #23866, #12081, #21420, #9898, #12528, #26304, #16979, #5404, #14666, #19968, #2957, #8280, #17854, #24726, #12375, #24160, #26154, #22438, #16833, #29322, #21723, #28453, #2808, #12233, #19423, #1375, #3667, #7563, #10045, #10785, #5103, #28749, #26453, #19273, #20132, #1210, #352, #3102, #503, #21868, #10618, #15402, #28595, #17693, #29479, #14527, #4956, #14389, #23723, #9745, #21572, #5259, #16015, #11238, #3974, #13253, #29633, #6286, #13709, #15868, #1526, #24874, #1834, #27460, #16170, #20898, #6593, #23206, #30244, #4441, #9210, #25475, #22594, #20744, #8599, #8762, #8914, #6438, #27171, #13866, #9059, #20586, #4130, #6143, #2152, #27323, #29934, #11397, #15709, #3823, #18148, #27618, #15557, #25314, #25166, #11082, #4290, #18005, #25019, #18452, #23050, #1989, #30094, #13398, #22742, #16466, #7054, #21203, #14315, #584, #9819, #430, #23656, #18602, #4592, #6897, #19195, #2885, #14018, #27924, #25938, #2592, #5183, #21648, #4885, #2729, #144, #21050, #23361, #2305, #28232, #12011, #16322, #23948, #21346, #14171, #25641, #287, #11705, #9525, #9671, #28378, #21503, #30398, #26089, #9365, #12158, #12307, #19061, #7206, #28524, #16617, #7493, #18757, #16906, #7358, #16763, #28079, #14596, #25795, #26231, #4745, #23509, #2452, #11863, #18912, #5029, #14462, #23795, #8238, #15361, #7786, #21941, #12451, #7642, #8085, #19777, #10124, #26972, #26526, #17052, #3472, #15190, #14885, #877, #10425, #22242, #21794 ),
 ( #28825, #26382, #10275, #3324, #9971, #29125, #7943, #24227, #19639, #5329, #17650, #1170, #12598, #3177, #12906, #29278, #5479, #17202, #28976, #17353, #5628, #22394, #10578, #19932, #15034, #19349, #14739, #28668, #5937, #24684, #24083, #3034, #26668, #24381, #3626, #13062, #12752, #24524, #22092, #741, #19495, #1027, #17499, #26815, #5778, #6713, #18108, #27277, #13825, #4092, #10745, #22703, #22853, #11198, #4246, #20090, #8876, #29433, #15975, #16130, #8720, #24835, #20250, #29599, #15827, #9024, #30054, #3930, #11041, #18414, #13217, #25127, #20387, #15669, #27734, #27575, #27132, #29744, #6250, #13512, #27428, #24978, #25436, #6101, #8559, #13668, #8404, #17964, #1791, #3785, #20545, #29895, #17812, #4399, #13357, #1955, #25273, #1333, #6394, #23010, #15513, #1642, #22554, #18264, #1487, #10896, #6556, #11358, #20705, #26194, #11673, #14137, #394, #18869, #20857, #4850, #5145, #6862, #14429, #25901, #23766, #11826, #2553, #21014, #30210, #9172, #28044, #248, #23476, #4703, #23619, #2413, #7319, #21164, #26053, #23169, #12122, #104, #21308, #13983, #9784, #4559, #4996, #2697, #18720, #21465, #16873, #19162, #28497, #2113, #7014, #7462, #11517, #30361, #9486, #25607, #18566, #9631, #19025, #23323, #27890, #9329, #2267, #16431, #28344, #25755, #28190, #7166, #16582, #14278, #2297, #21495, #21193, #28225, #28073, #18751, #5174, #2724, #11701, #23650, #14309, #9963, #16899, #9811, #14588, #2446, #21045, #12006, #14011, #12151, #7351, #11855, #4586, #26219, #9519, #23939, #25932, #7632, #14453, #23788, #12296, #4736, #16757, #25788, #7199, #422, #21640, #19190, #17042, #23356, #4879, #26081, #28518, #7489, #30392, #2877, #9359, #575, #19341, #21340, #7049, #23502, #135, #19054, #28660, #16461, #16611, #2583, #14165, #18906, #28371, #281, #9664, #5023, #22232, #21787, #15027, #21932, #19769, #5619, #26965, #10266, #10566, #3462, #10115, #1017, #1162, #12741, #19923, #17642, #29269, #15179, #10417, #3167, #12442, #19485, #5468, #12897, #24370, #730, #24075, #29115, #26658, #15353, #20081 ) ),
 .UNSPECIFIED., .F., .F., .F. ) 
 B_SPLINE_SURFACE_WITH_KNOTS ( ( 2, 2 ),
 ( 3, 2, 2, 2, 2, 2, 2, 2, 2, 2, 2, 2, 2, 2, 2, 2, 2, 2, 2, 2, 2, 2, 2, 2, 2, 2, 2, 2, 2, 2, 2, 2, 2, 2, 2, 2, 2, 2, 2, 2, 2, 2, 2, 2, 2, 2, 2, 2, 2, 2, 2, 2, 2, 2, 2, 2, 2, 2, 2, 2, 2, 2, 2, 2, 2, 2, 2, 2, 2, 2, 2, 2, 2, 2, 2, 2, 2, 2, 2, 2, 2, 2, 2, 2, 2, 2, 2, 2, 2, 2, 2, 2, 2, 2, 2, 2, 2, 2, 2, 2, 2, 2, 2, 2, 2, 2, 2, 2, 2, 2, 2, 2, 2, 2, 2, 2, 2, 2, 2, 2, 2, 2, 2, 2, 2, 2, 2, 2, 2, 2, 2, 2, 3 ),
 ( 0.000000000000000000, 1.000000000000000000 ),
 ( 0.000000000000000000, 0.007352941176470588133, 0.01470588235294117627, 0.02205882352941176613, 0.02941176470588235253, 0.03676470588235294240, 0.04411764705882353227, 0.05147058823529411520, 0.05882352941176470507, 0.06617647058823529493, 0.07352941176470588480, 0.08088235294117647467, 0.08823529411764706454, 0.09558823529411764053, 0.1029411764705882304, 0.1102941176470588203, 0.1176470588235294101, 0.1250000000000000000, 0.1323529411764705899, 0.1397058823529411797, 0.1470588235294117696, 0.1544117647058823595, 0.1617647058823529493, 0.1691176470588235392, 0.1764705882352941291, 0.1838235294117647189, 0.1911764705882352811, 0.1985294117647058709, 0.2058823529411764608, 0.2132352941176470507, 0.2205882352941176405, 0.2279411764705882304, 0.2352941176470588203, 0.2426470588235294101, 0.2500000000000000000, 0.2573529411764705621, 0.2647058823529411797, 0.2720588235294117418, 0.2794117647058823595, 0.2867647058823529216, 0.2941176470588235392, 0.3014705882352941013, 0.3088235294117647189, 0.3161764705882352811, 0.3235294117647058987, 0.3308823529411764608, 0.3382352941176470784, 0.3455882352941176405, 0.3529411764705882582, 0.3602941176470588203, 0.3676470588235294379, 0.3750000000000000000, 0.3823529411764705621, 0.3897058823529411797, 0.3970588235294117418, 0.4044117647058823595, 0.4117647058823529216, 0.4191176470588235392, 0.4264705882352941013, 0.4338235294117647189, 0.4411764705882352811, 0.4485294117647058987, 0.4558823529411764608, 0.4632352941176470784, 0.4705882352941176405, 0.4779411764705882582, 0.4852941176470588203, 0.4926470588235294379, 0.5000000000000000000, 0.5073529411764705621, 0.5147058823529411242, 0.5220588235294117974, 0.5294117647058823595, 0.5367647058823529216, 0.5441176470588234837, 0.5514705882352941568, 0.5588235294117647189, 0.5661764705882352811, 0.5735294117647058432, 0.5808823529411765163, 0.5882352941176470784, 0.5955882352941176405, 0.6029411764705882026, 0.6102941176470588758, 0.6176470588235294379, 0.6250000000000000000, 0.6323529411764705621, 0.6397058823529411242, 0.6470588235294117974, 0.6544117647058823595, 0.6617647058823529216, 0.6691176470588234837, 0.6764705882352941568, 0.6838235294117647189, 0.6911764705882352811, 0.6985294117647058432, 0.7058823529411765163, 0.7132352941176470784, 0.7205882352941176405, 0.7279411764705882026, 0.7352941176470588758, 0.7426470588235294379, 0.7500000000000000000, 0.7573529411764705621, 0.7647058823529411242, 0.7720588235294117974, 0.7794117647058823595, 0.7867647058823529216, 0.7941176470588234837, 0.8014705882352941568, 0.8088235294117647189, 0.8161764705882352811, 0.8235294117647058432, 0.8308823529411765163, 0.8382352941176470784, 0.8455882352941176405, 0.8529411764705882026, 0.8602941176470588758, 0.8676470588235294379, 0.8750000000000000000, 0.8823529411764705621, 0.8897058823529411242, 0.8970588235294117974, 0.9044117647058823595, 0.9117647058823529216, 0.9191176470588234837, 0.9264705882352941568, 0.9338235294117647189, 0.9411764705882352811, 0.9485294117647058432, 0.9558823529411765163, 0.9632352941176470784, 0.9705882352941176405 ),
 .UNSPECIFIED. ) 
 GEOMETRIC_REPRESENTATION_ITEM ( )  RATIONAL_B_SPLINE_SURFACE ( (
 ( 1.000000000000000000, 0.9238795325112867385, 1.000000000000000000, 0.9238795325112867385, 1.000000000000000000, 0.9238795325112867385, 1.000000000000000000, 0.9238795325112867385, 1.000000000000000000, 0.9238795325112867385, 1.000000000000000000, 0.9238795325112867385, 1.000000000000000000, 0.9238795325112867385, 1.000000000000000000, 0.9238795325112867385, 1.000000000000000000, 0.9238795325112867385, 1.000000000000000000, 0.9238795325112867385, 1.000000000000000000, 0.9238795325112867385, 1.000000000000000000, 0.9238795325112867385, 1.000000000000000000, 0.9238795325112867385, 1.000000000000000000, 0.9238795325112867385, 1.000000000000000000, 0.9238795325112867385, 1.000000000000000000, 0.9238795325112867385, 1.000000000000000000, 0.9238795325112867385, 1.000000000000000000, 0.9238795325112867385, 1.000000000000000000, 0.9238795325112867385, 1.000000000000000000, 0.9238795325112867385, 1.000000000000000000, 0.9238795325112867385, 1.000000000000000000, 0.9238795325112867385, 1.000000000000000000, 0.9238795325112867385, 1.000000000000000000, 0.9238795325112867385, 1.000000000000000000, 0.9238795325112867385, 1.000000000000000000, 0.9238795325112867385, 1.000000000000000000, 0.9238795325112867385, 1.000000000000000000, 0.9238795325112867385, 1.000000000000000000, 0.9238795325112867385, 1.000000000000000000, 0.9238795325112867385, 1.000000000000000000, 0.9238795325112867385, 1.000000000000000000, 0.9238795325112867385, 1.000000000000000000, 0.9238795325112867385, 1.000000000000000000, 0.9238795325112867385, 1.000000000000000000, 0.9238795325112867385, 1.000000000000000000, 0.9238795325112867385, 1.000000000000000000, 0.9238795325112867385, 1.000000000000000000, 0.9238795325112867385, 1.000000000000000000, 0.9238795325112867385, 1.000000000000000000, 0.9238795325112867385, 1.000000000000000000, 0.9238795325112867385, 1.000000000000000000, 0.9238795325112867385, 1.000000000000000000, 0.9238795325112867385, 1.000000000000000000, 0.9238795325112867385, 1.000000000000000000, 0.9238795325112867385, 1.000000000000000000, 0.9238795325112867385, 1.000000000000000000, 0.9238795325112867385, 1.000000000000000000, 0.9238795325112867385, 1.000000000000000000, 0.9238795325112867385, 1.000000000000000000, 0.9238795325112867385, 1.000000000000000000, 0.9238795325112867385, 1.000000000000000000, 0.9238795325112867385, 1.000000000000000000, 0.9238795325112867385, 1.000000000000000000, 0.9238795325112867385, 1.000000000000000000, 0.9238795325112867385, 1.000000000000000000, 0.9238795325112867385, 1.000000000000000000, 0.9238795325112867385, 1.000000000000000000, 0.9238795325112867385, 1.000000000000000000, 0.9238795325112867385, 1.000000000000000000, 0.9238795325112867385, 1.000000000000000000, 0.9238795325112867385, 1.000000000000000000, 0.9238795325112867385, 1.000000000000000000, 0.9238795325112867385, 1.000000000000000000, 0.9238795325112867385, 1.000000000000000000, 0.9238795325112867385, 1.000000000000000000, 0.9238795325112867385, 1.000000000000000000, 0.9238795325112867385, 1.000000000000000000, 0.9238795325112867385, 1.000000000000000000, 0.9238795325112867385, 1.000000000000000000, 0.9238795325112867385, 1.000000000000000000, 0.9238795325112867385, 1.000000000000000000, 0.9238795325112867385, 1.000000000000000000, 0.9238795325112867385, 1.000000000000000000, 0.9238795325112867385, 1.000000000000000000, 0.9238795325112867385, 1.000000000000000000, 0.9238795325112867385, 1.000000000000000000, 0.9238795325112867385, 1.000000000000000000, 0.9238795325112867385, 1.000000000000000000, 0.9238795325112867385, 1.000000000000000000, 0.9238795325112867385, 1.000000000000000000, 0.9238795325112867385, 1.000000000000000000, 0.9238795325112867385, 1.000000000000000000, 0.9238795325112867385, 1.000000000000000000, 0.9238795325112867385, 1.000000000000000000, 0.9238795325112867385, 1.000000000000000000, 0.9238795325112867385, 1.000000000000000000, 0.9238795325112867385, 1.000000000000000000, 0.9238795325112867385, 1.000000000000000000, 0.9238795325112867385, 1.000000000000000000, 0.9238795325112867385, 1.000000000000000000, 0.9238795325112867385, 1.000000000000000000, 0.9238795325112867385, 1.000000000000000000, 0.9238795325112867385, 1.000000000000000000, 0.9238795325112867385, 1.000000000000000000, 0.9238795325112867385, 1.000000000000000000, 0.9238795325112867385, 1.000000000000000000, 0.9238795325112867385, 1.000000000000000000, 0.9238795325112867385, 1.000000000000000000, 0.9238795325112867385, 1.000000000000000000, 0.9238795325112867385, 1.000000000000000000, 0.9238795325112867385, 1.000000000000000000, 0.9238795325112867385, 1.000000000000000000, 0.9238795325112867385, 1.000000000000000000, 0.9238795325112867385, 1.000000000000000000, 0.9238795325112867385, 1.000000000000000000, 0.9238795325112867385, 1.000000000000000000, 0.9238795325112867385, 1.000000000000000000, 0.9238795325112867385, 1.000000000000000000, 0.9238795325112867385, 1.000000000000000000, 0.9238795325112867385, 1.000000000000000000, 0.9238795325112867385, 1.000000000000000000, 0.9238795325112867385, 1.000000000000000000, 0.9238795325112867385, 1.000000000000000000, 0.9238795325112867385, 1.000000000000000000, 0.9238795325112867385, 1.000000000000000000, 0.9238795325112867385, 1.000000000000000000, 0.9238795325112867385, 1.000000000000000000, 0.9238795325112867385, 1.000000000000000000, 0.9238795325112867385, 1.000000000000000000, 0.9238795325112867385, 1.000000000000000000, 0.9238795325112867385, 1.000000000000000000, 0.9238795325112867385, 1.000000000000000000, 0.9238795325112867385, 1.000000000000000000, 0.9238795325112867385, 1.000000000000000000, 0.9238795325112867385, 1.000000000000000000, 0.9238795325112867385, 1.000000000000000000, 0.9238795325112867385, 1.000000000000000000, 0.9238795325112867385, 1.000000000000000000, 0.9238795325112867385, 1.000000000000000000, 0.9238795325112867385, 1.000000000000000000, 0.9238795325112867385, 1.000000000000000000, 0.9238795325112867385, 1.000000000000000000),
 ( 1.000000000000000000, 0.9238795325112867385, 1.000000000000000000, 0.9238795325112867385, 1.000000000000000000, 0.9238795325112867385, 1.000000000000000000, 0.9238795325112867385, 1.000000000000000000, 0.9238795325112867385, 1.000000000000000000, 0.9238795325112867385, 1.000000000000000000, 0.9238795325112867385, 1.000000000000000000, 0.9238795325112867385, 1.000000000000000000, 0.9238795325112867385, 1.000000000000000000, 0.9238795325112867385, 1.000000000000000000, 0.9238795325112867385, 1.000000000000000000, 0.9238795325112867385, 1.000000000000000000, 0.9238795325112867385, 1.000000000000000000, 0.9238795325112867385, 1.000000000000000000, 0.9238795325112867385, 1.000000000000000000, 0.9238795325112867385, 1.000000000000000000, 0.9238795325112867385, 1.000000000000000000, 0.9238795325112867385, 1.000000000000000000, 0.9238795325112867385, 1.000000000000000000, 0.9238795325112867385, 1.000000000000000000, 0.9238795325112867385, 1.000000000000000000, 0.9238795325112867385, 1.000000000000000000, 0.9238795325112867385, 1.000000000000000000, 0.9238795325112867385, 1.000000000000000000, 0.9238795325112867385, 1.000000000000000000, 0.9238795325112867385, 1.000000000000000000, 0.9238795325112867385, 1.000000000000000000, 0.9238795325112867385, 1.000000000000000000, 0.9238795325112867385, 1.000000000000000000, 0.9238795325112867385, 1.000000000000000000, 0.9238795325112867385, 1.000000000000000000, 0.9238795325112867385, 1.000000000000000000, 0.9238795325112867385, 1.000000000000000000, 0.9238795325112867385, 1.000000000000000000, 0.9238795325112867385, 1.000000000000000000, 0.9238795325112867385, 1.000000000000000000, 0.9238795325112867385, 1.000000000000000000, 0.9238795325112867385, 1.000000000000000000, 0.9238795325112867385, 1.000000000000000000, 0.9238795325112867385, 1.000000000000000000, 0.9238795325112867385, 1.000000000000000000, 0.9238795325112867385, 1.000000000000000000, 0.9238795325112867385, 1.000000000000000000, 0.9238795325112867385, 1.000000000000000000, 0.9238795325112867385, 1.000000000000000000, 0.9238795325112867385, 1.000000000000000000, 0.9238795325112867385, 1.000000000000000000, 0.9238795325112867385, 1.000000000000000000, 0.9238795325112867385, 1.000000000000000000, 0.9238795325112867385, 1.000000000000000000, 0.9238795325112867385, 1.000000000000000000, 0.9238795325112867385, 1.000000000000000000, 0.9238795325112867385, 1.000000000000000000, 0.9238795325112867385, 1.000000000000000000, 0.9238795325112867385, 1.000000000000000000, 0.9238795325112867385, 1.000000000000000000, 0.9238795325112867385, 1.000000000000000000, 0.9238795325112867385, 1.000000000000000000, 0.9238795325112867385, 1.000000000000000000, 0.9238795325112867385, 1.000000000000000000, 0.9238795325112867385, 1.000000000000000000, 0.9238795325112867385, 1.000000000000000000, 0.9238795325112867385, 1.000000000000000000, 0.9238795325112867385, 1.000000000000000000, 0.9238795325112867385, 1.000000000000000000, 0.9238795325112867385, 1.000000000000000000, 0.9238795325112867385, 1.000000000000000000, 0.9238795325112867385, 1.000000000000000000, 0.9238795325112867385, 1.000000000000000000, 0.9238795325112867385, 1.000000000000000000, 0.9238795325112867385, 1.000000000000000000, 0.9238795325112867385, 1.000000000000000000, 0.9238795325112867385, 1.000000000000000000, 0.9238795325112867385, 1.000000000000000000, 0.9238795325112867385, 1.000000000000000000, 0.9238795325112867385, 1.000000000000000000, 0.9238795325112867385, 1.000000000000000000, 0.9238795325112867385, 1.000000000000000000, 0.9238795325112867385, 1.000000000000000000, 0.9238795325112867385, 1.000000000000000000, 0.9238795325112867385, 1.000000000000000000, 0.9238795325112867385, 1.000000000000000000, 0.9238795325112867385, 1.000000000000000000, 0.9238795325112867385, 1.000000000000000000, 0.9238795325112867385, 1.000000000000000000, 0.9238795325112867385, 1.000000000000000000, 0.9238795325112867385, 1.000000000000000000, 0.9238795325112867385, 1.000000000000000000, 0.9238795325112867385, 1.000000000000000000, 0.9238795325112867385, 1.000000000000000000, 0.9238795325112867385, 1.000000000000000000, 0.9238795325112867385, 1.000000000000000000, 0.9238795325112867385, 1.000000000000000000, 0.9238795325112867385, 1.000000000000000000, 0.9238795325112867385, 1.000000000000000000, 0.9238795325112867385, 1.000000000000000000, 0.9238795325112867385, 1.000000000000000000, 0.9238795325112867385, 1.000000000000000000, 0.9238795325112867385, 1.000000000000000000, 0.9238795325112867385, 1.000000000000000000, 0.9238795325112867385, 1.000000000000000000, 0.9238795325112867385, 1.000000000000000000, 0.9238795325112867385, 1.000000000000000000, 0.9238795325112867385, 1.000000000000000000, 0.9238795325112867385, 1.000000000000000000, 0.9238795325112867385, 1.000000000000000000, 0.9238795325112867385, 1.000000000000000000, 0.9238795325112867385, 1.000000000000000000, 0.9238795325112867385, 1.000000000000000000, 0.9238795325112867385, 1.000000000000000000, 0.9238795325112867385, 1.000000000000000000, 0.9238795325112867385, 1.000000000000000000, 0.9238795325112867385, 1.000000000000000000, 0.9238795325112867385, 1.000000000000000000, 0.9238795325112867385, 1.000000000000000000, 0.9238795325112867385, 1.000000000000000000, 0.9238795325112867385, 1.000000000000000000, 0.9238795325112867385, 1.000000000000000000, 0.9238795325112867385, 1.000000000000000000, 0.9238795325112867385, 1.000000000000000000, 0.9238795325112867385, 1.000000000000000000, 0.9238795325112867385, 1.000000000000000000, 0.9238795325112867385, 1.000000000000000000, 0.9238795325112867385, 1.000000000000000000, 0.9238795325112867385, 1.000000000000000000, 0.9238795325112867385, 1.000000000000000000, 0.9238795325112867385, 1.000000000000000000, 0.9238795325112867385, 1.000000000000000000, 0.9238795325112867385, 1.000000000000000000, 0.9238795325112867385, 1.000000000000000000, 0.9238795325112867385, 1.000000000000000000, 0.9238795325112867385, 1.000000000000000000) ) ) 
 REPRESENTATION_ITEM ( '' )  SURFACE ( )  );
#16919 = CARTESIAN_POINT ( 'NONE',  ( 1.000000004086045946, -16.31569083567854150, 6.338645202004363988 ) ) ;
#16920 = CARTESIAN_POINT ( 'NONE',  ( -5.196152422706573404, -3.000000000000002665, -56.21132486540525264 ) ) ;
#16921 = DIRECTION ( 'NONE',  ( -7.147005652999508048E-36, 5.642372883946980038E-36, 1.000000000000000000 ) ) ;
#16922 = VERTEX_POINT ( 'NONE', #4525 ) ;
#16923 = CARTESIAN_POINT ( 'NONE',  ( 0.000000000000000000, -9.714451465470119729E-16, 17.50000000000004619 ) ) ;
#16924 =( LENGTH_UNIT ( ) NAMED_UNIT ( * ) SI_UNIT ( .MILLI., .METRE. ) );
#16925 = EDGE_LOOP ( 'NONE', ( #11531, #22567, #11511, #14947 ) ) ;
#16926 = CARTESIAN_POINT ( 'NONE',  ( 22.35117513459491789, 2.500000000000024425, 1.035533905932689347 ) ) ;
#16927 = ORIENTED_EDGE ( 'NONE', *, *, #9538, .F. ) ;
#16928 = ORIENTED_EDGE ( 'NONE', *, *, #18705, .F. ) ;
#16929 = CARTESIAN_POINT ( 'NONE',  ( 132.2812500000000000, 2.485281374238585972, 6.000000000000005329 ) ) ;
#16930 = CARTESIAN_POINT ( 'NONE',  ( 161.1562500000000284, -6.000000000000005329, 2.485281374238555774 ) ) ;
#16931 = ORIENTED_EDGE ( 'NONE', *, *, #11372, .F. ) ;
#16932 = CARTESIAN_POINT ( 'NONE',  ( 3.608439182435180470, 6.249999999999982236, -133.1919872981078470 ) ) ;
#16933 = CARTESIAN_POINT ( 'NONE',  ( 12.43750000000007816, 2.649519052838478661, 1.097466725451439196 ) ) ;
#16934 =( GEOMETRIC_REPRESENTATION_CONTEXT ( 3 ) GLOBAL_UNCERTAINTY_ASSIGNED_CONTEXT ( ( #21318 ) ) GLOBAL_UNIT_ASSIGNED_CONTEXT ( ( #22286, #10162, #5820 ) ) REPRESENTATION_CONTEXT ( 'NONE', 'WORKASPACE' ) );
#16935 = ADVANCED_FACE ( 'NONE', ( #23135 ), #27544, .T. ) ;
#16936 = CARTESIAN_POINT ( 'NONE',  ( -5.196152422706601826, 2.999999999999975131, -129.0386751345948824 ) ) ;
#16937 = CARTESIAN_POINT ( 'NONE',  ( 20.25000000000015632, 1.110223024625156540E-13, 1.999999999999946265 ) ) ;
#16938 = CARTESIAN_POINT ( 'NONE',  ( -5.196152422706573404, -3.000000000000002665, -130.2886751345948539 ) ) ;
#16939 = CARTESIAN_POINT ( 'NONE',  ( -5.999999999999963585, -1.487416814333745711E-14, -92.91367513459482552 ) ) ;
#16940 = CARTESIAN_POINT ( 'NONE',  ( 138.6413997308104342, 2.071067811865468400, -4.999999999999989342 ) ) ;
#16941 = CARTESIAN_POINT ( 'NONE',  ( 12.14882486540528284, -2.499999999999964473, 1.035533905932749299 ) ) ;
#16942 = CARTESIAN_POINT ( 'NONE',  ( 15.22617513459492855, 2.500000000000084821, -1.035533905932929599 ) ) ;
#16943 = CARTESIAN_POINT ( 'NONE',  ( 1.000000000000000888, 0.000000000000000000, 17.50000000000000355 ) ) ;
#16944 = CARTESIAN_POINT ( 'NONE',  ( 108.7113248654051176, 2.000000000000057288, 0.000000000000000000 ) ) ;
#16945 = CARTESIAN_POINT ( 'NONE',  ( 104.6874999999998437, -1.035533905932689347, -2.499999999999724221 ) ) ;
#16946 = EDGE_CURVE ( 'NONE', #22830, #26206, #3168, .T. ) ;
#16947 = CARTESIAN_POINT ( 'NONE',  ( -4.763139720814407951, 2.749999999999946709, -134.7500000000000284 ) ) ;
#16948 = DIRECTION ( 'NONE',  ( 1.000000000000000000, 0.000000000000000000, 0.000000000000000000 ) ) ;
#16949 = CARTESIAN_POINT ( 'NONE',  ( 154.0386751345948539, -5.500000000000005329, 0.000000000000000000 ) ) ;
#16950 = VERTEX_POINT ( 'NONE', #2234 ) ;
#16951 = CARTESIAN_POINT ( 'NONE',  ( 107.8511751345945129, -1.999999999999941602, -0.8284271247460553989 ) ) ;
#16952 = CARTESIAN_POINT ( 'NONE',  ( 3.464101615137757051, -5.999999999999979572, -132.9136751345947971 ) ) ;
#16953 = CARTESIAN_POINT ( 'NONE',  ( 117.9136751345946266, -1.414213562373201061, -1.414213562373034527 ) ) ;
#16954 =( BOUNDED_CURVE ( )  B_SPLINE_CURVE ( 2, ( #17328, #26644, #5603, #24349, #3302, #9648, #5009, #14441, #13034 ),
 .UNSPECIFIED., .F., .T. ) 
 B_SPLINE_CURVE_WITH_KNOTS ( ( 3, 2, 2, 2, 3 ),
 ( 0.7638888888888889506, 0.7648148148148148362, 0.7666666666666667185, 0.7685185185185184897, 0.7694444444444443754 ),
 .UNSPECIFIED. ) 
 CURVE ( )  GEOMETRIC_REPRESENTATION_ITEM ( )  RATIONAL_B_SPLINE_CURVE ( ( 0.9330127018922194093, 0.9330127018922234061, 1.000000000000000000, 0.8660254037844388186, 1.000000000000000000, 0.8660254037844388186, 1.000000000000000000, 0.9330127018922234061, 0.9330127018922194093 ) ) 
 REPRESENTATION_ITEM ( '' )  );
#16955 = VERTEX_POINT ( 'NONE', #6520 ) ;
#16956 = CARTESIAN_POINT ( 'NONE',  ( 118.0622167782374277, -1.849990392679381701, 0.7662911109079489913 ) ) ;
#16957 = CARTESIAN_POINT ( 'NONE',  ( 135.5625000000000284, -4.242640687119298093, 4.242640687119298093 ) ) ;
#16958 = CARTESIAN_POINT ( 'NONE',  ( 7.216878364870455975, -6.409875621278545621E-14, -92.94198729810784698 ) ) ;
#16959 = CARTESIAN_POINT ( 'NONE',  ( 6.000000000000000888, -3.330669073875464691E-16, -7.560779664488942560E-35 ) ) ;
#16960 =( BOUNDED_CURVE ( )  B_SPLINE_CURVE ( 2, ( #1232, #8302, #3688, #1393, #10804, #25659, #27792, #4610, #11572 ),
 .UNSPECIFIED., .F., .F. ) 
 B_SPLINE_CURVE_WITH_KNOTS ( ( 3, 2, 2, 2, 3 ),
 ( 0.6093750000000000000, 0.6171875000000000000, 0.6250000000000000000, 0.6328125000000000000, 0.6406250000000000000 ),
 .UNSPECIFIED. ) 
 CURVE ( )  GEOMETRIC_REPRESENTATION_ITEM ( )  RATIONAL_B_SPLINE_CURVE ( ( 1.000000000000000000, 0.9238795325112867385, 1.000000000000000000, 0.9238795325112867385, 1.000000000000000000, 0.9238795325112867385, 1.000000000000000000, 0.9238795325112867385, 1.000000000000000000 ) ) 
 REPRESENTATION_ITEM ( '' )  );
#16961 = CARTESIAN_POINT ( 'NONE',  ( 116.5624999999998721, -2.499999999999844569, -1.035533905932629173 ) ) ;
#16962 = AXIS2_PLACEMENT_3D ( 'NONE', #21330, #18740, #25922 ) ;
#16963 = CARTESIAN_POINT ( 'NONE',  ( 140.5384615384615756, -11.07692307692308908, 4.615384615384614975 ) ) ;
#16964 = CARTESIAN_POINT ( 'NONE',  ( -3.175426480542816510, 5.499999999999865885, -128.8750000000000000 ) ) ;
#16965 = ORIENTED_EDGE ( 'NONE', *, *, #22013, .T. ) ;
#16966 = EDGE_CURVE ( 'NONE', #6311, #278, #12069, .T. ) ;
#16967 = ORIENTED_EDGE ( 'NONE', *, *, #1470, .T. ) ;
#16968 = B_SPLINE_CURVE_WITH_KNOTS ( 'NONE', 3,
 ( #15212, #5797, #22719, #10598 ),
 .UNSPECIFIED., .F., .F.,
 ( 4, 4 ),
 ( 1.734723475976789761E-18, 0.0005141325497624451386 ),
 .UNSPECIFIED. ) ;
#16969 = PRESENTATION_STYLE_ASSIGNMENT (( #16824 ) ) ;
#16970 = AXIS2_PLACEMENT_3D ( 'NONE', #14718, #28646, #5157 ) ;
#16971 = EDGE_CURVE ( 'NONE', #19218, #10990, #15636, .T. ) ;
#16972 = CARTESIAN_POINT ( 'NONE',  ( 0.000000000000000000, 5.499999999999991118, -58.50000000000000000 ) ) ;
#16973 = CARTESIAN_POINT ( 'NONE',  ( -5.999999999999963585, 1.780251999655701777E-13, -81.83632486540521711 ) ) ;
#16974 = CARTESIAN_POINT ( 'NONE',  ( 3.608439182435180470, -6.249999999999997335, -85.05801270189222407 ) ) ;
#16975 = CYLINDRICAL_SURFACE ( 'NONE', #5914, 6.000000000000000888 ) ;
#16976 = CARTESIAN_POINT ( 'NONE',  ( 6.000000000000000888, -3.330669073875464691E-16, -7.560779664488942560E-35 ) ) ;
#16977 = CARTESIAN_POINT ( 'NONE',  ( -5.999999999999962697, 3.323446944526963891E-14, -161.3363248654052597 ) ) ;
#16978 = CARTESIAN_POINT ( 'NONE',  ( 5.196152422706629359, 3.000000000000002665, -61.46132486540523132 ) ) ;
#16979 = CARTESIAN_POINT ( 'NONE',  ( 116.1877832217621886, 0.7662911109078888172, -1.849990392679291551 ) ) ;
#16980 = EDGE_CURVE ( 'NONE', #27301, #3222, #20508, .T. ) ;
#16981 = CARTESIAN_POINT ( 'NONE',  ( -3.175426480542816066, -5.500000000000057732, -143.3750000000000000 ) ) ;
#16982 = AXIS2_PLACEMENT_3D ( 'NONE', #26687, #3344, #12772 ) ;
#16983 = CARTESIAN_POINT ( 'NONE',  ( -5.999999999999919176, 1.607695154586804565, -68.40331216351300725 ) ) ;
#16984 = CARTESIAN_POINT ( 'NONE',  ( 5.412658773652739619, 3.124999999999988898, -153.6830127018922099 ) ) ;
#16985 = CARTESIAN_POINT ( 'NONE',  ( 6.000000000000000888, 1.607695154586715303, -159.0193375672974412 ) ) ;
#16986 = DIRECTION ( 'NONE',  ( 0.000000000000000000, 0.000000000000000000, -1.000000000000000000 ) ) ;
#16987 = CARTESIAN_POINT ( 'NONE',  ( -4.763139720814407951, 2.749999999999946709, -74.75000000000004263 ) ) ;
#16988 = CARTESIAN_POINT ( 'NONE',  ( 6.350852961086080661, -9.614813431917819062E-14, -63.37500000000001421 ) ) ;
#16989 = CARTESIAN_POINT ( 'NONE',  ( 154.7812500000000568, 2.485281374238585972, 6.000000000000005329 ) ) ;
#16990 = CARTESIAN_POINT ( 'NONE',  ( 135.0000000000000000, -7.800730961597594160, -7.983509344454088108 ) ) ;
#16991 = CARTESIAN_POINT ( 'NONE',  ( 17.68750000000009592, -0.8284271247460552878, -1.999999999999971800 ) ) ;
#16992 = LINE ( 'NONE', #19287, #10182 ) ;
#16993 = CARTESIAN_POINT ( 'NONE',  ( 115.6247167782374561, 1.849990392679523588, 0.000000000000000000 ) ) ;
#16994 = CARTESIAN_POINT ( 'NONE',  ( -5.196152422706601826, 2.999999999999975131, -81.96132486540518869 ) ) ;
#16995 = ORIENTED_EDGE ( 'NONE', *, *, #8408, .T. ) ;
#16996 = CARTESIAN_POINT ( 'NONE',  ( 149.2500000000000284, -6.000000000000005329, 0.000000000000000000 ) ) ;
#16997 = CARTESIAN_POINT ( 'NONE',  ( -5.196152422706573404, -3.000000000000002665, -158.7886751345948255 ) ) ;
#16998 = CARTESIAN_POINT ( 'NONE',  ( -4.763139720814407951, -2.750000000000016431, -176.5000000000000000 ) ) ;
#16999 = CARTESIAN_POINT ( 'NONE',  ( 19.62500000000008527, -1.414213562372979016, -1.414213562373145550 ) ) ;
#17000 = ORIENTED_EDGE ( 'NONE', *, *, #22400, .F. ) ;
#17001 = CARTESIAN_POINT ( 'NONE',  ( -5.412658773652684552, -3.125000000000099920, -155.0669872981078470 ) ) ;
#17002 = VECTOR ( 'NONE', #18253, 1000.000000000000000 ) ;
#17003 = ORIENTED_EDGE ( 'NONE', *, *, #18222, .F. ) ;
#17004 = ADVANCED_FACE ( 'NONE', ( #22817 ), #1916, .T. ) ;
#17005 = CARTESIAN_POINT ( 'NONE',  ( 3.175426480543072749, -5.500000000000105693, -81.62500000000002842 ) ) ;
#17006 = CARTESIAN_POINT ( 'NONE',  ( -5.412658773652684552, -3.125000000000099920, -101.9330127018922525 ) ) ;
#17007 = DIRECTION ( 'NONE',  ( -7.147005652999508048E-36, 5.642372883946980038E-36, 1.000000000000000000 ) ) ;
#17008 = AXIS2_PLACEMENT_3D ( 'NONE', #13437, #27361, #22483 ) ;
#17009 = CARTESIAN_POINT ( 'NONE',  ( 140.0000000000000284, -11.45643923738959202, 5.000000000000004441 ) ) ;
#17010 = EDGE_CURVE ( 'NONE', #15344, #1672, #11324, .T. ) ;
#17011 = ADVANCED_FACE ( 'NONE', ( #3899 ), #11484, .T. ) ;
#17012 = CARTESIAN_POINT ( 'NONE',  ( -4.763139720814407951, 2.749999999999946709, -166.2500000000000000 ) ) ;
#17013 = CARTESIAN_POINT ( 'NONE',  ( 143.5238248654052029, 3.889087296526011706, -3.889087296526011706 ) ) ;
#17014 = CARTESIAN_POINT ( 'NONE',  ( -4.763139720814407951, 2.749999999999946709, -154.2500000000000000 ) ) ;
#17015 = CARTESIAN_POINT ( 'NONE',  ( 116.9136751345947260, -1.414213562373034527, -1.414213562372812483 ) ) ;
#17016 = CARTESIAN_POINT ( 'NONE',  ( 119.9999999999997868, 1.387778780781445676E-13, 1.110223024625156540E-13 ) ) ;
#17017 = CARTESIAN_POINT ( 'NONE',  ( -2.775557561562891351E-14, -5.500000000000115463, -93.75000000000000000 ) ) ;
#17018 = CARTESIAN_POINT ( 'NONE',  ( 6.000000000000000888, 1.607695154586715303, -126.0193375672974412 ) ) ;
#17019 = CARTESIAN_POINT ( 'NONE',  ( -10.00000000000000178, -19.99999999999998934, 4.000000000000003553 ) ) ;
#17020 = CARTESIAN_POINT ( 'NONE',  ( 3.175426480543072749, -5.500000000000105693, -89.12500000000000000 ) ) ;
#17021 = DIRECTION ( 'NONE',  ( -7.147005652999508048E-36, 5.642372883946980038E-36, 1.000000000000000000 ) ) ;
#17022 = CARTESIAN_POINT ( 'NONE',  ( 0.000000000000000000, 5.999999999999977796, -143.7113248654052313 ) ) ;
#17023 = CARTESIAN_POINT ( 'NONE',  ( 23.12500000000003553, 1.414213562373090038, 1.414213562373034527 ) ) ;
#17024 = CARTESIAN_POINT ( 'NONE',  ( 109.1874999999997584, 1.035533905932839449, 2.500000000000205169 ) ) ;
#17025 = CARTESIAN_POINT ( 'NONE',  ( -5.999999999999956479, -1.607695154586745057, -66.76933756729744118 ) ) ;
#17026 = CARTESIAN_POINT ( 'NONE',  ( -4.999999999999886313, -70.00000000000001421, -7.500000000000007105 ) ) ;
#17027 = CARTESIAN_POINT ( 'NONE',  ( 20.35117513459494631, 2.500000000000205169, 1.035533905932689347 ) ) ;
#17028 = ORIENTED_EDGE ( 'NONE', *, *, #18895, .T. ) ;
#17029 = CARTESIAN_POINT ( 'NONE',  ( -5.999999999999963585, -1.487416814333745711E-14, -170.3363248654052313 ) ) ;
#17030 = ORIENTED_EDGE ( 'NONE', *, *, #24347, .T. ) ;
#17031 = MECHANICAL_DESIGN_GEOMETRIC_PRESENTATION_REPRESENTATION (  '', ( #8174 ), #14152 ) ;
#17032 = VERTEX_POINT ( 'NONE', #30022 ) ;
#17033 = ADVANCED_FACE ( 'NONE', ( #8992 ), #4055, .F. ) ;
#17034 = CARTESIAN_POINT ( 'NONE',  ( 4.763139720814407951, 2.750000000000002665, -105.2500000000000142 ) ) ;
#17035 = VECTOR ( 'NONE', #13917, 1000.000000000000000 ) ;
#17036 = CARTESIAN_POINT ( 'NONE',  ( 20.06250000000018474, -1.097466725451379244, -2.649519052838419153 ) ) ;
#17037 =( BOUNDED_CURVE ( )  B_SPLINE_CURVE ( 2, ( #8423, #15532, #26831, #19948, #3800, #24543, #15050, #3494, #29142 ),
 .UNSPECIFIED., .F., .T. ) 
 B_SPLINE_CURVE_WITH_KNOTS ( ( 3, 2, 2, 2, 3 ),
 ( 0.7375000000000002665, 0.7437500000000004663, 0.7500000000000006661, 0.7562500000000009770, 0.7625000000000011768 ),
 .UNSPECIFIED. ) 
 CURVE ( )  GEOMETRIC_REPRESENTATION_ITEM ( )  RATIONAL_B_SPLINE_CURVE ( ( 0.9999999999999973355, 0.9238795325112894030, 1.000000000000000000, 0.9238795325112867385, 1.000000000000000000, 0.9238795325112867385, 1.000000000000000000, 0.9238795325112718615, 1.000000000000014877 ) ) 
 REPRESENTATION_ITEM ( '' )  );
#17038 = CARTESIAN_POINT ( 'NONE',  ( -5.412658773652684552, -3.125000000000099920, -121.4330127018922241 ) ) ;
#17039 = ORIENTED_EDGE ( 'NONE', *, *, #4660, .T. ) ;
#17040 = CARTESIAN_POINT ( 'NONE',  ( 6.000000000000000888, 1.743066579297358182E-13, -60.66367513459481842 ) ) ;
#17041 = CARTESIAN_POINT ( 'NONE',  ( 5.412658773652712085, -3.125000000000086153, -163.5669872981078186 ) ) ;
#17042 = CARTESIAN_POINT ( 'NONE',  ( 107.9999999999998863, 2.500000000000002220, 0.000000000000000000 ) ) ;
#17043 = LINE ( 'NONE', #7200, #22375 ) ;
#17044 = CARTESIAN_POINT ( 'NONE',  ( 3.608439182435180470, -6.249999999999997335, -62.55801270189225249 ) ) ;
#17045 = EDGE_LOOP ( 'NONE', ( #7920, #20718, #15567, #1743 ) ) ;
#17046 = CARTESIAN_POINT ( 'NONE',  ( 0.000000000000000000, 5.999999999999977796, -117.2886751345948397 ) ) ;
#17047 = EDGE_CURVE ( 'NONE', #5616, #30043, #13688, .T. ) ;
#17048 = CARTESIAN_POINT ( 'NONE',  ( -5.950275682033375979, 9.251745015924212723, -24.20335556275641054 ) ) ;
#17049 = FACE_OUTER_BOUND ( 'NONE', #2740, .T. ) ;
#17050 = VECTOR ( 'NONE', #26030, 1000.000000000000000 ) ;
#17051 = CARTESIAN_POINT ( 'NONE',  ( 3.175426480543072749, -5.500000000000105693, -179.1250000000000568 ) ) ;
#17052 = CARTESIAN_POINT ( 'NONE',  ( 105.3127832217621034, 1.849990392679562001, -0.7662911109076485650 ) ) ;
#17053 = CARTESIAN_POINT ( 'NONE',  ( 6.000000000000000888, -1.859271017917181981E-14, -168.6636751345947971 ) ) ;
#17054 = CARTESIAN_POINT ( 'NONE',  ( 5.412658773652712085, -3.125000000000086153, -170.4330127018922667 ) ) ;
#17055 = DIRECTION ( 'NONE',  ( -1.000000000000000000, -1.665334536937736783E-16, -2.220446049250315546E-16 ) ) ;
#17056 = PRESENTATION_STYLE_ASSIGNMENT (( #14466 ) ) ;
#17057 = CARTESIAN_POINT ( 'NONE',  ( -6.350852961085760029, -1.281975124255709124E-13, -118.1250000000000426 ) ) ;
#17058 = SURFACE_STYLE_FILL_AREA ( #7649 ) ;
#17059 = CARTESIAN_POINT ( 'NONE',  ( -6.350852961085760029, -1.281975124255709124E-13, -116.6250000000000000 ) ) ;
#17060 = FACE_OUTER_BOUND ( 'NONE', #8462, .T. ) ;
#17061 = CARTESIAN_POINT ( 'NONE',  ( 6.000000000000000888, -1.859271017917181981E-14, -54.08632486540521001 ) ) ;
#17062 = ORIENTED_EDGE ( 'NONE', *, *, #12034, .T. ) ;
#17063 = CARTESIAN_POINT ( 'NONE',  ( 18.68749999999999645, 2.649519052838298805, 1.097466725451499370 ) ) ;
#17064 = CARTESIAN_POINT ( 'NONE',  ( 0.1286836220987009893, -16.20672030812517761, 6.611306774490117277 ) ) ;
#17065 = CARTESIAN_POINT ( 'NONE',  ( -5.196152422706601826, 2.999999999999975131, -108.9613248654052171 ) ) ;
#17066 = CARTESIAN_POINT ( 'NONE',  ( -3.464101615137757051, -5.999999999999979572, -146.0863248654052029 ) ) ;
#17067 = ORIENTED_EDGE ( 'NONE', *, *, #20951, .F. ) ;
#17068 = CARTESIAN_POINT ( 'NONE',  ( 17.47617513459483618, 1.035533905932809473, 2.499999999999964473 ) ) ;
#17069 = DIRECTION ( 'NONE',  ( 0.000000000000000000, 0.000000000000000000, -1.000000000000000000 ) ) ;
#17070 = EDGE_LOOP ( 'NONE', ( #28998, #6691, #8828, #26995, #1679, #10779 ) ) ;
#17071 = DIRECTION ( 'NONE',  ( -1.000000000000000000, -1.665334536937736783E-16, -2.220446049250315546E-16 ) ) ;
#17072 = CIRCLE ( 'NONE', #28326, 1.000000000000000888 ) ;
#17073 = ORIENTED_EDGE ( 'NONE', *, *, #13694, .T. ) ;
#17074 = EDGE_LOOP ( 'NONE', ( #7819, #8581, #25326, #1481 ) ) ;
#17075 = LINE ( 'NONE', #24107, #17949 ) ;
#17076 = CARTESIAN_POINT ( 'NONE',  ( 135.1086002691896795, -2.071067811865468400, -4.999999999999989342 ) ) ;
#17077 = EDGE_CURVE ( 'NONE', #21702, #28373, #14196, .T. ) ;
#17078 = EDGE_CURVE ( 'NONE', #1574, #12351, #7846, .T. ) ;
#17079 = ORIENTED_EDGE ( 'NONE', *, *, #16481, .F. ) ;
#17080 = CARTESIAN_POINT ( 'NONE',  ( 5.412658773652712085, -3.125000000000086153, -135.0669872981078470 ) ) ;
#17081 =( NAMED_UNIT ( * ) SI_UNIT ( $, .STERADIAN. ) SOLID_ANGLE_UNIT ( ) );
#17082 = CARTESIAN_POINT ( 'NONE',  ( -3.464101615137725076, 5.999999999999979572, -130.6636751345948539 ) ) ;
#17083 = CARTESIAN_POINT ( 'NONE',  ( 3.464101615137852974, 5.999999999999884537, -129.4136751345948255 ) ) ;
#17084 = ORIENTED_EDGE ( 'NONE', *, *, #7409, .F. ) ;
#17085 = VECTOR ( 'NONE', #29761, 1000.000000000000000 ) ;
#17086 = CARTESIAN_POINT ( 'NONE',  ( 15.93749999999996980, 2.000000000000091926, -0.8284271247462955401 ) ) ;
#17087 = CARTESIAN_POINT ( 'NONE',  ( -0.004400386472629622125, -15.41927558935930875, -6.289782602405238343 ) ) ;
#17088 = CARTESIAN_POINT ( 'NONE',  ( 149.7261751345948539, -3.889087296526011706, -3.889087296526011706 ) ) ;
#17089 = CARTESIAN_POINT ( 'NONE',  ( 137.6101497308104342, 3.535533905932725318, 3.535533905932725318 ) ) ;
#17090 = FACE_OUTER_BOUND ( 'NONE', #8791, .T. ) ;
#17091 = CARTESIAN_POINT ( 'NONE',  ( -3.464101615137757051, -5.999999999999979572, -140.0863248654051745 ) ) ;
#17092 = LINE ( 'NONE', #21833, #20943 ) ;
#17093 = CARTESIAN_POINT ( 'NONE',  ( -5.196152422706573404, -3.000000000000002665, -69.71132486540521711 ) ) ;
#17094 = CARTESIAN_POINT ( 'NONE',  ( 106.1249999999999858, 1.767766952966320915, 1.767766952966431937 ) ) ;
#17095 = CARTESIAN_POINT ( 'NONE',  ( 0.000000000000000000, 5.499999999999991118, -139.5000000000000000 ) ) ;
#17096 = CARTESIAN_POINT ( 'NONE',  ( 108.5238248654049755, 0.8284271247463257382, -1.999999999999731104 ) ) ;
#17097 = ORIENTED_EDGE ( 'NONE', *, *, #7241, .F. ) ;
#17098 = CARTESIAN_POINT ( 'NONE',  ( -4.763139720814407951, -2.750000000000016431, -47.49999999999998579 ) ) ;
#17099 = CARTESIAN_POINT ( 'NONE',  ( 0.000000000000000000, 0.000000000000000000, 0.000000000000000000 ) ) ;
#17100 = CARTESIAN_POINT ( 'NONE',  ( 118.1011751345946124, 0.8284271247463257382, -1.999999999999851674 ) ) ;
#17101 = CARTESIAN_POINT ( 'NONE',  ( 5.999999999999949374, 1.607695154586804565, -153.0193375672974412 ) ) ;
#17102 = ORIENTED_EDGE ( 'NONE', *, *, #7638, .T. ) ;
#17103 = CARTESIAN_POINT ( 'NONE',  ( 119.3122167782375556, -0.7662911109076785410, -1.849990392679411677 ) ) ;
#17104 = AXIS2_PLACEMENT_3D ( 'NONE', #23099, #30142, #6645 ) ;
#17105 = FILL_AREA_STYLE_COLOUR ( '', #8045 ) ;
#17106 = CARTESIAN_POINT ( 'NONE',  ( -5.412658773652739619, 3.124999999999975131, -92.31698729810783277 ) ) ;
#17107 = CARTESIAN_POINT ( 'NONE',  ( -5.999999999999963585, -1.487416814333745711E-14, -172.4136751345948255 ) ) ;
#17108 = CARTESIAN_POINT ( 'NONE',  ( 11.02382486540524020, -1.035533905932689347, 2.499999999999964473 ) ) ;
#17109 = CARTESIAN_POINT ( 'NONE',  ( 117.4999999999999574, -2.499999999999891198, 0.000000000000000000 ) ) ;
#17110 = ORIENTED_EDGE ( 'NONE', *, *, #532, .F. ) ;
#17111 = CARTESIAN_POINT ( 'NONE',  ( 24.03867513459490013, 1.665334536937734811E-13, -2.500000000000002220 ) ) ;
#17112 = CARTESIAN_POINT ( 'NONE',  ( 3.175426480543072749, -5.500000000000105693, -129.6250000000000284 ) ) ;
#17113 = EDGE_CURVE ( 'NONE', #12780, #13246, #26712, .T. ) ;
#17114 = CARTESIAN_POINT ( 'NONE',  ( 10.00000000000009237, 2.000000000000112799, 0.000000000000000000 ) ) ;
#17115 = ORIENTED_EDGE ( 'NONE', *, *, #27984, .T. ) ;
#17116 = CARTESIAN_POINT ( 'NONE',  ( -5.999999999999956479, -1.607695154586745057, -138.7693375672974412 ) ) ;
#17117 = CARTESIAN_POINT ( 'NONE',  ( -6.350852961085760029, -1.281975124255709124E-13, -59.62500000000000000 ) ) ;
#17118 = B_SPLINE_CURVE_WITH_KNOTS ( 'NONE', 3,
 ( #29425, #3617, #24675, #8395, #19629, #13052, #1323, #24219, #7932, #28816, #3024, #24514 ),
 .UNSPECIFIED., .F., .F.,
 ( 4, 2, 2, 2, 2, 4 ),
 ( 0.000000000000000000, 0.0005856679266213420500, 0.001171335853242684100, 0.001757003779864027343, 0.002049837743174697663, 0.002342671706485368634 ),
 .UNSPECIFIED. ) ;
#17119 = DIRECTION ( 'NONE',  ( 0.000000000000000000, 0.000000000000000000, 1.000000000000000000 ) ) ;
#17120 = SURFACE_STYLE_USAGE ( .BOTH. , #30353 ) ;
#17121 = CARTESIAN_POINT ( 'NONE',  ( 3.608439182435180470, 6.249999999999982236, -83.05801270189220986 ) ) ;
#17122 = CYLINDRICAL_SURFACE ( 'NONE', #20180, 6.000000000000000888 ) ;
#17123 = CARTESIAN_POINT ( 'NONE',  ( -3.464101615137757051, -5.999999999999979572, -152.6636751345947971 ) ) ;
#17124 = CARTESIAN_POINT ( 'NONE',  ( -19.99999999999998224, -25.00000000000010658, 7.500000000000007105 ) ) ;
#17125 = DIRECTION ( 'NONE',  ( 1.000000000000000000, -5.551115123125773458E-17, -1.260129944081490338E-35 ) ) ;
#17126 = CARTESIAN_POINT ( 'NONE',  ( 117.0627832217621318, -0.7662911109077686911, -1.849990392679231599 ) ) ;
#17127 =( BOUNDED_CURVE ( )  B_SPLINE_CURVE ( 2, ( #24500, #19907, #29252, #23302, #18544, #11334, #20521, #27553, #13641 ),
 .UNSPECIFIED., .F., .T. ) 
 B_SPLINE_CURVE_WITH_KNOTS ( ( 3, 2, 2, 2, 3 ),
 ( 0.6861111111111111160, 0.6870370370370371127, 0.6888888888888888840, 0.6907407407407407662, 0.6916666666666666519 ),
 .UNSPECIFIED. ) 
 CURVE ( )  GEOMETRIC_REPRESENTATION_ITEM ( )  RATIONAL_B_SPLINE_CURVE ( ( 0.9330127018922194093, 0.9330127018922194093, 1.000000000000000000, 0.8660254037844388186, 1.000000000000000000, 0.8660254037844388186, 1.000000000000000000, 0.9330127018922234061, 0.9330127018922194093 ) ) 
 REPRESENTATION_ITEM ( '' )  );
#17128 = CARTESIAN_POINT ( 'NONE',  ( -4.763139720814407951, -2.750000000000016431, -143.5000000000000284 ) ) ;
#17129 = CARTESIAN_POINT ( 'NONE',  ( 139.8284140731593652, -9.384860798393967585, 7.878476001700652098 ) ) ;
#17130 = CARTESIAN_POINT ( 'NONE',  ( 2.775557561562891351E-14, -6.250000000000061284, -152.6830127018922099 ) ) ;
#17131 = CARTESIAN_POINT ( 'NONE',  ( 139.5074251345948255, 2.278174593051927044, -5.500000000000096811 ) ) ;
#17132 = CARTESIAN_POINT ( 'NONE',  ( 0.000000000000000000, 5.499999999999991118, -75.00000000000001421 ) ) ;
#17133 = CARTESIAN_POINT ( 'NONE',  ( 6.350852961086080661, -9.614813431917819062E-14, -58.87500000000005684 ) ) ;
#17134 =( BOUNDED_CURVE ( )  B_SPLINE_CURVE ( 2, ( #8372, #17782, #27102, #13332, #1613, #27397, #6362, #27859, #13792 ),
 .UNSPECIFIED., .F., .T. ) 
 B_SPLINE_CURVE_WITH_KNOTS ( ( 3, 2, 2, 2, 3 ),
 ( 0.5472222222222222765, 0.5481481481481481621, 0.5500000000000000444, 0.5518518518518518157, 0.5527777777777778123 ),
 .UNSPECIFIED. ) 
 CURVE ( )  GEOMETRIC_REPRESENTATION_ITEM ( )  RATIONAL_B_SPLINE_CURVE ( ( 0.9330127018922194093, 0.9330127018922234061, 1.000000000000000000, 0.8660254037844388186, 1.000000000000000000, 0.8660254037844388186, 1.000000000000000000, 0.9330127018922154125, 0.9330127018922194093 ) ) 
 REPRESENTATION_ITEM ( '' )  );
#17135 = CARTESIAN_POINT ( 'NONE',  ( 5.196152422706629359, 3.000000000000002665, -53.96132486540522422 ) ) ;
#17136 = CARTESIAN_POINT ( 'NONE',  ( 153.2812500000000000, 2.485281374238585972, 6.000000000000005329 ) ) ;
#17137 = CARTESIAN_POINT ( 'NONE',  ( 135.0000000000000568, -7.637934915400436786, -8.088409639717225375 ) ) ;
#17138 = B_SPLINE_CURVE_WITH_KNOTS ( 'NONE', 3,
 ( #18284, #6269, #15688, #27596, #24998, #3952, #13378, #6573, #1665, #11059, #20405, #18128, #6412, #25147, #15997, #7940, #3321, #17350, #3174, #26228, #19493, #17048, #5476, #28974, #12749, #28822, #5625, #22089, #26665, #9668, #15031, #5026, #12595, #21500, #21645, #26086, #24377, #26378, #19058, #21937, #3031, #5180, #2882, #2727 ),
 .UNSPECIFIED., .F., .F.,
 ( 4, 2, 2, 2, 2, 2, 2, 2, 2, 2, 2, 2, 2, 2, 2, 2, 2, 2, 2, 2, 2, 4 ),
 ( 0.000000000000000000, 0.001197331758471044914, 0.002394663516942089829, 0.003591995275413134743, 0.004789327033884179657, 0.005387992913119706018, 0.005986658792355230643, 0.007183990550826279894, 0.008381322309297329146, 0.009578654067768378397, 0.01017731994700390302, 0.01077598582623942765, 0.01137465170547495227, 0.01197331758471047516, 0.01317064934318152615, 0.01376931522241705598, 0.01436798110165258408, 0.01556531286012364373, 0.01676264461859470339, 0.01736131049783023322, 0.01795997637706576652, 0.01915730813553682965 ),
 .UNSPECIFIED. ) ;
#17139 = EDGE_CURVE ( 'NONE', #7046, #22143, #21274, .T. ) ;
#17140 = CARTESIAN_POINT ( 'NONE',  ( -3.464101615137757051, -5.999999999999979572, -89.08632486540521711 ) ) ;
#17141 = CARTESIAN_POINT ( 'NONE',  ( -3.464101615137725076, 5.999999999999979572, -82.08632486540517448 ) ) ;
#17142 = ORIENTED_EDGE ( 'NONE', *, *, #6959, .F. ) ;
#17143 = CARTESIAN_POINT ( 'NONE',  ( 142.7812500000000568, 2.485281374238585972, 6.000000000000005329 ) ) ;
#17144 = CARTESIAN_POINT ( 'NONE',  ( 14.46132486540527218, 5.551115123125782702E-14, -2.500000000000057732 ) ) ;
#17145 = CARTESIAN_POINT ( 'NONE',  ( 135.0863248654052313, 0.000000000000000000, 5.500000000000005329 ) ) ;
#17146 = EDGE_CURVE ( 'NONE', #18703, #5354, #16633, .T. ) ;
#17147 = CARTESIAN_POINT ( 'NONE',  ( 6.350852961086080661, -9.614813431917819062E-14, -178.8750000000000284 ) ) ;
#17148 = CARTESIAN_POINT ( 'NONE',  ( 21.31250000000010658, -0.8284271247460553989, 1.999999999999971800 ) ) ;
#17149 = CARTESIAN_POINT ( 'NONE',  ( -5.412658773652739619, 3.124999999999975131, -155.3169872981078470 ) ) ;
#17150 = ORIENTED_EDGE ( 'NONE', *, *, #9715, .F. ) ;
#17151 = CARTESIAN_POINT ( 'NONE',  ( -6.350852961085760029, -1.281975124255709124E-13, -82.12500000000004263 ) ) ;
#17152 = CARTESIAN_POINT ( 'NONE',  ( 15.62500000000011013, 1.665334536937734811E-13, 2.649519052838278377 ) ) ;
#17153 = CARTESIAN_POINT ( 'NONE',  ( 5.412658773652739619, 3.124999999999988898, -102.6830127018922241 ) ) ;
#17154 = ORIENTED_EDGE ( 'NONE', *, *, #4003, .F. ) ;
#17155 = CARTESIAN_POINT ( 'NONE',  ( 119.9999999999998721, 2.445790564474887852, 0.3393521411448525704 ) ) ;
#17156 = FACE_OUTER_BOUND ( 'NONE', #26537, .T. ) ;
#17157 = FACE_OUTER_BOUND ( 'NONE', #14724, .T. ) ;
#17158 = CARTESIAN_POINT ( 'NONE',  ( 140.5000000328705028, -11.02580175850465238, 4.736714422037595185 ) ) ;
#17159 = CARTESIAN_POINT ( 'NONE',  ( 0.000000000000000000, 5.499999999999991118, -160.5000000000000284 ) ) ;
#17160 = CARTESIAN_POINT ( 'NONE',  ( 3.464101615137757051, -5.999999999999979572, -80.41367513459479710 ) ) ;
#17161 = CARTESIAN_POINT ( 'NONE',  ( -2.775557561562891351E-14, -5.500000000000115463, -144.7500000000000568 ) ) ;
#17162 = DIRECTION ( 'NONE',  ( 1.000000000000000000, 0.000000000000000000, 0.000000000000000000 ) ) ;
#17163 = VECTOR ( 'NONE', #9737, 1000.000000000000000 ) ;
#17164 = CARTESIAN_POINT ( 'NONE',  ( 3.175426480543072749, -5.500000000000105693, -96.62500000000004263 ) ) ;
#17165 = CARTESIAN_POINT ( 'NONE',  ( 142.3988248654052313, 3.889087296526011706, 3.889087296526011706 ) ) ;
#17166 = CARTESIAN_POINT ( 'NONE',  ( -3.464101615137757051, -5.999999999999979572, -131.0863248654052029 ) ) ;
#17167 = CARTESIAN_POINT ( 'NONE',  ( -4.763139720814407951, -2.750000000000016431, -79.00000000000001421 ) ) ;
#17168 = TOROIDAL_SURFACE ( 'NONE', #27425, 12.50000000000000000, 5.000000000000000000 ) ;
#17169 = CARTESIAN_POINT ( 'NONE',  ( 9.437500000000122569, 1.097466725451679892, -2.649519052838238409 ) ) ;
#17170 = MECHANICAL_DESIGN_GEOMETRIC_PRESENTATION_REPRESENTATION (  '', ( #9330 ), #6863 ) ;
#17171 = CARTESIAN_POINT ( 'NONE',  ( 110.1249999999998437, 1.767766952966265404, 1.767766952966431937 ) ) ;
#17172 = ADVANCED_FACE ( 'NONE', ( #16397, #5675 ), #28315, .F. ) ;
#17173 = CARTESIAN_POINT ( 'NONE',  ( 5.196152422706629359, 3.000000000000002665, -126.5386751345948255 ) ) ;
#17174 = CARTESIAN_POINT ( 'NONE',  ( -9.999999999999772626, -89.00000000000001421, 3.000000000000002665 ) ) ;
#17175 = CARTESIAN_POINT ( 'NONE',  ( 6.000000000000000888, -3.330669073875464691E-16, -7.560779664488942560E-35 ) ) ;
#17176 = ORIENTED_EDGE ( 'NONE', *, *, #19792, .F. ) ;
#17177 = SURFACE_STYLE_USAGE ( .BOTH. , #15012 ) ;
#17178 = DIRECTION ( 'NONE',  ( -1.000000000000000000, -1.665334536937736783E-16, -2.220446049250315546E-16 ) ) ;
#17179 = CARTESIAN_POINT ( 'NONE',  ( 145.7886751345948539, 5.500000000000005329, 0.000000000000000000 ) ) ;
#17180 = CARTESIAN_POINT ( 'NONE',  ( 119.0627832217622739, -0.7662911109077388261, -1.849990392679291551 ) ) ;
#17181 = AXIS2_PLACEMENT_3D ( 'NONE', #22485, #3864, #15756 ) ;
#17182 = VERTEX_POINT ( 'NONE', #16552 ) ;
#17183 = EDGE_CURVE ( 'NONE', #25369, #26795, #22766, .T. ) ;
#17184 = EDGE_CURVE ( 'NONE', #28549, #20877, #17665, .T. ) ;
#17185 = ORIENTED_EDGE ( 'NONE', *, *, #12104, .F. ) ;
#17186 = ORIENTED_EDGE ( 'NONE', *, *, #9744, .F. ) ;
#17187 = CARTESIAN_POINT ( 'NONE',  ( 4.763139720814407951, 2.750000000000002665, -103.7500000000000142 ) ) ;
#17188 = VECTOR ( 'NONE', #872, 1000.000000000000000 ) ;
#17189 = CARTESIAN_POINT ( 'NONE',  ( 19.50000000000004619, 1.873492889145178530, 1.873492889144789952 ) ) ;
#17190 = CARTESIAN_POINT ( 'NONE',  ( -3.608439182435115633, 6.249999999999965361, -126.3080127018922383 ) ) ;
#17191 = ORIENTED_EDGE ( 'NONE', *, *, #26464, .F. ) ;
#17192 = CARTESIAN_POINT ( 'NONE',  ( 5.196152422706629359, -2.999999999999988898, -110.2886751345948397 ) ) ;
#17193 = CARTESIAN_POINT ( 'NONE',  ( -5.412658773652739619, 3.124999999999975131, -161.3169872981078470 ) ) ;
#17194 = CARTESIAN_POINT ( 'NONE',  ( 125.0000000000000568, -55.00000000000000711, 7.500000000000007105 ) ) ;
#17195 = CARTESIAN_POINT ( 'NONE',  ( 21.16367513459491079, 1.767766952966542959, -1.767766952966598470 ) ) ;
#17196 = CARTESIAN_POINT ( 'NONE',  ( -7.216878364870328078, 0.000000000000000000, -60.05801270189223118 ) ) ;
#17197 = ORIENTED_EDGE ( 'NONE', *, *, #5614, .T. ) ;
#17198 = CARTESIAN_POINT ( 'NONE',  ( -0.05026617339078452013, -14.53485816245738960, -8.281223121639204265 ) ) ;
#17199 = CARTESIAN_POINT ( 'NONE',  ( 158.9136751345948539, 0.000000000000000000, -5.500000000000005329 ) ) ;
#17200 = DIRECTION ( 'NONE',  ( -7.147005652999508048E-36, 5.642372883946980038E-36, 1.000000000000000000 ) ) ;
#17201 = CARTESIAN_POINT ( 'NONE',  ( -2.775557561562891351E-14, -5.500000000000115463, -170.2500000000000000 ) ) ;
#17202 = CARTESIAN_POINT ( 'NONE',  ( 119.9374999999996874, 2.500000000000114575, -1.035533905932388699 ) ) ;
#17203 = CARTESIAN_POINT ( 'NONE',  ( 3.464101615137852974, 5.999999999999884537, -100.3363248654052029 ) ) ;
#17204 = CARTESIAN_POINT ( 'NONE',  ( 5.412658773652712085, -3.125000000000086153, -171.9330127018922099 ) ) ;
#17205 = CARTESIAN_POINT ( 'NONE',  ( 0.000000000000000000, 0.000000000000000000, 0.000000000000000000 ) ) ;
#17206 = CARTESIAN_POINT ( 'NONE',  ( -4.763139720814407951, 2.749999999999946709, -113.7500000000000142 ) ) ;
#17207 = CARTESIAN_POINT ( 'NONE',  ( 3.175426480543072749, -5.500000000000105693, -113.1250000000000000 ) ) ;
#17208 = CARTESIAN_POINT ( 'NONE',  ( 3.464101615137757051, -5.999999999999979572, -131.4136751345947687 ) ) ;
#17209 = ORIENTED_EDGE ( 'NONE', *, *, #18843, .F. ) ;
#17210 = CARTESIAN_POINT ( 'NONE',  ( 17.81250000000006395, 1.097466725451619718, 2.649519052838298805 ) ) ;
#17211 = DIRECTION ( 'NONE',  ( 0.000000000000000000, 1.000000000000000000, -0.000000000000000000 ) ) ;
#17212 = EDGE_CURVE ( 'NONE', #8939, #1, #25891, .T. ) ;
#17213 = PRESENTATION_LAYER_ASSIGNMENT (  '', '', ( #20620 ) ) ;
#17214 = CARTESIAN_POINT ( 'NONE',  ( -6.000000000000000888, 1.067854986875958443E-15, 7.560779664488942560E-35 ) ) ;
#17215 = VERTEX_POINT ( 'NONE', #25176 ) ;
#17216 = DIRECTION ( 'NONE',  ( 0.000000000000000000, -1.000000000000000000, 0.000000000000000000 ) ) ;
#17217 = CARTESIAN_POINT ( 'NONE',  ( -1.000000000000000888, 11.00000000000001066, 3.000000000000002665 ) ) ;
#17218 = AXIS2_PLACEMENT_3D ( 'NONE', #10468, #13109, #24880 ) ;
#17219 = CARTESIAN_POINT ( 'NONE',  ( 5.412658773652712085, -3.125000000000086153, -85.56698729810786119 ) ) ;
#17220 = CARTESIAN_POINT ( 'NONE',  ( -5.999999999999963585, 1.780251999655701777E-13, -109.4136751345948113 ) ) ;
#17221 = EDGE_LOOP ( 'NONE', ( #16125, #24036, #10294, #15530 ) ) ;
#17222 = EDGE_CURVE ( 'NONE', #15499, #7376, #12222, .T. ) ;
#17223 = CARTESIAN_POINT ( 'NONE',  ( 24.53846405162355993, 0.8441100269167298720, -2.325921235098170836 ) ) ;
#17224 =( BOUNDED_CURVE ( )  B_SPLINE_CURVE ( 2, ( #21397, #2491, #11914, #635, #7542, #9722, #330, #28720, #5380 ),
 .UNSPECIFIED., .F., .T. ) 
 B_SPLINE_CURVE_WITH_KNOTS ( ( 3, 2, 2, 2, 3 ),
 ( 0.3083333333333333481, 0.3092592592592592338, 0.3111111111111111160, 0.3129629629629629983, 0.3138888888888888840 ),
 .UNSPECIFIED. ) 
 CURVE ( )  GEOMETRIC_REPRESENTATION_ITEM ( )  RATIONAL_B_SPLINE_CURVE ( ( 0.9330127018922194093, 0.9330127018922194093, 1.000000000000000000, 0.8660254037844388186, 1.000000000000000000, 0.8660254037844388186, 1.000000000000000000, 0.9330127018922194093, 0.9330127018922194093 ) ) 
 REPRESENTATION_ITEM ( '' )  );
#17225 = ORIENTED_EDGE ( 'NONE', *, *, #14195, .F. ) ;
#17226 = EDGE_LOOP ( 'NONE', ( #16304, #7340, #29448, #13643 ) ) ;
#17227 = CARTESIAN_POINT ( 'NONE',  ( 132.0937500000000568, 6.000000000000005329, 2.485281374238585972 ) ) ;
#17228 = CARTESIAN_POINT ( 'NONE',  ( 135.5773502691896510, 5.000000000000004441, 0.000000000000000000 ) ) ;
#17229 = CARTESIAN_POINT ( 'NONE',  ( 10.68750000000004441, -0.8284271247460553989, -1.999999999999971800 ) ) ;
#17230 = EDGE_LOOP ( 'NONE', ( #8215, #20491, #8110, #1579 ) ) ;
#17231 = CARTESIAN_POINT ( 'NONE',  ( 3.608439182435180470, -6.249999999999997335, -132.1919872981078470 ) ) ;
#17232 = CARTESIAN_POINT ( 'NONE',  ( 3.464101615137757051, -5.999999999999979572, -167.4136751345948255 ) ) ;
#17233 = ORIENTED_EDGE ( 'NONE', *, *, #15384, .F. ) ;
#17234 = CARTESIAN_POINT ( 'NONE',  ( 14.00000000000006750, 2.000000000000112799, 0.000000000000000000 ) ) ;
#17235 = CARTESIAN_POINT ( 'NONE',  ( 125.0000000000000568, -55.00000000000000711, -8.000000000000007105 ) ) ;
#17236 = DIRECTION ( 'NONE',  ( 1.000000000000000000, 0.000000000000000000, 0.000000000000000000 ) ) ;
#17237 = CARTESIAN_POINT ( 'NONE',  ( -6.000000000000000888, 1.067854986875958443E-15, 7.560779664488942560E-35 ) ) ;
#17238 = STYLED_ITEM ( 'NONE', ( #26636 ), #16776 ) ;
#17239 = CARTESIAN_POINT ( 'NONE',  ( 140.1413997308104058, 2.071067811865468400, -4.999999999999989342 ) ) ;
#17240 = CARTESIAN_POINT ( 'NONE',  ( -5.196152422706573404, -3.000000000000002665, -99.71132486540523132 ) ) ;
#17241 = DIRECTION ( 'NONE',  ( -7.147005652999508048E-36, 5.642372883946980038E-36, 1.000000000000000000 ) ) ;
#17242 = CARTESIAN_POINT ( 'NONE',  ( -5.196152422706573404, -3.000000000000002665, -162.7113248654051745 ) ) ;
#17243 = SURFACE_STYLE_FILL_AREA ( #3212 ) ;
#17244 = CARTESIAN_POINT ( 'NONE',  ( 107.3124999999996589, -1.035533905932598975, 2.500000000000205169 ) ) ;
#17245 = DIRECTION ( 'NONE',  ( 1.000000000000000000, -3.469446951953694061E-16, 0.000000000000000000 ) ) ;
#17246 = CARTESIAN_POINT ( 'NONE',  ( 4.763139720814407951, 2.750000000000002665, -138.2499999999999716 ) ) ;
#17247 = CARTESIAN_POINT ( 'NONE',  ( 108.4613248654050892, 5.551115123125782702E-14, -2.000000000000001776 ) ) ;
#17248 = VERTEX_POINT ( 'NONE', #1082 ) ;
#17249 = EDGE_CURVE ( 'NONE', #25966, #5920, #10473, .T. ) ;
#17250 = CARTESIAN_POINT ( 'NONE',  ( 0.000000000000000000, 5.499999999999991118, -48.00000000000004263 ) ) ;
#17251 = CARTESIAN_POINT ( 'NONE',  ( -9.999999999999980460, -60.00000000000001421, 4.000000000000003553 ) ) ;
#17252 = CARTESIAN_POINT ( 'NONE',  ( 6.000000000000000888, 1.743066579297358182E-13, -99.66367513459479710 ) ) ;
#17253 = EDGE_CURVE ( 'NONE', #14683, #3959, #8135, .T. ) ;
#17254 = ORIENTED_EDGE ( 'NONE', *, *, #5075, .T. ) ;
#17255 = PRODUCT_RELATED_PRODUCT_CATEGORY ( 'part', '', ( #5956 ) ) ;
#17256 = CARTESIAN_POINT ( 'NONE',  ( 118.1247167782376408, -1.849990392679523588, 0.000000000000000000 ) ) ;
#17257 = CARTESIAN_POINT ( 'NONE',  ( 135.4687500000000853, -2.485281374238585972, 6.000000000000005329 ) ) ;
#17258 = CARTESIAN_POINT ( 'NONE',  ( 7.216878364870455975, -6.409875621278545621E-14, -98.94198729810781856 ) ) ;
#17259 = CIRCLE ( 'NONE', #26062, 0.5000000000000004441 ) ;
#17260 = CARTESIAN_POINT ( 'NONE',  ( 6.000000000000052403, -1.607695154586662678, -50.23066243270261566 ) ) ;
#17261 = CARTESIAN_POINT ( 'NONE',  ( 162.0000000000000284, 1.408343819019456176E-15, 11.00000000000000355 ) ) ;
#17262 = CARTESIAN_POINT ( 'NONE',  ( 115.7499999999998153, -1.110223024625156540E-13, -2.499999999999946709 ) ) ;
#17263 = DIRECTION ( 'NONE',  ( 1.000000000000000000, -5.551115123125773458E-17, -1.260129944081490338E-35 ) ) ;
#17264 = AXIS2_PLACEMENT_3D ( 'NONE', #14174, #23512, #2454 ) ;
#17265 = ORIENTED_EDGE ( 'NONE', *, *, #25113, .T. ) ;
#17266 = ORIENTED_EDGE ( 'NONE', *, *, #20481, .T. ) ;
#17267 = CARTESIAN_POINT ( 'NONE',  ( 0.000000000000000000, 0.000000000000000000, 0.000000000000000000 ) ) ;
#17268 = CARTESIAN_POINT ( 'NONE',  ( -4.763139720814407951, 2.749999999999946709, -58.25000000000002132 ) ) ;
#17269 =( BOUNDED_CURVE ( )  B_SPLINE_CURVE ( 2, ( #13438, #8167, #24607, #27061, #6026, #10827, #29531, #15444, #3713 ),
 .UNSPECIFIED., .F., .F. ) 
 B_SPLINE_CURVE_WITH_KNOTS ( ( 3, 2, 2, 2, 3 ),
 ( 0.9749999999999999778, 0.9759259259259259744, 0.9777777777777777457, 0.9796296296296296280, 0.9805555555555555136 ),
 .UNSPECIFIED. ) 
 CURVE ( )  GEOMETRIC_REPRESENTATION_ITEM ( )  RATIONAL_B_SPLINE_CURVE ( ( 0.9330127018922194093, 0.9330127018922154125, 1.000000000000000000, 0.8660254037844388186, 1.000000000000000000, 0.8660254037844388186, 1.000000000000000000, 0.9330127018922234061, 0.9330127018922194093 ) ) 
 REPRESENTATION_ITEM ( '' )  );
#17270 = CARTESIAN_POINT ( 'NONE',  ( -5.999999999999919176, 1.607695154586804565, -68.98066243270260145 ) ) ;
#17271 = CYLINDRICAL_SURFACE ( 'NONE', #28892, 6.000000000000000888 ) ;
#17272 = CARTESIAN_POINT ( 'NONE',  ( 3.464101615137852974, 5.999999999999884537, -67.91367513459479710 ) ) ;
#17273 = CARTESIAN_POINT ( 'NONE',  ( 3.608439182435180470, 6.249999999999982236, -72.55801270189222407 ) ) ;
#17274 = CARTESIAN_POINT ( 'NONE',  ( 153.5476497308104342, 0.000000000000000000, -5.000000000000004441 ) ) ;
#17275 = CARTESIAN_POINT ( 'NONE',  ( 5.196152422706629359, 3.000000000000002665, -169.4613248654052029 ) ) ;
#17276 = CARTESIAN_POINT ( 'NONE',  ( -3.464101615137757051, -5.999999999999979572, -168.5863248654051745 ) ) ;
#17277 = CARTESIAN_POINT ( 'NONE',  ( 116.0000000000000142, 0.000000000000000000, 0.000000000000000000 ) ) ;
#17278 = CIRCLE ( 'NONE', #10898, 15.99999999999998579 ) ;
#17279 = CARTESIAN_POINT ( 'NONE',  ( -3.464101615137757051, -5.999999999999979572, -94.16367513459479710 ) ) ;
#17280 = CARTESIAN_POINT ( 'NONE',  ( 0.000000000000000000, 5.499999999999991118, -142.5000000000000284 ) ) ;
#17281 = DIRECTION ( 'NONE',  ( 1.000000000000000000, 0.000000000000000000, 0.000000000000000000 ) ) ;
#17282 = CARTESIAN_POINT ( 'NONE',  ( 3.608439182435180470, 6.249999999999982236, -152.0580127018922383 ) ) ;
#17283 = CARTESIAN_POINT ( 'NONE',  ( 106.7113248654050324, 2.000000000000001776, 1.110223024625156540E-13 ) ) ;
#17284 = CARTESIAN_POINT ( 'NONE',  ( -4.999999999999886313, -10.00000000000000888, -7.500000000000007105 ) ) ;
#17285 = CARTESIAN_POINT ( 'NONE',  ( -4.763139720814407951, 2.749999999999946709, -71.75000000000004263 ) ) ;
#17286 = CARTESIAN_POINT ( 'NONE',  ( 3.175426480543072749, -5.500000000000105693, -54.62500000000003553 ) ) ;
#17287 = ADVANCED_FACE ( 'NONE', ( #18018 ), #20805, .T. ) ;
#17288 = CARTESIAN_POINT ( 'NONE',  ( -10.00000000000000178, 9.000000000000007105, 3.000000000000002665 ) ) ;
#17289 = ORIENTED_EDGE ( 'NONE', *, *, #21777, .T. ) ;
#17290 = CARTESIAN_POINT ( 'NONE',  ( 141.8586002691896510, 2.071067811865468400, 4.999999999999989342 ) ) ;
#17291 = CARTESIAN_POINT ( 'NONE',  ( 152.7187500000000284, 2.485281374238556218, -6.000000000000005329 ) ) ;
#17292 = CARTESIAN_POINT ( 'NONE',  ( 5.196152422706629359, 3.000000000000002665, -98.03867513459485394 ) ) ;
#17293 = CIRCLE ( 'NONE', #20216, 4.999999999999999112 ) ;
#17294 = CARTESIAN_POINT ( 'NONE',  ( 157.5863248654052597, 0.000000000000000000, 5.500000000000005329 ) ) ;
#17295 = CARTESIAN_POINT ( 'NONE',  ( 145.9687500000000568, -2.485281374238585972, 6.000000000000005329 ) ) ;
#17296 = CARTESIAN_POINT ( 'NONE',  ( 143.3363248654052029, 0.000000000000000000, -5.500000000000005329 ) ) ;
#17297 = PRESENTATION_LAYER_ASSIGNMENT (  '', '', ( #101 ) ) ;
#17298 = AXIS2_PLACEMENT_3D ( 'NONE', #6482, #1248, #4014 ) ;
#17299 = CARTESIAN_POINT ( 'NONE',  ( -0.5000000000000004441, -10.00000000000000888, 5.000000000000004441 ) ) ;
#17300 = CARTESIAN_POINT ( 'NONE',  ( -7.216878364870328078, 0.000000000000000000, -47.19198729810782567 ) ) ;
#17301 = CARTESIAN_POINT ( 'NONE',  ( 15.62500000000013856, -1.414213562372979016, -1.414213562373145550 ) ) ;
#17302 = CARTESIAN_POINT ( 'NONE',  ( -5.412658773652684552, -3.125000000000099920, -150.5669872981077901 ) ) ;
#17303 =( LENGTH_UNIT ( ) NAMED_UNIT ( * ) SI_UNIT ( .MILLI., .METRE. ) );
#17304 = CARTESIAN_POINT ( 'NONE',  ( -3.175426480542816510, -5.500000000000057732, -81.87500000000004263 ) ) ;
#17305 = CARTESIAN_POINT ( 'NONE',  ( 14.12499999999999822, 5.551115123125782702E-14, -2.649519052838444910 ) ) ;
#17306 =( BOUNDED_CURVE ( )  B_SPLINE_CURVE ( 2, ( #19780, #30018, #23132, #24384, #26671, #5631, #15037, #8088, #17502 ),
 .UNSPECIFIED., .F., .T. ) 
 B_SPLINE_CURVE_WITH_KNOTS ( ( 3, 2, 2, 2, 3 ),
 ( 0.2125000000000006883, 0.2187500000000004441, 0.2250000000000002276, 0.2312500000000000111, 0.2374999999999997391 ),
 .UNSPECIFIED. ) 
 CURVE ( )  GEOMETRIC_REPRESENTATION_ITEM ( )  RATIONAL_B_SPLINE_CURVE ( ( 0.9999999999999915623, 0.9238795325112951762, 1.000000000000000000, 0.9238795325112867385, 1.000000000000000000, 0.9238795325112867385, 1.000000000000000000, 0.9238795325112897361, 0.9999999999999970024 ) ) 
 REPRESENTATION_ITEM ( '' )  );
#17307 = ORIENTED_EDGE ( 'NONE', *, *, #8328, .F. ) ;
#17308 = CARTESIAN_POINT ( 'NONE',  ( -6.000000000000007105, -1.607695154586655129, -128.2693375672974128 ) ) ;
#17309 = AXIS2_PLACEMENT_3D ( 'NONE', #23142, #20832, #18538 ) ;
#17310 = EDGE_CURVE ( 'NONE', #15465, #17671, #29500, .T. ) ;
#17311 = CARTESIAN_POINT ( 'NONE',  ( 0.000000000000000000, 0.000000000000000000, 0.000000000000000000 ) ) ;
#17312 = DIRECTION ( 'NONE',  ( 1.000000000000000000, 0.000000000000000000, 0.000000000000000000 ) ) ;
#17313 = CARTESIAN_POINT ( 'NONE',  ( -5.999999999999963585, -1.487416814333745711E-14, -59.33632486540522422 ) ) ;
#17314 = CARTESIAN_POINT ( 'NONE',  ( -3.175426480542816066, -5.500000000000057732, -164.3750000000000568 ) ) ;
#17315 = CARTESIAN_POINT ( 'NONE',  ( 5.196152422706629359, -2.999999999999988898, -60.21132486540520290 ) ) ;
#17316 = CARTESIAN_POINT ( 'NONE',  ( -6.350852961085760029, -1.281975124255709124E-13, -145.1250000000000284 ) ) ;
#17317 = CARTESIAN_POINT ( 'NONE',  ( 134.9999999999999147, 5.939731808376970790, 0.5826989768619842414 ) ) ;
#17318 = CARTESIAN_POINT ( 'NONE',  ( 6.000000000000052403, -1.607695154586662678, -51.73066243270262277 ) ) ;
#17319 = CARTESIAN_POINT ( 'NONE',  ( 3.175426480543072749, -5.500000000000105693, -95.12500000000002842 ) ) ;
#17320 = CARTESIAN_POINT ( 'NONE',  ( 6.350852961086080661, -9.614813431917819062E-14, -79.87500000000001421 ) ) ;
#17321 = ADVANCED_FACE ( 'NONE', ( #18887 ), #7030, .F. ) ;
#17322 = CARTESIAN_POINT ( 'NONE',  ( 153.7648502691896510, 3.535533905932725318, 3.535533905932752852 ) ) ;
#17323 = CARTESIAN_POINT ( 'NONE',  ( 0.000000000000000000, -5.999999999999991118, -72.46132486540524553 ) ) ;
#17324 = CARTESIAN_POINT ( 'NONE',  ( 151.8824251345948255, 5.500000000000012434, 2.278174593052012309 ) ) ;
#17325 = CARTESIAN_POINT ( 'NONE',  ( 22.18750000000018119, 0.8284271247464156662, 1.999999999999971800 ) ) ;
#17326 = CARTESIAN_POINT ( 'NONE',  ( -5.999999999999963585, -1.487416814333745711E-14, -128.3363248654052029 ) ) ;
#17327 = DIRECTION ( 'NONE',  ( 1.000000000000000000, 0.000000000000000000, 0.000000000000000000 ) ) ;
#17328 = CARTESIAN_POINT ( 'NONE',  ( 6.000000000000000888, 1.743066579297358182E-13, -78.66367513459482552 ) ) ;
#17329 = ORIENTED_EDGE ( 'NONE', *, *, #3831, .F. ) ;
#17330 = CARTESIAN_POINT ( 'NONE',  ( 159.5625000000000284, -4.242640687119298093, 4.242640687119298093 ) ) ;
#17331 = CARTESIAN_POINT ( 'NONE',  ( 0.000000000000000000, 0.000000000000000000, 0.000000000000000000 ) ) ;
#17332 = CARTESIAN_POINT ( 'NONE',  ( 5.196152422706629359, -2.999999999999988898, -78.78867513459486815 ) ) ;
#17333 = CARTESIAN_POINT ( 'NONE',  ( 121.0627832217620750, -0.7662911109076785410, -1.849990392679291551 ) ) ;
#17334 = VERTEX_POINT ( 'NONE', #27341 ) ;
#17335 = ORIENTED_EDGE ( 'NONE', *, *, #1174, .F. ) ;
#17336 = CARTESIAN_POINT ( 'NONE',  ( -6.350852961085760029, -1.281975124255709124E-13, -104.6250000000000142 ) ) ;
#17337 = CARTESIAN_POINT ( 'NONE',  ( 18.68750000000005329, -1.097466725451499370, 2.649519052838238409 ) ) ;
#17338 = CARTESIAN_POINT ( 'NONE',  ( 5.412658773652739619, 3.124999999999988898, -123.6830127018922525 ) ) ;
#17339 = CIRCLE ( 'NONE', #4057, 0.9999999999999991118 ) ;
#17340 = EDGE_LOOP ( 'NONE', ( #4381, #17676, #19761, #15298 ) ) ;
#17341 = CARTESIAN_POINT ( 'NONE',  ( -5.999999999999963585, 8.134310703387671600E-14, -135.8363248654052597 ) ) ;
#17342 = CARTESIAN_POINT ( 'NONE',  ( 2.775557561562891351E-14, 6.250000000000033751, -163.0669872981078186 ) ) ;
#17343 = DIRECTION ( 'NONE',  ( -7.147005652999508048E-36, 5.642372883946980038E-36, 1.000000000000000000 ) ) ;
#17344 = CARTESIAN_POINT ( 'NONE',  ( 147.1949251345948539, 5.500000000000012434, -2.278174593052012309 ) ) ;
#17345 = EDGE_CURVE ( 'NONE', #26264, #25850, #23928, .T. ) ;
#17346 = CARTESIAN_POINT ( 'NONE',  ( 3.608439182435180470, 6.249999999999982236, -60.55801270189223118 ) ) ;
#17347 = ORIENTED_EDGE ( 'NONE', *, *, #11296, .F. ) ;
#17348 = DIRECTION ( 'NONE',  ( -7.147005652999508048E-36, 5.642372883946980038E-36, 1.000000000000000000 ) ) ;
#17349 = CARTESIAN_POINT ( 'NONE',  ( -6.000000000000000888, 1.067854986875958443E-15, 7.560779664488942560E-35 ) ) ;
#17350 = CARTESIAN_POINT ( 'NONE',  ( -5.959171229995748220, 9.246457381727791969, -25.80348449789763876 ) ) ;
#17351 = DIRECTION ( 'NONE',  ( 1.000000000000000000, 0.000000000000000000, 0.000000000000000000 ) ) ;
#17352 = CARTESIAN_POINT ( 'NONE',  ( -6.350852961085760029, -1.281975124255709124E-13, -167.6249999999999716 ) ) ;
#17353 = CARTESIAN_POINT ( 'NONE',  ( 119.8124999999998863, 1.035533905932839449, -2.499999999999844569 ) ) ;
#17354 = CARTESIAN_POINT ( 'NONE',  ( -5.999999999999919176, 1.607695154586804565, -99.90331216351299304 ) ) ;
#17355 = CARTESIAN_POINT ( 'NONE',  ( 5.412658773652739619, 3.124999999999988898, -165.6830127018922383 ) ) ;
#17356 = CARTESIAN_POINT ( 'NONE',  ( 5.999999999999949374, 1.607695154586804565, -48.59668783648704249 ) ) ;
#17357 = DIRECTION ( 'NONE',  ( 1.000000000000000000, -5.551115123125773458E-17, -1.260129944081490338E-35 ) ) ;
#17358 = CARTESIAN_POINT ( 'NONE',  ( 135.0124371858787526, -7.358334781654392920, 8.428837531783013759 ) ) ;
#17359 = EDGE_CURVE ( 'NONE', #4337, #26795, #8616, .T. ) ;
#17360 = CARTESIAN_POINT ( 'NONE',  ( 3.175426480543072749, 5.499999999999865885, -106.6250000000000284 ) ) ;
#17361 = CYLINDRICAL_SURFACE ( 'NONE', #20014, 6.000000000000000888 ) ;
#17362 = LINE ( 'NONE', #19646, #14081 ) ;
#17363 = EDGE_CURVE ( 'NONE', #11174, #8510, #20005, .T. ) ;
#17364 = ORIENTED_EDGE ( 'NONE', *, *, #21840, .T. ) ;
#17365 = CARTESIAN_POINT ( 'NONE',  ( 120.1874999999997016, 1.035533905932809473, 2.500000000000205169 ) ) ;
#17366 = CARTESIAN_POINT ( 'NONE',  ( 135.1659834729329930, -8.213724325835228157, -8.175323444973551901 ) ) ;
#17367 = AXIS2_PLACEMENT_3D ( 'NONE', #18579, #2424, #13678 ) ;
#17368 = ORIENTED_EDGE ( 'NONE', *, *, #12931, .F. ) ;
#17369 = CARTESIAN_POINT ( 'NONE',  ( 3.608439182435180470, -6.249999999999997335, -82.69198729810781856 ) ) ;
#17370 = ORIENTED_EDGE ( 'NONE', *, *, #29691, .F. ) ;
#17371 = CYLINDRICAL_SURFACE ( 'NONE', #16982, 6.000000000000000888 ) ;
#17372 = VERTEX_POINT ( 'NONE', #27480 ) ;
#17373 = EDGE_LOOP ( 'NONE', ( #17079, #16927 ) ) ;
#17374 = CARTESIAN_POINT ( 'NONE',  ( 133.6086002691896510, -2.071067811865468400, -4.999999999999989342 ) ) ;
#17375 = ORIENTED_EDGE ( 'NONE', *, *, #6987, .F. ) ;
#17376 = CARTESIAN_POINT ( 'NONE',  ( 7.216878364870455975, -6.409875621278545621E-14, -133.4419872981077901 ) ) ;
#17377 =( NAMED_UNIT ( * ) SI_UNIT ( $, .STERADIAN. ) SOLID_ANGLE_UNIT ( ) );
#17378 = CARTESIAN_POINT ( 'NONE',  ( 136.0000000000000284, -9.165151389911695645, -8.000000000000007105 ) ) ;
#17379 = FACE_OUTER_BOUND ( 'NONE', #10472, .T. ) ;
#17380 = EDGE_CURVE ( 'NONE', #24771, #22382, #20152, .T. ) ;
#17381 = ORIENTED_EDGE ( 'NONE', *, *, #23855, .T. ) ;
#17382 = CARTESIAN_POINT ( 'NONE',  ( 15.25000000000012434, 1.110223024625156540E-13, 1.999999999999946265 ) ) ;
#17383 = CARTESIAN_POINT ( 'NONE',  ( 15.00000000000000000, 2.081899558550500674E-15, 16.50000000000000355 ) ) ;
#17384 = CARTESIAN_POINT ( 'NONE',  ( 135.0788997308104342, -4.999999999999989342, 2.071067811865468400 ) ) ;
#17385 = DIRECTION ( 'NONE',  ( 5.551115123125783935E-17, -1.000000000000000000, -8.881784197001254296E-16 ) ) ;
#17386 = CARTESIAN_POINT ( 'NONE',  ( 10.00000000000002309, 8.326672684688674053E-14, 1.110223024625156540E-13 ) ) ;
#17387 = CARTESIAN_POINT ( 'NONE',  ( 5.412658773652739619, 3.124999999999988898, -67.31698729810780435 ) ) ;
#17388 = CARTESIAN_POINT ( 'NONE',  ( 5.412658773652712085, -3.125000000000086153, -57.06698729810783277 ) ) ;
#17389 = DIRECTION ( 'NONE',  ( 0.000000000000000000, 0.000000000000000000, -1.000000000000000000 ) ) ;
#17390 = CARTESIAN_POINT ( 'NONE',  ( -5.999999999999963585, -1.487416814333745711E-14, -128.9136751345948539 ) ) ;
#17391 = CARTESIAN_POINT ( 'NONE',  ( 105.4999999999999147, -2.499999999999919176, 1.110223024625156540E-13 ) ) ;
#17392 = CARTESIAN_POINT ( 'NONE',  ( -5.999999999999963585, 1.780251999655701777E-13, -74.33632486540523132 ) ) ;
#17393 = EDGE_CURVE ( 'NONE', #1437, #13422, #29010, .T. ) ;
#17394 = CARTESIAN_POINT ( 'NONE',  ( 6.350852961086080661, -9.614813431917819062E-14, -127.8749999999999858 ) ) ;
#17395 = EDGE_CURVE ( 'NONE', #25470, #28274, #15884, .T. ) ;
#17396 = CARTESIAN_POINT ( 'NONE',  ( 108.2738248654049471, -1.999999999999941602, -0.8284271247459952248 ) ) ;
#17397 = EDGE_LOOP ( 'NONE', ( #23347, #14185, #2606, #13562 ) ) ;
#17398 = CARTESIAN_POINT ( 'NONE',  ( 13.14882486540533257, -2.499999999999844569, 1.035533905932689347 ) ) ;
#17399 = DIRECTION ( 'NONE',  ( 5.551115123125785167E-17, -1.000000000000000000, -8.881784197001256268E-16 ) ) ;
#17400 = CARTESIAN_POINT ( 'NONE',  ( -5.196152422706573404, -3.000000000000002665, -160.2886751345948824 ) ) ;
#17401 = CARTESIAN_POINT ( 'NONE',  ( 1.000000000000000888, -16.43939393939394833, 5.999693900976793337 ) ) ;
#17402 =( BOUNDED_CURVE ( )  B_SPLINE_CURVE ( 2, ( #15278, #24605, #19568, #13143, #17581, #1417, #23056, #8486, #19857 ),
 .UNSPECIFIED., .F., .T. ) 
 B_SPLINE_CURVE_WITH_KNOTS ( ( 3, 2, 2, 2, 3 ),
 ( 0.01562500000000000000, 0.02343750000000000000, 0.03125000000000000000, 0.03906250000000000000, 0.04687500000000000000 ),
 .UNSPECIFIED. ) 
 CURVE ( )  GEOMETRIC_REPRESENTATION_ITEM ( )  RATIONAL_B_SPLINE_CURVE ( ( 1.000000000000000000, 0.9238795325112867385, 1.000000000000000000, 0.9238795325112867385, 1.000000000000000000, 0.9238795325112867385, 1.000000000000000000, 0.9238795325112867385, 1.000000000000000000 ) ) 
 REPRESENTATION_ITEM ( '' )  );
#17403 = CARTESIAN_POINT ( 'NONE',  ( 162.0000000000000284, 0.000000000000000000, -6.499999999999977796 ) ) ;
#17404 = ORIENTED_EDGE ( 'NONE', *, *, #22224, .F. ) ;
#17405 = CARTESIAN_POINT ( 'NONE',  ( 115.4372167782374561, 0.7662911109078287542, -1.849990392679231599 ) ) ;
#17406 =( LENGTH_UNIT ( ) NAMED_UNIT ( * ) SI_UNIT ( .MILLI., .METRE. ) );
#17407 = CARTESIAN_POINT ( 'NONE',  ( -3.608439182435052128, -6.250000000000110134, -96.44198729810780435 ) ) ;
#17408 = CARTESIAN_POINT ( 'NONE',  ( 5.196152422706629359, -2.999999999999988898, -78.21132486540521711 ) ) ;
#17409 = CARTESIAN_POINT ( 'NONE',  ( 20.77382486540531303, 2.500000000000144773, 1.035533905932689347 ) ) ;
#17410 = CARTESIAN_POINT ( 'NONE',  ( 114.0624999999997300, 2.500000000000115019, 1.035533905932989551 ) ) ;
#17411 = DIRECTION ( 'NONE',  ( 0.000000000000000000, 0.000000000000000000, 1.000000000000000000 ) ) ;
#17412 = CARTESIAN_POINT ( 'NONE',  ( 140.1656963055991127, -11.58284815279920110, 4.440052304730676802 ) ) ;
#17413 = AXIS2_PLACEMENT_3D ( 'NONE', #1184, #4219, #12613 ) ;
#17414 = CARTESIAN_POINT ( 'NONE',  ( 25.00000000000015987, -1.873492889144789952, -1.873492889145123019 ) ) ;
#17415 = VERTEX_POINT ( 'NONE', #25621 ) ;
#17416 = CARTESIAN_POINT ( 'NONE',  ( 18.60117513459491434, -1.035533905932749299, 2.499999999999964473 ) ) ;
#17417 = CARTESIAN_POINT ( 'NONE',  ( 3.175426480543072749, 5.499999999999865885, -55.62500000000003553 ) ) ;
#17418 = ADVANCED_FACE ( 'NONE', ( #4574 ), #13999, .F. ) ;
#17419 = LINE ( 'NONE', #1242, #3749 ) ;
#17420 = CARTESIAN_POINT ( 'NONE',  ( -5.196152422706573404, -3.000000000000002665, -51.71132486540519579 ) ) ;
#17421 = CARTESIAN_POINT ( 'NONE',  ( 5.412658773652739619, 3.124999999999988898, -78.68301270189226670 ) ) ;
#17422 = DIRECTION ( 'NONE',  ( 1.000000000000000000, -5.551115123125774690E-17, 0.000000000000000000 ) ) ;
#17423 = CARTESIAN_POINT ( 'NONE',  ( 158.4226497308104058, 5.000000000000004441, 0.000000000000000000 ) ) ;
#17424 = DIRECTION ( 'NONE',  ( -0.000000000000000000, -1.000000000000000000, -0.000000000000000000 ) ) ;
#17425 = EDGE_CURVE ( 'NONE', #30226, #20441, #19473, .T. ) ;
#17426 = CARTESIAN_POINT ( 'NONE',  ( 3.175426480543072749, 5.499999999999865885, -129.1250000000000284 ) ) ;
#17427 = CARTESIAN_POINT ( 'NONE',  ( -5.999999999999904965, -1.607695154586834541, -177.7693375672974412 ) ) ;
#17428 = CARTESIAN_POINT ( 'NONE',  ( -5.999999999999963585, -1.487416814333745711E-14, -71.33632486540521711 ) ) ;
#17429 = CARTESIAN_POINT ( 'NONE',  ( 6.000000000000000888, -1.859271017917181981E-14, -67.58632486540523132 ) ) ;
#17430 = CARTESIAN_POINT ( 'NONE',  ( 0.000000000000000000, 5.499999999999991118, -72.00000000000001421 ) ) ;
#17431 = LINE ( 'NONE', #8647, #28120 ) ;
#17432 = CARTESIAN_POINT ( 'NONE',  ( -4.763139720814407951, 2.749999999999946709, -61.25000000000002842 ) ) ;
#17433 = DIRECTION ( 'NONE',  ( 0.000000000000000000, 0.000000000000000000, -1.000000000000000000 ) ) ;
#17434 = ORIENTED_EDGE ( 'NONE', *, *, #17887, .T. ) ;
#17435 = CARTESIAN_POINT ( 'NONE',  ( 153.7500000000000284, -6.000000000000005329, 0.000000000000000000 ) ) ;
#17436 = DIRECTION ( 'NONE',  ( -1.000000000000000000, -1.665334536937736783E-16, -2.220446049250315546E-16 ) ) ;
#17437 = CARTESIAN_POINT ( 'NONE',  ( 14.18749999999996270, 0.8284271247462955401, 2.000000000000031530 ) ) ;
#17438 = CARTESIAN_POINT ( 'NONE',  ( 115.0863248654050608, -1.414213562373090038, 1.414213562373256572 ) ) ;
#17439 = CARTESIAN_POINT ( 'NONE',  ( 111.7497167782375129, 1.308140751793751555, 1.308140751793973600 ) ) ;
#17440 = EDGE_LOOP ( 'NONE', ( #12401, #1014, #26718, #28570 ) ) ;
#17441 = CARTESIAN_POINT ( 'NONE',  ( 145.2187500000000000, 2.485281374238555774, -6.000000000000005329 ) ) ;
#17442 = CARTESIAN_POINT ( 'NONE',  ( 161.3226222142385495, -5.782726518792725479, 0.7502167045361700648 ) ) ;
#17443 = AXIS2_PLACEMENT_3D ( 'NONE', #9342, #23183, #15989 ) ;
#17444 =( BOUNDED_CURVE ( )  B_SPLINE_CURVE ( 2, ( #27450, #8750, #29464, #25306, #15544, #5969, #29622, #22730, #8266 ),
 .UNSPECIFIED., .F., .F. ) 
 B_SPLINE_CURVE_WITH_KNOTS ( ( 3, 2, 2, 2, 3 ),
 ( 0.6124999999999991562, 0.6187499999999994671, 0.6249999999999996669, 0.6312499999999998668, 0.6375000000000001776 ),
 .UNSPECIFIED. ) 
 CURVE ( )  GEOMETRIC_REPRESENTATION_ITEM ( )  RATIONAL_B_SPLINE_CURVE ( ( 1.000000000000010880, 0.9238795325112759693, 1.000000000000000000, 0.9238795325112867385, 1.000000000000000000, 0.9238795325112867385, 1.000000000000000000, 0.9238795325112840739, 1.000000000000002665 ) ) 
 REPRESENTATION_ITEM ( '' )  );
#17445 = CARTESIAN_POINT ( 'NONE',  ( 4.763139720814407951, -2.749999999999988454, -143.0000000000000284 ) ) ;
#17446 = CARTESIAN_POINT ( 'NONE',  ( 4.763139720814407951, 2.750000000000002665, -175.7500000000000284 ) ) ;
#17447 = CARTESIAN_POINT ( 'NONE',  ( 16.93750000000001421, 2.000000000000151879, -0.8284271247462354770 ) ) ;
#17448 = VERTEX_POINT ( 'NONE', #12137 ) ;
#17449 = CARTESIAN_POINT ( 'NONE',  ( -3.608439182435115633, 6.249999999999965361, -150.9419872981077901 ) ) ;
#17450 = CARTESIAN_POINT ( 'NONE',  ( 3.175426480543072749, -5.500000000000105693, -80.12500000000002842 ) ) ;
#17451 = EDGE_CURVE ( 'NONE', #2002, #1706, #19327, .T. ) ;
#17452 = ADVANCED_FACE ( 'NONE', ( #12428 ), #19612, .T. ) ;
#17453 = CARTESIAN_POINT ( 'NONE',  ( -5.412658773652739619, 3.124999999999975131, -97.68301270189222407 ) ) ;
#17454 = ORIENTED_EDGE ( 'NONE', *, *, #271, .T. ) ;
#17455 = CIRCLE ( 'NONE', #9596, 1.000000000000000888 ) ;
#17456 = CARTESIAN_POINT ( 'NONE',  ( 6.000000000000052403, -1.607695154586662678, -96.15331216351300725 ) ) ;
#17457 = CARTESIAN_POINT ( 'NONE',  ( 3.464101615137757051, -5.999999999999979572, -150.9136751345947971 ) ) ;
#17458 = CARTESIAN_POINT ( 'NONE',  ( 135.5572654074498757, -8.633464121020763216, -8.190187016698715183 ) ) ;
#17459 = CARTESIAN_POINT ( 'NONE',  ( 135.0583403565103993, -7.808325495672431948, 8.343593232207838994 ) ) ;
#17460 = CARTESIAN_POINT ( 'NONE',  ( 4.763139720814407951, -2.749999999999988454, -164.0000000000000284 ) ) ;
#17461 = CARTESIAN_POINT ( 'NONE',  ( -2.775557561562891351E-14, -5.500000000000115463, -146.2500000000000000 ) ) ;
#17462 = DIRECTION ( 'NONE',  ( -7.147005652999508048E-36, 5.642372883946980038E-36, 1.000000000000000000 ) ) ;
#17463 = SURFACE_SIDE_STYLE ('',( #17617 ) ) ;
#17464 = CARTESIAN_POINT ( 'NONE',  ( 4.763139720814407951, 2.750000000000002665, -94.75000000000000000 ) ) ;
#17465 = CARTESIAN_POINT ( 'NONE',  ( 104.3747167782376124, -5.551115123125782702E-14, -1.849990392679523588 ) ) ;
#17466 = DIRECTION ( 'NONE',  ( 1.000000000000000000, -5.551115123125773458E-17, -1.260129944081490338E-35 ) ) ;
#17467 = CARTESIAN_POINT ( 'NONE',  ( -3.175426480542816510, -5.500000000000057732, -84.87500000000004263 ) ) ;
#17468 = CARTESIAN_POINT ( 'NONE',  ( 5.196152422706629359, -2.999999999999988898, -72.21132486540521711 ) ) ;
#17469 = CARTESIAN_POINT ( 'NONE',  ( 151.9761751345948255, 3.889087296526011706, 3.889087296526011706 ) ) ;
#17470 = CARTESIAN_POINT ( 'NONE',  ( -5.196152422706601826, 2.999999999999975131, -131.4613248654052313 ) ) ;
#17471 = CARTESIAN_POINT ( 'NONE',  ( 21.50000000000004619, -1.999999999999890754, -1.665334536937734811E-13 ) ) ;
#17472 = CARTESIAN_POINT ( 'NONE',  ( 10.58632486540522777, 1.767766952966487448, -1.767766952966487448 ) ) ;
#17473 = DIRECTION ( 'NONE',  ( -1.000000000000000000, -1.665334536937736783E-16, -2.220446049250315546E-16 ) ) ;
#17474 = CARTESIAN_POINT ( 'NONE',  ( 0.000000000000000000, 0.000000000000000000, 0.000000000000000000 ) ) ;
#17475 = VERTEX_POINT ( 'NONE', #26502 ) ;
#17476 = CARTESIAN_POINT ( 'NONE',  ( 4.000000000000003553, -2.220446049250311602E-16, -180.0000000000000568 ) ) ;
#17477 = DIRECTION ( 'NONE',  ( -7.147005652999508048E-36, 5.642372883946980038E-36, 1.000000000000000000 ) ) ;
#17478 = CARTESIAN_POINT ( 'NONE',  ( -5.999999999999963585, 1.780251999655701777E-13, -82.41367513459481131 ) ) ;
#17479 = CARTESIAN_POINT ( 'NONE',  ( 104.4997167782375413, 1.308140751793668288, -1.308140751793640533 ) ) ;
#17480 = VECTOR ( 'NONE', #4550, 1000.000000000000000 ) ;
#17481 = CARTESIAN_POINT ( 'NONE',  ( 24.88665106358411094, 0.9137963255674127483, -1.910487928109039002 ) ) ;
#17482 = ORIENTED_EDGE ( 'NONE', *, *, #6477, .T. ) ;
#17483 =( BOUNDED_CURVE ( )  B_SPLINE_CURVE ( 2, ( #19175, #14721, #3009, #10102, #28507, #10255, #28802, #7335, #7764 ),
 .UNSPECIFIED., .F., .T. ) 
 B_SPLINE_CURVE_WITH_KNOTS ( ( 3, 2, 2, 2, 3 ),
 ( 0.01944444444444445169, 0.02037037037037037202, 0.02222222222222222307, 0.02407407407407407413, 0.02499999999999999445 ),
 .UNSPECIFIED. ) 
 CURVE ( )  GEOMETRIC_REPRESENTATION_ITEM ( )  RATIONAL_B_SPLINE_CURVE ( ( 0.9330127018922194093, 0.9330127018922198534, 1.000000000000000000, 0.8660254037844388186, 1.000000000000000000, 0.8660254037844388186, 1.000000000000000000, 0.9330127018922198534, 0.9330127018922195203 ) ) 
 REPRESENTATION_ITEM ( '' )  );
#17484 = ORIENTED_EDGE ( 'NONE', *, *, #4238, .F. ) ;
#17485 = CARTESIAN_POINT ( 'NONE',  ( -4.763139720814407951, 2.749999999999946709, -109.2500000000000142 ) ) ;
#17486 = EDGE_CURVE ( 'NONE', #17588, #22916, #20519, .T. ) ;
#17487 = CARTESIAN_POINT ( 'NONE',  ( 2.775557561562891351E-14, 6.250000000000033751, -117.4330127018922099 ) ) ;
#17488 =( BOUNDED_CURVE ( )  B_SPLINE_CURVE ( 2, ( #13013, #10700, #17770, #22515, #27089, #1447, #27240, #10855, #27999 ),
 .UNSPECIFIED., .F., .T. ) 
 B_SPLINE_CURVE_WITH_KNOTS ( ( 3, 2, 2, 2, 3 ),
 ( 0.7027777777777777235, 0.7037037037037037202, 0.7055555555555556024, 0.7074074074074073737, 0.7083333333333333703 ),
 .UNSPECIFIED. ) 
 CURVE ( )  GEOMETRIC_REPRESENTATION_ITEM ( )  RATIONAL_B_SPLINE_CURVE ( ( 0.9330127018922194093, 0.9330127018922154125, 1.000000000000000000, 0.8660254037844388186, 1.000000000000000000, 0.8660254037844388186, 1.000000000000000000, 0.9330127018922154125, 0.9330127018922194093 ) ) 
 REPRESENTATION_ITEM ( '' )  );
#17489 = EDGE_LOOP ( 'NONE', ( #4752, #16786, #26609, #14867 ) ) ;
#17490 = CARTESIAN_POINT ( 'NONE',  ( 113.7113248654051034, 2.000000000000057288, 0.000000000000000000 ) ) ;
#17491 = CARTESIAN_POINT ( 'NONE',  ( -3.608439182435052128, -6.250000000000110134, -156.4419872981078470 ) ) ;
#17492 = FACE_OUTER_BOUND ( 'NONE', #16085, .T. ) ;
#17493 = CARTESIAN_POINT ( 'NONE',  ( 147.4761751345948255, 3.889087296526011706, 3.889087296526011706 ) ) ;
#17494 = EDGE_LOOP ( 'NONE', ( #17368, #19332, #9981, #28102 ) ) ;
#17495 = CARTESIAN_POINT ( 'NONE',  ( 3.464101615137852974, 5.999999999999884537, -99.41367513459482552 ) ) ;
#17496 = CARTESIAN_POINT ( 'NONE',  ( 0.000000000000000000, -5.999999999999991118, -61.96132486540523132 ) ) ;
#17497 = DIRECTION ( 'NONE',  ( -0.000000000000000000, -0.000000000000000000, -1.000000000000000000 ) ) ;
#17498 = CARTESIAN_POINT ( 'NONE',  ( 4.763139720814407951, 2.750000000000002665, -169.7500000000000000 ) ) ;
#17499 = CARTESIAN_POINT ( 'NONE',  ( 118.3749999999999147, -1.767766952966293159, 1.767766952966431937 ) ) ;
#17500 =( LENGTH_UNIT ( ) NAMED_UNIT ( * ) SI_UNIT ( .MILLI., .METRE. ) );
#17501 = CARTESIAN_POINT ( 'NONE',  ( -5.412658773652739619, 3.124999999999975131, -172.6830127018922383 ) ) ;
#17502 = CARTESIAN_POINT ( 'NONE',  ( 154.5863248654052313, 0.000000000000000000, 5.500000000000005329 ) ) ;
#17503 = CARTESIAN_POINT ( 'NONE',  ( 24.00000000000013145, 2.000000000000057288, -1.665334536937734811E-13 ) ) ;
#17504 = CARTESIAN_POINT ( 'NONE',  ( 4.763139720814407951, -2.749999999999988454, -117.5000000000000426 ) ) ;
#17505 = CARTESIAN_POINT ( 'NONE',  ( 135.3537157487436673, -8.430252226432825680, 8.227605494166098765 ) ) ;
#17506 = CIRCLE ( 'NONE', #18002, 0.5000000000000004441 ) ;
#17507 = CARTESIAN_POINT ( 'NONE',  ( 4.763139720814407951, 2.750000000000002665, -102.2500000000000142 ) ) ;
#17508 = DIRECTION ( 'NONE',  ( -7.147005652999508048E-36, 5.642372883946980038E-36, 1.000000000000000000 ) ) ;
#17509 =( LENGTH_UNIT ( ) NAMED_UNIT ( * ) SI_UNIT ( .MILLI., .METRE. ) );
#17510 = CARTESIAN_POINT ( 'NONE',  ( -5.999999999999963585, 1.780251999655701777E-13, -82.41367513459481131 ) ) ;
#17511 = ORIENTED_EDGE ( 'NONE', *, *, #26950, .F. ) ;
#17512 = CARTESIAN_POINT ( 'NONE',  ( 15.25000000000012434, -1.873492889144789952, -1.873492889145123019 ) ) ;
#17513 = CARTESIAN_POINT ( 'NONE',  ( 119.2499999999999574, -5.551115123125782702E-14, 2.500000000000168754 ) ) ;
#17514 = DIRECTION ( 'NONE',  ( 0.000000000000000000, -1.000000000000000000, 0.000000000000000000 ) ) ;
#17515 = ORIENTED_EDGE ( 'NONE', *, *, #13622, .T. ) ;
#17516 = CARTESIAN_POINT ( 'NONE',  ( 4.763139720814407951, -2.749999999999988454, -159.5000000000000284 ) ) ;
#17517 = EDGE_CURVE ( 'NONE', #22382, #7050, #17483, .T. ) ;
#17518 = CARTESIAN_POINT ( 'NONE',  ( 5.412658773652739619, 3.124999999999988898, -79.31698729810781856 ) ) ;
#17519 = CARTESIAN_POINT ( 'NONE',  ( -5.999999999999963585, -1.487416814333745711E-14, -97.41367513459481131 ) ) ;
#17520 = ORIENTED_EDGE ( 'NONE', *, *, #27637, .T. ) ;
#17521 = COLOUR_RGB ( '', 0.66274510, 0.83137255, 0.94901961) ;
#17522 = CARTESIAN_POINT ( 'NONE',  ( 24.95539562619975271, 2.044604373800484876, -0.2498804828010667833 ) ) ;
#17523 = AXIS2_PLACEMENT_3D ( 'NONE', #6313, #8473, #6777 ) ;
#17524 = ORIENTED_EDGE ( 'NONE', *, *, #713, .F. ) ;
#17525 = VERTEX_POINT ( 'NONE', #21324 ) ;
#17526 = CARTESIAN_POINT ( 'NONE',  ( 133.5148502691896510, -3.535533905932725318, -3.535533905932725318 ) ) ;
#17527 = ADVANCED_FACE ( 'NONE', ( #5456 ), #9796, .T. ) ;
#17528 = CARTESIAN_POINT ( 'NONE',  ( 5.412658773652712085, -3.125000000000086153, -137.4330127018922383 ) ) ;
#17529 = ORIENTED_EDGE ( 'NONE', *, *, #5433, .F. ) ;
#17530 = CARTESIAN_POINT ( 'NONE',  ( 7.216878364870455975, -6.409875621278545621E-14, -128.9419872981078186 ) ) ;
#17531 = CARTESIAN_POINT ( 'NONE',  ( 113.7113248654051034, 2.000000000000057288, 0.000000000000000000 ) ) ;
#17532 = CARTESIAN_POINT ( 'NONE',  ( -2.775557561562891351E-14, -5.500000000000115463, -170.2500000000000000 ) ) ;
#17533 = CARTESIAN_POINT ( 'NONE',  ( 5.196152422706629359, -2.999999999999988898, -167.2886751345948255 ) ) ;
#17534 = ORIENTED_EDGE ( 'NONE', *, *, #15526, .F. ) ;
#17535 = CARTESIAN_POINT ( 'NONE',  ( 14.31250000000002132, -0.8284271247461152399, 2.000000000000151879 ) ) ;
#17536 = CARTESIAN_POINT ( 'NONE',  ( -2.081668171172168020E-16, -5.204170427930420051E-17, 2.499999999999999112 ) ) ;
#17537 = SURFACE_STYLE_USAGE ( .BOTH. , #12492 ) ;
#17538 = CARTESIAN_POINT ( 'NONE',  ( -3.464101615137725076, 5.999999999999979572, -171.1636751345948255 ) ) ;
#17539 = CARTESIAN_POINT ( 'NONE',  ( 13.78867513459489125, -2.499999999999780176, -1.110223024625156540E-13 ) ) ;
#17540 = CARTESIAN_POINT ( 'NONE',  ( 5.412658773652739619, 3.124999999999988898, -71.81698729810781856 ) ) ;
#17541 = CARTESIAN_POINT ( 'NONE',  ( 3.464101615137757051, -5.999999999999979572, -162.3363248654052313 ) ) ;
#17542 = LINE ( 'NONE', #5989, #8209 ) ;
#17543 = FACE_OUTER_BOUND ( 'NONE', #16892, .T. ) ;
#17544 = AXIS2_PLACEMENT_3D ( 'NONE', #21883, #821, #7880 ) ;
#17545 = VECTOR ( 'NONE', #27335, 1000.000000000000000 ) ;
#17546 = CARTESIAN_POINT ( 'NONE',  ( 3.175426480543072749, 5.499999999999865885, -126.1250000000000426 ) ) ;
#17547 = CARTESIAN_POINT ( 'NONE',  ( 5.196152422706629359, 3.000000000000002665, -167.0386751345947971 ) ) ;
#17548 = STYLED_ITEM ( 'NONE', ( #1309 ), #7074 ) ;
#17549 = VERTEX_POINT ( 'NONE', #9949 ) ;
#17550 = CARTESIAN_POINT ( 'NONE',  ( -3.464101615137725076, 5.999999999999979572, -132.1636751345948539 ) ) ;
#17551 = CARTESIAN_POINT ( 'NONE',  ( 17.53867513459494987, 1.665334536937734811E-13, 2.499999999999946709 ) ) ;
#17552 = CARTESIAN_POINT ( 'NONE',  ( -6.000000000000000888, 1.067854986875958443E-15, 7.560779664488942560E-35 ) ) ;
#17553 = CARTESIAN_POINT ( 'NONE',  ( 112.6011751345947545, -0.8284271247462053900, 2.000000000000151879 ) ) ;
#17554 = CARTESIAN_POINT ( 'NONE',  ( 0.9172842643931518047, -15.89806073124487540, 7.323133569090728656 ) ) ;
#17555 = VERTEX_POINT ( 'NONE', #21481 ) ;
#17556 = AXIS2_PLACEMENT_3D ( 'NONE', #28174, #7144, #23599 ) ;
#17557 = CARTESIAN_POINT ( 'NONE',  ( 112.3122167782374987, -0.7662911109076785410, -1.849990392679291551 ) ) ;
#17558 = FILL_AREA_STYLE ('',( #19988 ) ) ;
#17559 = EDGE_CURVE ( 'NONE', #3582, #5384, #7476, .T. ) ;
#17560 = CARTESIAN_POINT ( 'NONE',  ( -3.608439182435052128, -6.250000000000110134, -94.94198729810780435 ) ) ;
#17561 = CARTESIAN_POINT ( 'NONE',  ( -5.196152422706573404, -3.000000000000002665, -54.71132486540519579 ) ) ;
#17562 = CARTESIAN_POINT ( 'NONE',  ( 0.000000000000000000, 0.000000000000000000, 0.000000000000000000 ) ) ;
#17563 = CARTESIAN_POINT ( 'NONE',  ( 113.6249999999998721, -1.767766952966376426, -1.767766952966431937 ) ) ;
#17564 = CARTESIAN_POINT ( 'NONE',  ( 140.1944936379391322, -11.19449363793818542, 4.371599137206779062 ) ) ;
#17565 = COLOUR_RGB ( '', 0.08235294, 0.09019608, 0.10196078) ;
#17566 = EDGE_CURVE ( 'NONE', #13568, #22235, #18086, .T. ) ;
#17567 = ADVANCED_FACE ( 'NONE', ( #267, #21922 ), #28954, .T. ) ;
#17568 = CARTESIAN_POINT ( 'NONE',  ( -5.999999999999963585, -1.487416814333745711E-14, -80.91367513459482552 ) ) ;
#17569 = CARTESIAN_POINT ( 'NONE',  ( 4.763139720814407951, 2.750000000000002665, -46.75000000000001421 ) ) ;
#17570 = CARTESIAN_POINT ( 'NONE',  ( 6.000000000000052403, -1.607695154586662678, -62.23066243270258724 ) ) ;
#17571 = CARTESIAN_POINT ( 'NONE',  ( 5.412658773652739619, 3.124999999999988898, -75.68301270189226670 ) ) ;
#17572 = CARTESIAN_POINT ( 'NONE',  ( -5.999999999999963585, -1.487416814333745711E-14, -143.3363248654052029 ) ) ;
#17573 = CARTESIAN_POINT ( 'NONE',  ( 148.2038997308104342, 2.071067811865468400, 4.999999999999989342 ) ) ;
#17574 = LINE ( 'NONE', #15272, #9917 ) ;
#17575 = TOROIDAL_SURFACE ( 'NONE', #27818, 14.49999999999999822, 0.5000000000000000000 ) ;
#17576 = CARTESIAN_POINT ( 'NONE',  ( 0.000000000000000000, 0.000000000000000000, -44.99152654425658682 ) ) ;
#17577 = CARTESIAN_POINT ( 'NONE',  ( -5.999999999999963585, 1.780251999655701777E-13, -79.41367513459482552 ) ) ;
#17578 = CARTESIAN_POINT ( 'NONE',  ( 6.000000000000000888, 1.743066579297358182E-13, -113.1636751345948397 ) ) ;
#17579 =( BOUNDED_SURFACE ( )  B_SPLINE_SURFACE ( 3, 2, ( 
 ( #30085, #8439, #27609 ),
 ( #15700, #20125, #18445 ),
 ( #16159, #25309, #6425 ),
 ( #13095, #22429, #27313 ),
 ( #18295, #1367, #3964 ),
 ( #10777, #17844, #6586 ),
 ( #13391, #27164, #22734 ),
 ( #20578, #1677, #24866 ),
 ( #8754, #4122, #13544 ),
 ( #22883, #11545, #13858 ),
 ( #4432, #25468, #2145 ),
 ( #23198, #10561, #17638 ) ),
 .UNSPECIFIED., .F., .F., .T. ) 
 B_SPLINE_SURFACE_WITH_KNOTS ( ( 4, 2, 2, 2, 2, 4 ),
 ( 3, 3 ),
 ( 0.001274372683696326294, 0.001674986756246988479, 0.002075600828797650663, 0.002876828973898974597, 0.003678057119000298532, 0.004479285264101622900 ),
 ( 0.000000000000000000, 1.000000000000000000 ),
 .UNSPECIFIED. ) 
 GEOMETRIC_REPRESENTATION_ITEM ( )  RATIONAL_B_SPLINE_SURFACE ( (
 ( 1.000000000000000000, 0.8320502943378437211, 1.000000000000000000),
 ( 1.000000000000000000, 0.8320475279104844191, 1.000000000000000000),
 ( 1.000000000000000000, 0.8309444048799978777, 1.000000000000000000),
 ( 1.000000000000000000, 0.8266812726961745295, 1.000000000000000000),
 ( 1.000000000000000000, 0.8234657432881781203, 1.000000000000000000),
 ( 1.000000000000000000, 0.8113071453214155682, 1.000000000000000000),
 ( 1.000000000000000000, 0.7996314351500605211, 1.000000000000000000),
 ( 1.000000000000000000, 0.7734282707767409226, 1.000000000000000000),
 ( 1.000000000000000000, 0.7587203540637079691, 1.000000000000000000),
 ( 1.000000000000000000, 0.7309429981451178726, 1.000000000000000000),
 ( 1.000000000000000000, 0.7175754434900719625, 1.000000000000000000),
 ( 1.000000000000000000, 0.7071067811865474617, 1.000000000000000000) ) ) 
 REPRESENTATION_ITEM ( '' )  SURFACE ( )  );
#17580 = CARTESIAN_POINT ( 'NONE',  ( 6.350852961086080661, -9.614813431917819062E-14, -129.3750000000000284 ) ) ;
#17581 = CARTESIAN_POINT ( 'NONE',  ( 10.28867513459494276, 2.500000000000057732, -1.665334536937734811E-13 ) ) ;
#17582 = CARTESIAN_POINT ( 'NONE',  ( -3.464101615137757051, -5.999999999999979572, -71.08632486540520290 ) ) ;
#17583 = COLOUR_RGB ( '', 0.72549020, 0.75294118, 0.79215686) ;
#17584 = CARTESIAN_POINT ( 'NONE',  ( 6.350852961086080661, -9.614813431917819062E-14, -63.37500000000001421 ) ) ;
#17585 = CARTESIAN_POINT ( 'NONE',  ( 4.763139720814407951, 2.750000000000002665, -55.75000000000002132 ) ) ;
#17586 = AXIS2_PLACEMENT_3D ( 'NONE', #26273, #9713, #21691 ) ;
#17587 = CARTESIAN_POINT ( 'NONE',  ( 5.196152422706629359, -2.999999999999988898, -174.2113248654052597 ) ) ;
#17588 = VERTEX_POINT ( 'NONE', #20067 ) ;
#17589 = CARTESIAN_POINT ( 'NONE',  ( 144.9375000000000284, -4.242640687119298093, -4.242640687119298093 ) ) ;
#17590 = CYLINDRICAL_SURFACE ( 'NONE', #25624, 6.000000000000000888 ) ;
#17591 = CARTESIAN_POINT ( 'NONE',  ( 13.93750000000017941, 2.000000000000151879, -0.8284271247462354770 ) ) ;
#17592 = ADVANCED_FACE ( 'NONE', ( #3912 ), #11024, .T. ) ;
#17593 = CARTESIAN_POINT ( 'NONE',  ( -5.196152422706573404, -3.000000000000002665, -89.21132486540523132 ) ) ;
#17594 = CARTESIAN_POINT ( 'NONE',  ( 111.4372167782375271, 0.7662911109078888172, -1.849990392679231599 ) ) ;
#17595 = ORIENTED_EDGE ( 'NONE', *, *, #14496, .F. ) ;
#17596 = CARTESIAN_POINT ( 'NONE',  ( 144.9375000000000284, -4.242640687119298093, -4.242640687119298093 ) ) ;
#17597 = CARTESIAN_POINT ( 'NONE',  ( 161.4683586609244799, -4.012149146953796652, -4.464357517409463405 ) ) ;
#17598 = ORIENTED_EDGE ( 'NONE', *, *, #13407, .T. ) ;
#17599 = EDGE_CURVE ( 'NONE', #10564, #5997, #30199, .T. ) ;
#17600 = CARTESIAN_POINT ( 'NONE',  ( -4.763139720814407951, 2.749999999999946709, -143.7500000000000568 ) ) ;
#17601 = CARTESIAN_POINT ( 'NONE',  ( 2.775557561562891351E-14, 6.250000000000033751, -49.06698729810782567 ) ) ;
#17602 = CARTESIAN_POINT ( 'NONE',  ( 16.18750000000014566, 0.8284271247462955401, 2.000000000000031530 ) ) ;
#17603 = EDGE_LOOP ( 'NONE', ( #17265, #16490, #19135, #16714 ) ) ;
#17604 = CARTESIAN_POINT ( 'NONE',  ( 7.216878364870455975, -6.409875621278545621E-14, -143.9419872981078470 ) ) ;
#17605 = CARTESIAN_POINT ( 'NONE',  ( 6.350852961086080661, -9.614813431917819062E-14, -76.87500000000000000 ) ) ;
#17606 = CARTESIAN_POINT ( 'NONE',  ( 15.00000000000015277, -1.873492889144845464, -1.873492889145011997 ) ) ;
#17607 = CARTESIAN_POINT ( 'NONE',  ( 5.412658773652739619, 3.124999999999988898, -98.18301270189222407 ) ) ;
#17608 = CARTESIAN_POINT ( 'NONE',  ( -4.763139720814407951, 2.749999999999946709, -152.7500000000000568 ) ) ;
#17609 = CARTESIAN_POINT ( 'NONE',  ( 0.000000000000000000, 5.999999999999977796, -175.7886751345948539 ) ) ;
#17610 = LINE ( 'NONE', #10532, #29726 ) ;
#17611 = CARTESIAN_POINT ( 'NONE',  ( 140.0255071013316410, -11.51275355066580453, -4.738782956804194590 ) ) ;
#17612 = CARTESIAN_POINT ( 'NONE',  ( 110.2886751345946834, 2.000000000000085265, 1.110223024625156540E-13 ) ) ;
#17613 = CARTESIAN_POINT ( 'NONE',  ( 3.175426480543072749, 5.499999999999865885, -154.6250000000000853 ) ) ;
#17614 = CARTESIAN_POINT ( 'NONE',  ( -4.999999999999990230, -24.99999999999999289, 5.000000000000004441 ) ) ;
#17615 = CARTESIAN_POINT ( 'NONE',  ( -3.175426480542816510, -5.500000000000057732, -144.8750000000000853 ) ) ;
#17616 = CARTESIAN_POINT ( 'NONE',  ( 134.9999999999999716, 5.403404080199650572, 2.230070723382028053 ) ) ;
#17617 = SURFACE_STYLE_FILL_AREA ( #29238 ) ;
#17618 = CARTESIAN_POINT ( 'NONE',  ( 3.175426480543072749, 5.499999999999865885, -88.62500000000001421 ) ) ;
#17619 = CARTESIAN_POINT ( 'NONE',  ( 6.000000000000000888, -3.330669073875464691E-16, -7.560779664488942560E-35 ) ) ;
#17620 = CARTESIAN_POINT ( 'NONE',  ( 4.763139720814407951, 2.750000000000002665, -84.25000000000004263 ) ) ;
#17621 = DIRECTION ( 'NONE',  ( -1.000000000000000000, -1.665334536937731113E-16, 1.526556658859586792E-16 ) ) ;
#17622 = CARTESIAN_POINT ( 'NONE',  ( 150.9523502691896510, 0.000000000000000000, 5.000000000000004441 ) ) ;
#17623 = CARTESIAN_POINT ( 'NONE',  ( 0.000000000000000000, 5.999999999999977796, -142.2113248654052313 ) ) ;
#17624 = CARTESIAN_POINT ( 'NONE',  ( 150.8363248654052029, 0.000000000000000000, -5.500000000000005329 ) ) ;
#17625 = CARTESIAN_POINT ( 'NONE',  ( 144.8363248654052029, 0.000000000000000000, -5.500000000000005329 ) ) ;
#17626 = DIRECTION ( 'NONE',  ( 1.000000000000000000, 0.000000000000000000, 0.000000000000000000 ) ) ;
#17627 = EDGE_CURVE ( 'NONE', #15465, #13349, #10244, .T. ) ;
#17628 = DIRECTION ( 'NONE',  ( 0.000000000000000000, 0.000000000000000000, -1.000000000000000000 ) ) ;
#17629 = DIRECTION ( 'NONE',  ( -5.551115123125774074E-17, -1.000000000000000000, 5.642372883946979370E-36 ) ) ;
#17630 = EDGE_CURVE ( 'NONE', #2147, #15812, #3606, .T. ) ;
#17631 = VERTEX_POINT ( 'NONE', #13340 ) ;
#17632 = CARTESIAN_POINT ( 'NONE',  ( 160.8750000000000568, 0.000000000000000000, 6.000000000000005329 ) ) ;
#17633 = CARTESIAN_POINT ( 'NONE',  ( 109.9136751345947260, -1.414213562373090038, -1.414213562373145550 ) ) ;
#17634 = CARTESIAN_POINT ( 'NONE',  ( 117.1877832217620892, 0.7662911109078287542, -1.849990392679472073 ) ) ;
#17635 = FACE_OUTER_BOUND ( 'NONE', #28916, .T. ) ;
#17636 = VERTEX_POINT ( 'NONE', #24661 ) ;
#17637 = CARTESIAN_POINT ( 'NONE',  ( 0.000000000000000000, 5.499999999999991118, -109.5000000000000426 ) ) ;
#17638 = CARTESIAN_POINT ( 'NONE',  ( 160.0000000000000284, -12.64911064067352164, 3.000000000000002220 ) ) ;
#17639 = CARTESIAN_POINT ( 'NONE',  ( 7.216878364870455975, -6.409875621278545621E-14, -117.8080127018922525 ) ) ;
#17640 = ORIENTED_EDGE ( 'NONE', *, *, #18921, .T. ) ;
#17641 = CARTESIAN_POINT ( 'NONE',  ( 5.999999999999949374, 1.607695154586804565, -92.09668783648706381 ) ) ;
#17642 = CARTESIAN_POINT ( 'NONE',  ( 105.4374999999998153, -2.499999999999994671, 1.035533905932929599 ) ) ;
#17643 = CARTESIAN_POINT ( 'NONE',  ( -3.608439182435115633, 6.249999999999965361, -49.80801270189224539 ) ) ;
#17644 = AXIS2_PLACEMENT_3D ( 'NONE', #23354, #16459, #2722 ) ;
#17645 = ORIENTED_EDGE ( 'NONE', *, *, #5555, .F. ) ;
#17646 = LINE ( 'NONE', #17349, #28045 ) ;
#17647 = CARTESIAN_POINT ( 'NONE',  ( 146.1636751345948255, 0.000000000000000000, 5.500000000000005329 ) ) ;
#17648 = CARTESIAN_POINT ( 'NONE',  ( 141.1800748654052029, -2.278174593051950136, 5.500000000000074607 ) ) ;
#17649 = CARTESIAN_POINT ( 'NONE',  ( 3.175426480543072749, -5.500000000000105693, -174.6250000000000284 ) ) ;
#17650 = CARTESIAN_POINT ( 'NONE',  ( 120.3750000000000284, -1.767766952966376426, 1.767766952966320915 ) ) ;
#17651 = CARTESIAN_POINT ( 'NONE',  ( 10.14882486540516204, -2.499999999999964473, 1.035533905932869425 ) ) ;
#17652 = CARTESIAN_POINT ( 'NONE',  ( -5.412658773652739619, 3.124999999999975131, -166.6830127018922383 ) ) ;
#17653 = CARTESIAN_POINT ( 'NONE',  ( -2.775557561562891351E-14, -5.500000000000115463, -114.7500000000000142 ) ) ;
#17654 = CARTESIAN_POINT ( 'NONE',  ( 0.000000000000000000, 0.000000000000000000, 0.000000000000000000 ) ) ;
#17655 = CARTESIAN_POINT ( 'NONE',  ( -4.763139720814407951, 2.749999999999946709, -101.7500000000000000 ) ) ;
#17656 = FACE_OUTER_BOUND ( 'NONE', #20308, .T. ) ;
#17657 = CARTESIAN_POINT ( 'NONE',  ( -3.464101615137757051, -5.999999999999979572, -87.58632486540518869 ) ) ;
#17658 =( NAMED_UNIT ( * ) SI_UNIT ( $, .STERADIAN. ) SOLID_ANGLE_UNIT ( ) );
#17659 = CARTESIAN_POINT ( 'NONE',  ( 135.0000000000000284, -9.047800747817552391, 7.500000000000007105 ) ) ;
#17660 = ORIENTED_EDGE ( 'NONE', *, *, #10809, .F. ) ;
#17661 = CARTESIAN_POINT ( 'NONE',  ( 14.56250000000001954, 2.649519052838419153, -1.097466725451499370 ) ) ;
#17662 = FACE_OUTER_BOUND ( 'NONE', #20536, .T. ) ;
#17663 = CARTESIAN_POINT ( 'NONE',  ( 161.3437500000000568, -6.000000000000005329, -2.485281374238556218 ) ) ;
#17664 = CARTESIAN_POINT ( 'NONE',  ( 111.0002832217622597, -1.308140751793557266, -1.308140751793640533 ) ) ;
#17665 =( BOUNDED_CURVE ( )  B_SPLINE_CURVE ( 2, ( #22754, #6450, #26867, #4141, #17865, #13406, #6152, #1695, #29491 ),
 .UNSPECIFIED., .F., .T. ) 
 B_SPLINE_CURVE_WITH_KNOTS ( ( 3, 2, 2, 2, 3 ),
 ( 0.5361111111111110938, 0.5370370370370369795, 0.5388888888888888618, 0.5407407407407407440, 0.5416666666666667407 ),
 .UNSPECIFIED. ) 
 CURVE ( )  GEOMETRIC_REPRESENTATION_ITEM ( )  RATIONAL_B_SPLINE_CURVE ( ( 0.9330127018922194093, 0.9330127018922194093, 1.000000000000000000, 0.8660254037844388186, 1.000000000000000000, 0.8660254037844388186, 1.000000000000000000, 0.9330127018922114157, 0.9330127018922194093 ) ) 
 REPRESENTATION_ITEM ( '' )  );
#17666 = EDGE_CURVE ( 'NONE', #6328, #7272, #26813, .T. ) ;
#17667 = VERTEX_POINT ( 'NONE', #8699 ) ;
#17668 = CARTESIAN_POINT ( 'NONE',  ( 4.763139720814407951, 2.750000000000002665, -159.2500000000000000 ) ) ;
#17669 = CARTESIAN_POINT ( 'NONE',  ( 3.608439182435180470, 6.249999999999982236, -83.69198729810780435 ) ) ;
#17670 = VECTOR ( 'NONE', #5926, 1000.000000000000000 ) ;
#17671 = VERTEX_POINT ( 'NONE', #15013 ) ;
#17672 = CARTESIAN_POINT ( 'NONE',  ( 0.000000000000000000, 0.000000000000000000, 0.000000000000000000 ) ) ;
#17673 = STYLED_ITEM ( 'NONE', ( #20551 ), #14742 ) ;
#17674 =( GEOMETRIC_REPRESENTATION_CONTEXT ( 3 ) GLOBAL_UNCERTAINTY_ASSIGNED_CONTEXT ( ( #26936 ) ) GLOBAL_UNIT_ASSIGNED_CONTEXT ( ( #17500, #27429, #10897 ) ) REPRESENTATION_CONTEXT ( 'NONE', 'WORKASPACE' ) );
#17675 = EDGE_LOOP ( 'NONE', ( #21696, #3955, #19045, #2827 ) ) ;
#17676 = ORIENTED_EDGE ( 'NONE', *, *, #12170, .F. ) ;
#17677 = CARTESIAN_POINT ( 'NONE',  ( 156.1875000000000284, 4.242640687119269671, 4.242640687119298093 ) ) ;
#17678 = CARTESIAN_POINT ( 'NONE',  ( 0.000000000000000000, 5.499999999999991118, -133.5000000000000000 ) ) ;
#17679 = CARTESIAN_POINT ( 'NONE',  ( -5.412658773652684552, -3.125000000000099920, -139.4330127018922383 ) ) ;
#17680 = VERTEX_POINT ( 'NONE', #8383 ) ;
#17681 = LINE ( 'NONE', #18136, #3114 ) ;
#17682 = CARTESIAN_POINT ( 'NONE',  ( -5.412658773652739619, 3.124999999999975131, -122.3169872981078043 ) ) ;
#17683 = CARTESIAN_POINT ( 'NONE',  ( 5.196152422706629359, -2.999999999999988898, -135.2113248654052029 ) ) ;
#17684 = CARTESIAN_POINT ( 'NONE',  ( -6.350852961085760029, -1.281975124255709124E-13, -169.1249999999999716 ) ) ;
#17685 = CARTESIAN_POINT ( 'NONE',  ( 5.196152422706629359, 3.000000000000002665, -83.96132486540520290 ) ) ;
#17686 = CARTESIAN_POINT ( 'NONE',  ( -5.999999999999963585, 8.134310703387671600E-14, -130.4136751345948539 ) ) ;
#17687 = VERTEX_POINT ( 'NONE', #27110 ) ;
#17688 = CARTESIAN_POINT ( 'NONE',  ( -0.07769256095284111929, -15.23231281889970390, -7.499999999999977796 ) ) ;
#17689 = CARTESIAN_POINT ( 'NONE',  ( -5.196152422706601826, 2.999999999999975131, -147.9613248654052597 ) ) ;
#17690 = CARTESIAN_POINT ( 'NONE',  ( 6.000000000000000888, -1.859271017917181981E-14, -168.0863248654052313 ) ) ;
#17691 = CARTESIAN_POINT ( 'NONE',  ( 6.000000000000000888, -1.859271017917181981E-14, -54.66367513459481842 ) ) ;
#17692 = CARTESIAN_POINT ( 'NONE',  ( 0.7560530053056007116, -15.51661680578449598, -8.092351268349677440 ) ) ;
#17693 = CARTESIAN_POINT ( 'NONE',  ( 113.8752832217622313, -1.849990392679523588, 0.000000000000000000 ) ) ;
#17694 = CARTESIAN_POINT ( 'NONE',  ( 3.608439182435180470, -6.249999999999997335, -64.69198729810784698 ) ) ;
#17695 = CARTESIAN_POINT ( 'NONE',  ( -3.608439182435052128, -6.250000000000110134, -55.94198729810781145 ) ) ;
#17696 = EDGE_CURVE ( 'NONE', #22958, #5354, #16589, .T. ) ;
#17697 = FACE_OUTER_BOUND ( 'NONE', #1353, .T. ) ;
#17698 = PRESENTATION_STYLE_ASSIGNMENT (( #3671 ) ) ;
#17699 = CARTESIAN_POINT ( 'NONE',  ( -4.999999999999886313, -70.00000000000001421, 8.000000000000007105 ) ) ;
#17700 = CARTESIAN_POINT ( 'NONE',  ( 0.000000000000000000, 5.499999999999991118, -130.5000000000000000 ) ) ;
#17701 = CARTESIAN_POINT ( 'NONE',  ( 6.000000000000000888, -1.859271017917181981E-14, -167.1636751345948539 ) ) ;
#17702 = ORIENTED_EDGE ( 'NONE', *, *, #5061, .F. ) ;
#17703 = CARTESIAN_POINT ( 'NONE',  ( 23.56250000000001066, 2.649519052838298805, -1.097466725451559322 ) ) ;
#17704 = CARTESIAN_POINT ( 'NONE',  ( 0.000000000000000000, 0.000000000000000000, 0.000000000000000000 ) ) ;
#17705 = CARTESIAN_POINT ( 'NONE',  ( 6.000000000000000888, 1.743066579297358182E-13, -49.58632486540520290 ) ) ;
#17706 = CARTESIAN_POINT ( 'NONE',  ( 0.000000000000000000, -10.50000000000000888, 8.500000000000007105 ) ) ;
#17707 = EDGE_CURVE ( 'NONE', #13841, #19367, #3272, .T. ) ;
#17708 = ORIENTED_EDGE ( 'NONE', *, *, #22363, .F. ) ;
#17709 = CARTESIAN_POINT ( 'NONE',  ( 114.9372167782374135, -0.7662911109077987781, 1.849990392679591977 ) ) ;
#17710 = CARTESIAN_POINT ( 'NONE',  ( 10.72617513459493388, -2.499999999999844569, 1.035533905932809473 ) ) ;
#17711 = CARTESIAN_POINT ( 'NONE',  ( 11.31250000000006395, -0.8284271247460552878, 2.000000000000031530 ) ) ;
#17712 = CARTESIAN_POINT ( 'NONE',  ( -5.412658773652739619, 3.124999999999975131, -114.8169872981078470 ) ) ;
#17713 = CARTESIAN_POINT ( 'NONE',  ( -5.999999999999963585, 1.780251999655701777E-13, -110.3363248654052029 ) ) ;
#17714 = UNCERTAINTY_MEASURE_WITH_UNIT (LENGTH_MEASURE( 1.000000000000000082E-05 ), #17303, 'distance_accuracy_value', 'NONE');
#17715 = CARTESIAN_POINT ( 'NONE',  ( 114.6874999999997158, -1.035533905932689347, -2.499999999999784173 ) ) ;
#17716 = CARTESIAN_POINT ( 'NONE',  ( -5.999999999999963585, -1.487416814333745711E-14, -55.41367513459483973 ) ) ;
#17717 = CARTESIAN_POINT ( 'NONE',  ( 143.1562500000000284, -6.000000000000005329, 2.485281374238555774 ) ) ;
#17718 = AXIS2_PLACEMENT_3D ( 'NONE', #28556, #26263, #10153 ) ;
#17719 = ORIENTED_EDGE ( 'NONE', *, *, #7803, .F. ) ;
#17720 = CARTESIAN_POINT ( 'NONE',  ( 24.43750000000014921, 2.649519052838478661, 1.097466725451499370 ) ) ;
#17721 = CARTESIAN_POINT ( 'NONE',  ( 4.763139720814407951, -2.749999999999988454, -51.49999999999999289 ) ) ;
#17722 = CARTESIAN_POINT ( 'NONE',  ( 140.9136751345948539, 0.000000000000000000, -5.500000000000005329 ) ) ;
#17723 = CARTESIAN_POINT ( 'NONE',  ( -5.999999999999963585, 9.296355089585909904E-15, -164.9136751345948255 ) ) ;
#17724 = CARTESIAN_POINT ( 'NONE',  ( 6.000000000000000888, 1.743066579297358182E-13, -60.66367513459481842 ) ) ;
#17725 = CARTESIAN_POINT ( 'NONE',  ( 2.775557561562891351E-14, 6.250000000000033751, -78.43301270189223828 ) ) ;
#17726 = CARTESIAN_POINT ( 'NONE',  ( 3.464101615137757051, -5.999999999999979572, -172.8363248654052029 ) ) ;
#17727 = AXIS2_PLACEMENT_3D ( 'NONE', #19422, #24159, #21419 ) ;
#17728 = CARTESIAN_POINT ( 'NONE',  ( 150.0788997308104058, -4.999999999999989342, 2.071067811865468400 ) ) ;
#17729 = CARTESIAN_POINT ( 'NONE',  ( 6.000000000000000888, 5.577813053751546416E-15, -177.6636751345948255 ) ) ;
#17730 = DIRECTION ( 'NONE',  ( 1.000000000000000000, -5.551115123125773458E-17, -1.260129944081490338E-35 ) ) ;
#17731 = ADVANCED_FACE ( 'NONE', ( #15493 ), #10404, .T. ) ;
#17732 = CARTESIAN_POINT ( 'NONE',  ( 5.196152422706629359, 3.000000000000002665, -104.9613248654052171 ) ) ;
#17733 = CARTESIAN_POINT ( 'NONE',  ( 0.000000000000000000, 5.499999999999991118, -133.5000000000000000 ) ) ;
#17734 = CARTESIAN_POINT ( 'NONE',  ( 105.6636751345948113, -1.414213562373117794, 1.414213562373145550 ) ) ;
#17735 = DIRECTION ( 'NONE',  ( -7.147005652999508048E-36, 5.642372883946980038E-36, 1.000000000000000000 ) ) ;
#17736 = ORIENTED_EDGE ( 'NONE', *, *, #19742, .F. ) ;
#17737 = VECTOR ( 'NONE', #6348, 1000.000000000000000 ) ;
#17738 = CARTESIAN_POINT ( 'NONE',  ( 4.763139720814407951, -2.749999999999988454, -63.50000000000000000 ) ) ;
#17739 = CARTESIAN_POINT ( 'NONE',  ( -5.999999999999963585, 1.780251999655701777E-13, -72.83632486540523132 ) ) ;
#17740 = EDGE_CURVE ( 'NONE', #1, #24992, #9218, .T. ) ;
#17741 = CARTESIAN_POINT ( 'NONE',  ( -2.775557561562891351E-14, -5.500000000000115463, -54.75000000000002132 ) ) ;
#17742 = VERTEX_POINT ( 'NONE', #13804 ) ;
#17743 = CARTESIAN_POINT ( 'NONE',  ( 108.3124999999997442, -1.035533905932629173, 2.500000000000205169 ) ) ;
#17744 = CARTESIAN_POINT ( 'NONE',  ( 147.9375000000000284, -4.242640687119298093, -4.242640687119298093 ) ) ;
#17745 = DIRECTION ( 'NONE',  ( -7.147005652999508048E-36, 5.642372883946980038E-36, 1.000000000000000000 ) ) ;
#17746 = CARTESIAN_POINT ( 'NONE',  ( 14.93750000000010303, 2.000000000000151879, -0.8284271247462955401 ) ) ;
#17747 = DIRECTION ( 'NONE',  ( 1.000000000000000000, -5.551115123125773458E-17, -1.260129944081490338E-35 ) ) ;
#17748 = ORIENTED_EDGE ( 'NONE', *, *, #25996, .T. ) ;
#17749 = CARTESIAN_POINT ( 'NONE',  ( 142.6875000000000284, 4.242640687119269671, 4.242640687119298093 ) ) ;
#17750 = CARTESIAN_POINT ( 'NONE',  ( 161.1978354363685924, -3.302530014113373102, 4.653882225248398896 ) ) ;
#17751 = AXIS2_PLACEMENT_3D ( 'NONE', #17277, #26738, #22319 ) ;
#17752 = ORIENTED_EDGE ( 'NONE', *, *, #29771, .F. ) ;
#17753 =( BOUNDED_CURVE ( )  B_SPLINE_CURVE ( 2, ( #13800, #1768, #20365, #29716, #8851, #20834, #22984, #11332, #4371 ),
 .UNSPECIFIED., .F., .F. ) 
 B_SPLINE_CURVE_WITH_KNOTS ( ( 3, 2, 2, 2, 3 ),
 ( 0.4638888888888889062, 0.4648148148148147918, 0.4666666666666666741, 0.4685185185185185008, 0.4694444444444444420 ),
 .UNSPECIFIED. ) 
 CURVE ( )  GEOMETRIC_REPRESENTATION_ITEM ( )  RATIONAL_B_SPLINE_CURVE ( ( 0.9330127018922194093, 0.9330127018922214077, 1.000000000000000000, 0.8660254037844388186, 1.000000000000000000, 0.8660254037844388186, 1.000000000000000000, 0.9330127018922194093, 0.9330127018922194093 ) ) 
 REPRESENTATION_ITEM ( '' )  );
#17754 = CARTESIAN_POINT ( 'NONE',  ( 4.763139720814407951, 2.750000000000002665, -142.7500000000000568 ) ) ;
#17755 = CARTESIAN_POINT ( 'NONE',  ( 17.18750000000013500, 0.8284271247463557142, 1.999999999999971800 ) ) ;
#17756 = ORIENTED_EDGE ( 'NONE', *, *, #24115, .T. ) ;
#17757 = CARTESIAN_POINT ( 'NONE',  ( -3.608439182435052128, -6.250000000000110134, -150.4419872981077901 ) ) ;
#17758 = CARTESIAN_POINT ( 'NONE',  ( 6.350852961086080661, -9.614813431917819062E-14, -72.37499999999998579 ) ) ;
#17759 = AXIS2_PLACEMENT_3D ( 'NONE', #16319, #23359, #2303 ) ;
#17760 = CARTESIAN_POINT ( 'NONE',  ( 14.18750000000002487, 1.097466725451559322, -2.649519052838298805 ) ) ;
#17761 = CARTESIAN_POINT ( 'NONE',  ( -5.412658773652684552, -3.125000000000099920, -95.93301270189225249 ) ) ;
#17762 =( BOUNDED_CURVE ( )  B_SPLINE_CURVE ( 2, ( #8115, #19376, #10607, #19961, #21969, #15065, #17685, #5659, #770 ),
 .UNSPECIFIED., .F., .F. ) 
 B_SPLINE_CURVE_WITH_KNOTS ( ( 3, 2, 2, 2, 3 ),
 ( 0.2750000000000000222, 0.2759259259259259078, 0.2777777777777777901, 0.2796296296296296724, 0.2805555555555555580 ),
 .UNSPECIFIED. ) 
 CURVE ( )  GEOMETRIC_REPRESENTATION_ITEM ( )  RATIONAL_B_SPLINE_CURVE ( ( 0.9330127018922194093, 0.9330127018922234061, 1.000000000000000000, 0.8660254037844388186, 1.000000000000000000, 0.8660254037844388186, 1.000000000000000000, 0.9330127018922194093, 0.9330127018922194093 ) ) 
 REPRESENTATION_ITEM ( '' )  );
#17763 = CARTESIAN_POINT ( 'NONE',  ( -2.775557561562891351E-14, -5.500000000000115463, -152.2500000000000000 ) ) ;
#17764 = CIRCLE ( 'NONE', #13864, 5.999999999999992006 ) ;
#17765 = CARTESIAN_POINT ( 'NONE',  ( 105.1011751345946124, 0.8284271247462955401, -1.999999999999731104 ) ) ;
#17766 = AXIS2_PLACEMENT_3D ( 'NONE', #17205, #15038, #17357 ) ;
#17767 = EDGE_CURVE ( 'NONE', #18127, #8549, #12385, .T. ) ;
#17768 = CARTESIAN_POINT ( 'NONE',  ( -1.000000000000000888, 9.000000000000007105, -4.000000000000003553 ) ) ;
#17769 = CARTESIAN_POINT ( 'NONE',  ( 106.4613248654051176, 5.551115123125782702E-14, -1.999999999999890754 ) ) ;
#17770 = CARTESIAN_POINT ( 'NONE',  ( -5.196152422706573404, -3.000000000000002665, -86.78867513459486815 ) ) ;
#17771 = FACE_OUTER_BOUND ( 'NONE', #15842, .T. ) ;
#17772 = APPLICATION_PROTOCOL_DEFINITION ( 'draft international standard', 'automotive_design', 1998, #9497 ) ;
#17773 = CARTESIAN_POINT ( 'NONE',  ( 6.350852961086080661, -9.614813431917819062E-14, -154.8749999999999716 ) ) ;
#17774 = CARTESIAN_POINT ( 'NONE',  ( 137.2425748654051461, -2.278174593052383567, -5.499999999999640288 ) ) ;
#17775 = CARTESIAN_POINT ( 'NONE',  ( 3.175426480543072749, -5.500000000000105693, -149.1250000000000284 ) ) ;
#17776 = CARTESIAN_POINT ( 'NONE',  ( -5.374111793511253232, 2.595803520898224637, -180.0000000000000284 ) ) ;
#17777 = UNCERTAINTY_MEASURE_WITH_UNIT (LENGTH_MEASURE( 1.000000000000000082E-05 ), #11908, 'distance_accuracy_value', 'NONE');
#17778 = CARTESIAN_POINT ( 'NONE',  ( 3.175426480543072749, -5.500000000000105693, -89.12500000000001421 ) ) ;
#17779 = CARTESIAN_POINT ( 'NONE',  ( -4.999999999999886313, -10.50000000000000888, -7.500000000000007105 ) ) ;
#17780 = ADVANCED_FACE ( 'NONE', ( #20683, #16414 ), #4377, .F. ) ;
#17781 = CARTESIAN_POINT ( 'NONE',  ( 4.763139720814407951, -2.749999999999988454, -84.50000000000001421 ) ) ;
#17782 = CARTESIAN_POINT ( 'NONE',  ( 5.999999999999949374, -1.607695154586841868, -120.1533121635130072 ) ) ;
#17783 = CARTESIAN_POINT ( 'NONE',  ( 153.2961002691896795, 2.071067811865468400, -4.999999999999989342 ) ) ;
#17784 = CARTESIAN_POINT ( 'NONE',  ( -5.999999999999963585, 1.780251999655701777E-13, -64.41367513459483973 ) ) ;
#17785 = CARTESIAN_POINT ( 'NONE',  ( 140.0000000000000853, -9.835711086345112264, -7.609525942436604851 ) ) ;
#17786 = CYLINDRICAL_SURFACE ( 'NONE', #13352, 0.5000000000000004441 ) ;
#17787 = CARTESIAN_POINT ( 'NONE',  ( -5.999999999999971578, 1.607695154586715303, -124.4806624327026014 ) ) ;
#17788 = AXIS2_PLACEMENT_3D ( 'NONE', #11900, #16503, #23244 ) ;
#17789 = CARTESIAN_POINT ( 'NONE',  ( 120.4997167782374703, 1.308140751793723799, -1.308140751793640533 ) ) ;
#17790 = DIRECTION ( 'NONE',  ( -7.147005652999508048E-36, 5.642372883946980038E-36, 1.000000000000000000 ) ) ;
#17791 = VERTEX_POINT ( 'NONE', #22990 ) ;
#17792 = CARTESIAN_POINT ( 'NONE',  ( 160.0312500000000284, -2.485281374238555774, -6.000000000000005329 ) ) ;
#17793 = CARTESIAN_POINT ( 'NONE',  ( 110.2886751345946834, 2.000000000000085265, 1.110223024625156540E-13 ) ) ;
#17794 = CARTESIAN_POINT ( 'NONE',  ( 118.3127832217620750, 1.849990392679532247, -0.7662911109075883909 ) ) ;
#17795 = ORIENTED_EDGE ( 'NONE', *, *, #8367, .F. ) ;
#17796 = CARTESIAN_POINT ( 'NONE',  ( 3.175426480543072749, 5.499999999999865885, -96.12500000000004263 ) ) ;
#17797 = CARTESIAN_POINT ( 'NONE',  ( 16.37500000000008527, 2.649519052838500421, 0.000000000000000000 ) ) ;
#17798 = CARTESIAN_POINT ( 'NONE',  ( 0.000000000000000000, 5.999999999999977796, -70.78867513459485394 ) ) ;
#17799 = CARTESIAN_POINT ( 'NONE',  ( 3.608439182435180470, 6.249999999999982236, -111.5580127018922099 ) ) ;
#17800 = ORIENTED_EDGE ( 'NONE', *, *, #22612, .T. ) ;
#17801 = CARTESIAN_POINT ( 'NONE',  ( -3.464101615137725076, 5.999999999999979572, -94.08632486540524553 ) ) ;
#17802 = DIRECTION ( 'NONE',  ( 1.000000000000000000, -0.000000000000000000, -0.000000000000000000 ) ) ;
#17803 = CARTESIAN_POINT ( 'NONE',  ( 5.196152422706629359, 3.000000000000002665, -63.53867513459482552 ) ) ;
#17804 = EDGE_CURVE ( 'NONE', #17588, #28274, #9179, .T. ) ;
#17805 = CARTESIAN_POINT ( 'NONE',  ( 5.412658773652739619, 3.124999999999988898, -50.18301270189223828 ) ) ;
#17806 = ORIENTED_EDGE ( 'NONE', *, *, #17010, .T. ) ;
#17807 = ADVANCED_FACE ( 'NONE', ( #2093 ), #23305, .T. ) ;
#17808 = CARTESIAN_POINT ( 'NONE',  ( -3.464101615137725076, 5.999999999999979572, -99.16367513459481131 ) ) ;
#17809 = LINE ( 'NONE', #25898, #13070 ) ;
#17810 = DIRECTION ( 'NONE',  ( -0.000000000000000000, -0.000000000000000000, -1.000000000000000000 ) ) ;
#17811 = CARTESIAN_POINT ( 'NONE',  ( -6.350852961085760029, -1.281975124255709124E-13, -172.1250000000000284 ) ) ;
#17812 = CARTESIAN_POINT ( 'NONE',  ( 115.2499999999998721, -5.551115123125782702E-14, 2.500000000000057732 ) ) ;
#17813 = CARTESIAN_POINT ( 'NONE',  ( 10.04463841219782694, -1.279379774532318326, 2.256154131400250673 ) ) ;
#17814 = CARTESIAN_POINT ( 'NONE',  ( 3.608439182435180470, 6.249999999999982236, -158.0580127018922667 ) ) ;
#17815 = CARTESIAN_POINT ( 'NONE',  ( -0.1262135825162392089, -9.436893208741910399, 4.496381089953947807 ) ) ;
#17816 = CARTESIAN_POINT ( 'NONE',  ( -6.350852961085760029, -1.281975124255709124E-13, -106.1250000000000426 ) ) ;
#17817 = DIRECTION ( 'NONE',  ( -7.147005652999508048E-36, 5.642372883946980038E-36, 1.000000000000000000 ) ) ;
#17818 = CARTESIAN_POINT ( 'NONE',  ( -4.763139720814407951, 2.749999999999946709, -109.2500000000000142 ) ) ;
#17819 = CARTESIAN_POINT ( 'NONE',  ( 0.000000000000000000, 5.999999999999977796, -151.7886751345948255 ) ) ;
#17820 = CARTESIAN_POINT ( 'NONE',  ( 5.999999999999988454, 1.607695154586737729, -162.5966878364870638 ) ) ;
#17821 = CARTESIAN_POINT ( 'NONE',  ( 135.0000000000000284, -7.893250067244766299, 8.123627818918411236 ) ) ;
#17822 = EDGE_LOOP ( 'NONE', ( #22449, #14693, #27782, #25041 ) ) ;
#17823 = CARTESIAN_POINT ( 'NONE',  ( 15.12500000000005507, -2.649519052838222866, 0.000000000000000000 ) ) ;
#17824 = CARTESIAN_POINT ( 'NONE',  ( 120.7499999999998721, 1.110223024625156540E-13, -2.499999999999946709 ) ) ;
#17825 = CARTESIAN_POINT ( 'NONE',  ( 109.9377832217622029, -1.849990392679472073, -0.7662911109076485650 ) ) ;
#17826 = CARTESIAN_POINT ( 'NONE',  ( 3.464101615137757051, -5.999999999999979572, -133.8363248654052313 ) ) ;
#17827 = ORIENTED_EDGE ( 'NONE', *, *, #4605, .T. ) ;
#17828 = CARTESIAN_POINT ( 'NONE',  ( -4.763139720814407951, -2.750000000000016431, -160.0000000000000284 ) ) ;
#17829 = CARTESIAN_POINT ( 'NONE',  ( -5.196152422706601826, 2.999999999999975131, -65.46132486540523132 ) ) ;
#17830 = CARTESIAN_POINT ( 'NONE',  ( 108.1872167782373850, -1.849990392679472073, -0.7662911109077087390 ) ) ;
#17831 = CARTESIAN_POINT ( 'NONE',  ( -3.608439182435052128, -6.250000000000110134, -81.44198729810780435 ) ) ;
#17832 = CARTESIAN_POINT ( 'NONE',  ( 149.7113248654052313, 5.500000000000005329, 0.000000000000000000 ) ) ;
#17833 = EDGE_LOOP ( 'NONE', ( #456, #28692 ) ) ;
#17834 = CARTESIAN_POINT ( 'NONE',  ( 5.999999999999974243, 1.607695154586759934, -144.5966878364870354 ) ) ;
#17835 = VECTOR ( 'NONE', #14057, 1000.000000000000000 ) ;
#17836 = VERTEX_POINT ( 'NONE', #6994 ) ;
#17837 = ORIENTED_EDGE ( 'NONE', *, *, #23285, .T. ) ;
#17838 = CARTESIAN_POINT ( 'NONE',  ( 155.8125000000000284, 4.242640687119298093, -4.242640687119298093 ) ) ;
#17839 = CARTESIAN_POINT ( 'NONE',  ( 3.175426480543072749, 5.499999999999865885, -120.1250000000000284 ) ) ;
#17840 = CARTESIAN_POINT ( 'NONE',  ( -3.608439182435052128, -6.250000000000110134, -140.8080127018922383 ) ) ;
#17841 = CARTESIAN_POINT ( 'NONE',  ( 5.999999999999988454, 1.607695154586737729, -161.0966878364870922 ) ) ;
#17842 = CARTESIAN_POINT ( 'NONE',  ( 3.608439182435180470, -6.249999999999997335, -126.1919872981078328 ) ) ;
#17843 = CARTESIAN_POINT ( 'NONE',  ( 6.350852961086080661, -9.614813431917819062E-14, -172.8750000000000284 ) ) ;
#17844 = CARTESIAN_POINT ( 'NONE',  ( 159.6387256973390834, -11.39945094249770108, 3.799649049763677233 ) ) ;
#17845 = SURFACE_STYLE_FILL_AREA ( #29314 ) ;
#17846 = EDGE_CURVE ( 'NONE', #10564, #226, #11804, .T. ) ;
#17847 = ORIENTED_EDGE ( 'NONE', *, *, #5092, .T. ) ;
#17848 = CARTESIAN_POINT ( 'NONE',  ( 10.81250000000001243, 0.8284271247461753029, -2.000000000000091926 ) ) ;
#17849 = LINE ( 'NONE', #17536, #16725 ) ;
#17850 = EDGE_CURVE ( 'NONE', #25850, #3562, #11211, .T. ) ;
#17851 = CARTESIAN_POINT ( 'NONE',  ( 160.0185456724816220, -11.17912010889672381, -4.362636621731123654 ) ) ;
#17852 = DIRECTION ( 'NONE',  ( -1.000000000000000000, 0.000000000000000000, 0.000000000000000000 ) ) ;
#17853 = DIRECTION ( 'NONE',  ( 1.000000000000000000, 0.000000000000000000, 0.000000000000000000 ) ) ;
#17854 = CARTESIAN_POINT ( 'NONE',  ( 115.8127832217621460, -1.849990392679472073, 0.7662911109078888172 ) ) ;
#17855 = CARTESIAN_POINT ( 'NONE',  ( -3.608439182435052128, -6.250000000000110134, -64.94198729810784698 ) ) ;
#17856 = CARTESIAN_POINT ( 'NONE',  ( 3.608439182435180470, 6.249999999999982236, -56.69198729810781145 ) ) ;
#17857 = CARTESIAN_POINT ( 'NONE',  ( -5.999999999999963585, -1.487416814333745711E-14, -170.9136751345948255 ) ) ;
#17858 = CARTESIAN_POINT ( 'NONE',  ( 119.9999999999998437, 2.265773637424566278, -0.8226836970581136166 ) ) ;
#17859 = CARTESIAN_POINT ( 'NONE',  ( -3.464101615137725076, 5.999999999999979572, -74.58632486540520290 ) ) ;
#17860 =( BOUNDED_CURVE ( )  B_SPLINE_CURVE ( 2, ( #6079, #29414, #15494, #8384, #17179, #27111, #5607, #24355, #15014 ),
 .UNSPECIFIED., .F., .T. ) 
 B_SPLINE_CURVE_WITH_KNOTS ( ( 3, 2, 2, 2, 3 ),
 ( 0.4374999999999999445, 0.4437499999999997002, 0.4499999999999994005, 0.4562499999999992673, 0.4624999999999990230 ),
 .UNSPECIFIED. ) 
 CURVE ( )  GEOMETRIC_REPRESENTATION_ITEM ( )  RATIONAL_B_SPLINE_CURVE ( ( 1.000000000000000666, 0.9238795325112860723, 1.000000000000000000, 0.9238795325112867385, 1.000000000000000000, 0.9238795325112867385, 1.000000000000000000, 0.9238795325112989509, 0.9999999999999877875 ) ) 
 REPRESENTATION_ITEM ( '' )  );
#17861 = CARTESIAN_POINT ( 'NONE',  ( -4.763139720814407951, -2.750000000000016431, -127.0000000000000000 ) ) ;
#17862 = VECTOR ( 'NONE', #5381, 1000.000000000000000 ) ;
#17863 = CARTESIAN_POINT ( 'NONE',  ( 6.000000000000000888, 1.743066579297358182E-13, -51.08632486540523132 ) ) ;
#17864 = ORIENTED_EDGE ( 'NONE', *, *, #2159, .F. ) ;
#17865 = CARTESIAN_POINT ( 'NONE',  ( 0.000000000000000000, -5.999999999999991118, -118.9613248654052313 ) ) ;
#17866 = CARTESIAN_POINT ( 'NONE',  ( 6.000000000000000888, -3.330669073875464691E-16, -7.560779664488942560E-35 ) ) ;
#17867 = CARTESIAN_POINT ( 'NONE',  ( 0.000000000000000000, 0.000000000000000000, 0.000000000000000000 ) ) ;
#17868 = CARTESIAN_POINT ( 'NONE',  ( 138.3898502691896510, 3.535533905932725318, -3.535533905932725318 ) ) ;
#17869 = ORIENTED_EDGE ( 'NONE', *, *, #19013, .F. ) ;
#17870 = CARTESIAN_POINT ( 'NONE',  ( 114.4372167782375271, 0.7662911109078588412, -1.849990392679351725 ) ) ;
#17871 = CARTESIAN_POINT ( 'NONE',  ( -5.999999999999971578, 1.607695154586715303, -71.40331216351300725 ) ) ;
#17872 = CARTESIAN_POINT ( 'NONE',  ( 113.7886751345947687, -1.999999999999918510, 0.000000000000000000 ) ) ;
#17873 = CARTESIAN_POINT ( 'NONE',  ( 2.775557561562891351E-14, 6.250000000000033751, -115.0669872981078186 ) ) ;
#17874 = CARTESIAN_POINT ( 'NONE',  ( 140.5000000328705028, -11.02580175850478383, -4.736714422037297645 ) ) ;
#17875 = CARTESIAN_POINT ( 'NONE',  ( 115.1874999999998579, 1.035533905932719101, 2.500000000000265121 ) ) ;
#17876 = ORIENTED_EDGE ( 'NONE', *, *, #7607, .T. ) ;
#17877 = CARTESIAN_POINT ( 'NONE',  ( -4.999999999999913847, -65.50000000000001421, 8.000000000000007105 ) ) ;
#17878 = EDGE_CURVE ( 'NONE', #29332, #13966, #10667, .T. ) ;
#17879 = CARTESIAN_POINT ( 'NONE',  ( 144.0000000000000284, 6.000000000000005329, 0.000000000000000000 ) ) ;
#17880 = ORIENTED_EDGE ( 'NONE', *, *, #15526, .T. ) ;
#17881 = AXIS2_PLACEMENT_3D ( 'NONE', #5078, #2781, #2931 ) ;
#17882 = CLOSED_SHELL ( 'NONE', ( #28673, #2826, #12784, #306, #17321, #12648, #24241, #24624, #23966, #28405, #4213, #23456, #9321, #15854, #23251, #6418, #25826, #1186, #15165, #16088, #25148, #18992, #10238, #27563, #14353, #23623, #24214, #11075, #4963, #23762, #1644, #5208, #814, #21478, #26268, #28537, #7807, #19222, #29979, #17731, #11003, #19096, #11034, #12998, #26485, #10626, #6467, #25387, #30155, #29861, #25954, #2014, #3086, #11658, #28750, #19853, #25112, #29566, #3682, #869, #20252, #14433, #27057, #15096, #11186, #29447, #10663, #14012, #23418, #26757, #14153, #24242, #19928, #20564, #3265, #30365, #18814, #16839, #29908, #12470, #25223, #21130, #16123, #22181, #97, #495, #1316, #21128, #2790, #15638, #2932, #5932, #26496, #298, #23357, #1585, #24428, #21675, #4535, #27858, #2483, #12472, #6263, #21196, #14187, #28772, #1252, #3565, #21368, #27645, #14672, #16394, #15954, #29760, #26151, #12540, #26432, #25747, #20995, #20846, #13489, #650, #17011, #28068, #18059, #12514, #22047, #968, #9246, #8703, #6162, #29169, #1214, #21912, #14868, #28958, #754, #20141, #17452, #3610, #26033, #15716, #20373, #25080, #15675, #13515, #21088, #16935, #24489, #5106, #19917, #8484, #26728, #4631, #18501, #8291, #3332, #23595, #13735, #18714, #23929, #28601, #8379, #8977, #11976, #10370, #5683, #7744, #28413, #8624, #7704, #10837, #21464, #3124, #22263, #17527, #10228, #10544, #11799, #16339, #11322, #7904, #975, #4798, #11259, #20915, #21519, #20531, #17567, #18784, #11533, #10731, #26979, #27855, #15276, #231, #6041, #24597, #23253, #27344 ) ) ;
#17883 = CARTESIAN_POINT ( 'NONE',  ( -4.763139720814407951, 2.749999999999946709, -149.7500000000000568 ) ) ;
#17884 = CARTESIAN_POINT ( 'NONE',  ( 3.175426480543072749, 5.499999999999865885, -46.62500000000006395 ) ) ;
#17885 = CARTESIAN_POINT ( 'NONE',  ( 135.9449251345948539, -5.500000000000012434, 2.278174593052012309 ) ) ;
#17886 = CARTESIAN_POINT ( 'NONE',  ( 7.216878364870455975, -6.409875621278545621E-14, -75.80801270189223828 ) ) ;
#17887 = EDGE_CURVE ( 'NONE', #8975, #9651, #26325, .T. ) ;
#17888 = CYLINDRICAL_SURFACE ( 'NONE', #4513, 6.000000000000000888 ) ;
#17889 = CARTESIAN_POINT ( 'NONE',  ( 152.9851497308104058, -3.535533905932725318, 3.535533905932725318 ) ) ;
#17890 = DIRECTION ( 'NONE',  ( -7.147005652999508048E-36, 5.642372883946980038E-36, 1.000000000000000000 ) ) ;
#17891 = FILL_AREA_STYLE_COLOUR ( '', #4954 ) ;
#17892 = DIRECTION ( 'NONE',  ( -7.147005652999508048E-36, 5.642372883946980038E-36, 1.000000000000000000 ) ) ;
#17893 = CARTESIAN_POINT ( 'NONE',  ( 4.763139720814407951, 2.750000000000002665, -129.2500000000000284 ) ) ;
#17894 = CARTESIAN_POINT ( 'NONE',  ( 3.608439182435180470, -6.249999999999997335, -146.5580127018922383 ) ) ;
#17895 = DIRECTION ( 'NONE',  ( -1.000000000000000000, -1.665334536937731113E-16, 1.526556658859586792E-16 ) ) ;
#17896 = ORIENTED_EDGE ( 'NONE', *, *, #18471, .F. ) ;
#17897 = CARTESIAN_POINT ( 'NONE',  ( 3.175426480543072749, -5.500000000000105693, -66.62500000000002842 ) ) ;
#17898 = DIRECTION ( 'NONE',  ( 1.000000000000000000, 1.734723475976807094E-15, 0.000000000000000000 ) ) ;
#17899 = SURFACE_STYLE_FILL_AREA ( #8331 ) ;
#17900 = VERTEX_POINT ( 'NONE', #21888 ) ;
#17901 = CARTESIAN_POINT ( 'NONE',  ( 107.6874999999997726, -1.035533905932659149, -2.499999999999724221 ) ) ;
#17902 = CARTESIAN_POINT ( 'NONE',  ( 143.8125000000000284, 4.242640687119298093, -4.242640687119298093 ) ) ;
#17903 = CARTESIAN_POINT ( 'NONE',  ( -3.464101615137757051, -5.999999999999979572, -118.1636751345948397 ) ) ;
#17904 = CARTESIAN_POINT ( 'NONE',  ( 14.62500000000008171, -1.414213562372979016, -1.414213562373145550 ) ) ;
#17905 = DIRECTION ( 'NONE',  ( 0.000000000000000000, 0.000000000000000000, -1.000000000000000000 ) ) ;
#17906 = ORIENTED_EDGE ( 'NONE', *, *, #4286, .F. ) ;
#17907 = CARTESIAN_POINT ( 'NONE',  ( 136.1250000000000284, 0.000000000000000000, -6.000000000000005329 ) ) ;
#17908 = CARTESIAN_POINT ( 'NONE',  ( 161.1037658773653050, -2.857005778783127844E-13, 5.603765877365280090 ) ) ;
#17909 = EDGE_CURVE ( 'NONE', #15017, #17667, #825, .T. ) ;
#17910 = ORIENTED_EDGE ( 'NONE', *, *, #16445, .T. ) ;
#17911 = EDGE_CURVE ( 'NONE', #1653, #15017, #15091, .T. ) ;
#17912 = CARTESIAN_POINT ( 'NONE',  ( -3.175426480542816510, 5.499999999999865885, -148.3750000000000568 ) ) ;
#17913 = B_SPLINE_CURVE_WITH_KNOTS ( 'NONE', 3,
 ( #26153, #11938, #4812, #12232 ),
 .UNSPECIFIED., .F., .F.,
 ( 4, 4 ),
 ( 0.000000000000000000, 0.0002043583609089620558 ),
 .UNSPECIFIED. ) ;
#17914 = VERTEX_POINT ( 'NONE', #2536 ) ;
#17915 = CARTESIAN_POINT ( 'NONE',  ( 18.87500000000008527, 1.414213562373256572, -1.414213562373090038 ) ) ;
#17916 = ORIENTED_EDGE ( 'NONE', *, *, #27844, .F. ) ;
#17917 = CARTESIAN_POINT ( 'NONE',  ( -4.763139720814407951, 2.749999999999946709, -71.75000000000004263 ) ) ;
#17918 = EDGE_CURVE ( 'NONE', #20178, #26967, #14371, .T. ) ;
#17919 = CARTESIAN_POINT ( 'NONE',  ( 3.608439182435180470, 6.249999999999982236, -96.55801270189228092 ) ) ;
#17920 = CARTESIAN_POINT ( 'NONE',  ( -4.520452470708151260, -10.03252783106556123, -21.03609891486514627 ) ) ;
#17921 = CARTESIAN_POINT ( 'NONE',  ( 5.196152422706629359, -2.999999999999988898, -83.28867513459481131 ) ) ;
#17922 = CARTESIAN_POINT ( 'NONE',  ( 148.1175748654052313, 5.500000000000012434, -2.278174593052012309 ) ) ;
#17923 = VECTOR ( 'NONE', #6064, 1000.000000000000000 ) ;
#17924 = CARTESIAN_POINT ( 'NONE',  ( 110.4761751345946976, 0.8284271247462354770, 2.000000000000212275 ) ) ;
#17925 = PRESENTATION_LAYER_ASSIGNMENT (  '', '', ( #14023 ) ) ;
#17926 = CARTESIAN_POINT ( 'NONE',  ( 4.763139720814407951, 2.750000000000002665, -157.7500000000000568 ) ) ;
#17927 = CARTESIAN_POINT ( 'NONE',  ( 17.64882486540520645, 2.500000000000144773, -1.035533905932929599 ) ) ;
#17928 = PLANE ( 'NONE',  #13014 ) ;
#17929 = CARTESIAN_POINT ( 'NONE',  ( 4.763139720814407951, -2.749999999999988454, -89.00000000000002842 ) ) ;
#17930 = CARTESIAN_POINT ( 'NONE',  ( 6.000000000000000888, -3.330669073875464691E-16, -7.560779664488942560E-35 ) ) ;
#17931 = CARTESIAN_POINT ( 'NONE',  ( -4.763139720814407951, 2.749999999999946709, -73.25000000000004263 ) ) ;
#17932 = CARTESIAN_POINT ( 'NONE',  ( 152.8273502691896510, -5.000000000000004441, 0.000000000000000000 ) ) ;
#17933 = CARTESIAN_POINT ( 'NONE',  ( 150.5699251345948255, 2.278174593052259667, 5.499999999999763745 ) ) ;
#17934 = CARTESIAN_POINT ( 'NONE',  ( 161.0874653000716989, -5.321804761115118687, -1.753823027392139577 ) ) ;
#17935 = CARTESIAN_POINT ( 'NONE',  ( 114.7113248654050750, 2.000000000000057288, 0.000000000000000000 ) ) ;
#17936 = TOROIDAL_SURFACE ( 'NONE', #1195, 29.00000000000000000, 1.000000000000000000 ) ;
#17937 = DIRECTION ( 'NONE',  ( -7.147005652999508048E-36, 5.642372883946980038E-36, 1.000000000000000000 ) ) ;
#17938 = CARTESIAN_POINT ( 'NONE',  ( 119.8747167782375982, 0.000000000000000000, 1.849990392679523588 ) ) ;
#17939 = CARTESIAN_POINT ( 'NONE',  ( 10.00000000000001421, -5.551115123125781716E-16, -43.99152654425658682 ) ) ;
#17940 =( BOUNDED_CURVE ( )  B_SPLINE_CURVE ( 2, ( #25474, #3973, #25313, #6592, #2304, #9208, #2151, #6896, #25165 ),
 .UNSPECIFIED., .F., .F. ) 
 B_SPLINE_CURVE_WITH_KNOTS ( ( 3, 2, 2, 2, 3 ),
 ( 0.4705882352941176405, 0.4779411764705882582, 0.4852941176470588203, 0.4926470588235294379, 0.5000000000000000000 ),
 .UNSPECIFIED. ) 
 CURVE ( )  GEOMETRIC_REPRESENTATION_ITEM ( )  RATIONAL_B_SPLINE_CURVE ( ( 1.000000000000000000, 0.9238795325112867385, 1.000000000000000000, 0.9238795325112867385, 1.000000000000000000, 0.9238795325112867385, 1.000000000000000000, 0.9238795325112867385, 1.000000000000000000 ) ) 
 REPRESENTATION_ITEM ( '' )  );
#17941 = ORIENTED_EDGE ( 'NONE', *, *, #23781, .T. ) ;
#17942 = CARTESIAN_POINT ( 'NONE',  ( 154.6875000000000284, 4.242640687119269671, 4.242640687119298093 ) ) ;
#17943 = CARTESIAN_POINT ( 'NONE',  ( 0.000000000000000000, 5.999999999999977796, -73.21132486540521711 ) ) ;
#17944 = LINE ( 'NONE', #3766, #10359 ) ;
#17945 = CARTESIAN_POINT ( 'NONE',  ( 116.5627832217621034, 0.7662911109078888172, 1.849990392679652151 ) ) ;
#17946 = EDGE_CURVE ( 'NONE', #16741, #25006, #15773, .T. ) ;
#17947 = ORIENTED_EDGE ( 'NONE', *, *, #17946, .F. ) ;
#17948 =( BOUNDED_CURVE ( )  B_SPLINE_CURVE ( 2, ( #9685, #155, #28839, #7369, #7798, #2744, #5492, #9985, #19361 ),
 .UNSPECIFIED., .F., .F. ) 
 B_SPLINE_CURVE_WITH_KNOTS ( ( 3, 2, 2, 2, 3 ),
 ( 0.09722222222222222376, 0.09814814814814815103, 0.1000000000000000056, 0.1018518518518518462, 0.1027777777777777735 ),
 .UNSPECIFIED. ) 
 CURVE ( )  GEOMETRIC_REPRESENTATION_ITEM ( )  RATIONAL_B_SPLINE_CURVE ( ( 0.9330127018922194093, 0.9330127018922194093, 1.000000000000000000, 0.8660254037844388186, 1.000000000000000000, 0.8660254037844388186, 1.000000000000000000, 0.9330127018922194093, 0.9330127018922194093 ) ) 
 REPRESENTATION_ITEM ( '' )  );
#17949 = VECTOR ( 'NONE', #28852, 1000.000000000000000 ) ;
#17950 = ORIENTED_EDGE ( 'NONE', *, *, #27676, .T. ) ;
#17951 = CARTESIAN_POINT ( 'NONE',  ( -6.350852961085760029, -1.281975124255709124E-13, -98.62500000000005684 ) ) ;
#17952 = CARTESIAN_POINT ( 'NONE',  ( -5.999999999999963585, 9.296355089585909904E-15, -169.4136751345948539 ) ) ;
#17953 = EDGE_CURVE ( 'NONE', #21789, #15083, #28919, .T. ) ;
#17954 = CARTESIAN_POINT ( 'NONE',  ( 3.608439182435180470, 6.249999999999982236, -117.5580127018922383 ) ) ;
#17955 = EDGE_CURVE ( 'NONE', #17415, #5531, #20967, .T. ) ;
#17956 = EDGE_LOOP ( 'NONE', ( #13703, #12181, #18582, #14689 ) ) ;
#17957 = DIRECTION ( 'NONE',  ( 0.000000000000000000, 0.000000000000000000, 1.000000000000000000 ) ) ;
#17958 = CARTESIAN_POINT ( 'NONE',  ( -5.999999999999956479, -1.607695154586745057, -143.8466878364870354 ) ) ;
#17959 = AXIS2_PLACEMENT_3D ( 'NONE', #5909, #29577, #3604 ) ;
#17960 = CARTESIAN_POINT ( 'NONE',  ( 7.216878364870455975, -6.409875621278545621E-14, -50.30801270189225249 ) ) ;
#17961 = ORIENTED_EDGE ( 'NONE', *, *, #24664, .T. ) ;
#17962 = CARTESIAN_POINT ( 'NONE',  ( 6.000000000000000888, 1.743066579297358182E-13, -61.58632486540521001 ) ) ;
#17963 = CARTESIAN_POINT ( 'NONE',  ( 6.350852961086080661, -9.614813431917819062E-14, -160.8750000000000284 ) ) ;
#17964 = CARTESIAN_POINT ( 'NONE',  ( 115.5624999999999005, -2.499999999999934719, -1.035533905932568777 ) ) ;
#17965 = CARTESIAN_POINT ( 'NONE',  ( 10.21132486540524198, -2.499999999999835687, -1.110223024625156540E-13 ) ) ;
#17966 = CARTESIAN_POINT ( 'NONE',  ( 6.350852961086080661, -9.614813431917819062E-14, -106.8750000000000426 ) ) ;
#17967 = CYLINDRICAL_SURFACE ( 'NONE', #27626, 2.000000000000012879 ) ;
#17968 = CARTESIAN_POINT ( 'NONE',  ( -3.175426480542816510, 5.499999999999865885, -103.3750000000000142 ) ) ;
#17969 = DIRECTION ( 'NONE',  ( -0.000000000000000000, 0.000000000000000000, -1.000000000000000000 ) ) ;
#17970 = DIRECTION ( 'NONE',  ( 0.000000000000000000, 0.000000000000000000, -1.000000000000000000 ) ) ;
#17971 = CARTESIAN_POINT ( 'NONE',  ( -5.999999999999866773, 1.607695154586893826, -144.9033121635130215 ) ) ;
#17972 = ORIENTED_EDGE ( 'NONE', *, *, #22431, .T. ) ;
#17973 = CARTESIAN_POINT ( 'NONE',  ( 16.37500000000016698, 1.110223024625156540E-13, -2.649519052838389399 ) ) ;
#17974 = CARTESIAN_POINT ( 'NONE',  ( 115.6874999999997584, -1.035533905932719101, -2.499999999999844569 ) ) ;
#17975 = CARTESIAN_POINT ( 'NONE',  ( 110.6252832217622029, 5.551115123125782702E-14, 1.849990392679523588 ) ) ;
#17976 = CARTESIAN_POINT ( 'NONE',  ( 108.2113248654050892, -1.999999999999946265, 0.000000000000000000 ) ) ;
#17977 = ORIENTED_EDGE ( 'NONE', *, *, #5976, .T. ) ;
#17978 = DIRECTION ( 'NONE',  ( 0.000000000000000000, 0.000000000000000000, -1.000000000000000000 ) ) ;
#17979 = CARTESIAN_POINT ( 'NONE',  ( -5.412658773652739619, 3.124999999999975131, -90.81698729810783277 ) ) ;
#17980 = EDGE_CURVE ( 'NONE', #2648, #8247, #26853, .T. ) ;
#17981 = CARTESIAN_POINT ( 'NONE',  ( -6.000000000000007105, -1.607695154586655129, -129.7693375672974128 ) ) ;
#17982 = ORIENTED_EDGE ( 'NONE', *, *, #28511, .F. ) ;
#17983 = CARTESIAN_POINT ( 'NONE',  ( 6.000000000000000000, 2.951592740943527306E-14, -157.5863248654052313 ) ) ;
#17984 = CARTESIAN_POINT ( 'NONE',  ( -3.175426480542816510, 5.499999999999865885, -151.3749999999999716 ) ) ;
#17985 = VERTEX_POINT ( 'NONE', #13162 ) ;
#17986 = ORIENTED_EDGE ( 'NONE', *, *, #8741, .F. ) ;
#17987 = CARTESIAN_POINT ( 'NONE',  ( 154.1250000000000284, 0.000000000000000000, -6.000000000000005329 ) ) ;
#17988 = CARTESIAN_POINT ( 'NONE',  ( -3.175426480542816510, 5.499999999999865885, -124.3749999999999858 ) ) ;
#17989 = EDGE_CURVE ( 'NONE', #16735, #91, #30013, .T. ) ;
#17990 = CARTESIAN_POINT ( 'NONE',  ( -5.412658773652739619, 3.124999999999975131, -141.1830127018922667 ) ) ;
#17991 = ORIENTED_EDGE ( 'NONE', *, *, #15316, .F. ) ;
#17992 = CARTESIAN_POINT ( 'NONE',  ( 6.000000000000000888, 1.743066579297358182E-13, -57.08632486540521001 ) ) ;
#17993 = CARTESIAN_POINT ( 'NONE',  ( 7.216878364870455975, -6.409875621278545621E-14, -127.4419872981078328 ) ) ;
#17994 = CARTESIAN_POINT ( 'NONE',  ( 3.608439182435180470, 6.249999999999982236, -175.1919872981077901 ) ) ;
#17995 = CARTESIAN_POINT ( 'NONE',  ( 4.763139720814407951, 2.750000000000002665, -174.2500000000000284 ) ) ;
#17996 = CARTESIAN_POINT ( 'NONE',  ( 6.000000000000000888, 7.762456499804235646E-14, -122.1636751345948397 ) ) ;
#17997 = LINE ( 'NONE', #8116, #1496 ) ;
#17998 =( BOUNDED_CURVE ( )  B_SPLINE_CURVE ( 2, ( #11604, #9724, #6947, #7098, #28279, #14214, #28574, #14505, #7405 ),
 .UNSPECIFIED., .F., .T. ) 
 B_SPLINE_CURVE_WITH_KNOTS ( ( 3, 2, 2, 2, 3 ),
 ( 0.2416666666666666963, 0.2425925925925925819, 0.2444444444444444642, 0.2462962962962963465, 0.2472222222222222321 ),
 .UNSPECIFIED. ) 
 CURVE ( )  GEOMETRIC_REPRESENTATION_ITEM ( )  RATIONAL_B_SPLINE_CURVE ( ( 0.9330127018922194093, 0.9330127018922234061, 1.000000000000000000, 0.8660254037844388186, 1.000000000000000000, 0.8660254037844388186, 1.000000000000000000, 0.9330127018922194093, 0.9330127018922194093 ) ) 
 REPRESENTATION_ITEM ( '' )  );
#17999 = VERTEX_POINT ( 'NONE', #966 ) ;
#18000 = CARTESIAN_POINT ( 'NONE',  ( 13.56250000000003375, -1.999999999999971800, -0.8284271247462354770 ) ) ;
#18001 = CYLINDRICAL_SURFACE ( 'NONE', #14260, 6.000000000000000888 ) ;
#18002 = AXIS2_PLACEMENT_3D ( 'NONE', #4515, #18825, #11312 ) ;
#18003 = CARTESIAN_POINT ( 'NONE',  ( 159.9311390374854227, -11.50936040660355353, -3.430377613042744578 ) ) ;
#18004 = CARTESIAN_POINT ( 'NONE',  ( 5.196152422706629359, 3.000000000000002665, -46.46132486540521711 ) ) ;
#18005 = CARTESIAN_POINT ( 'NONE',  ( 110.5002832217622881, 1.308140751793668288, 1.308140751793640533 ) ) ;
#18006 = CARTESIAN_POINT ( 'NONE',  ( 3.608439182435180470, 6.249999999999982236, -70.19198729810780435 ) ) ;
#18007 = VECTOR ( 'NONE', #16439, 1000.000000000000000 ) ;
#18008 = CARTESIAN_POINT ( 'NONE',  ( -3.608439182435052128, -6.250000000000110134, -54.44198729810779724 ) ) ;
#18009 = CARTESIAN_POINT ( 'NONE',  ( -4.999999999999879208, -9.000000000000007105, -5.000000000000004441 ) ) ;
#18010 = CARTESIAN_POINT ( 'NONE',  ( -4.763139720814407951, -2.750000000000016431, -50.49999999999998579 ) ) ;
#18011 = CARTESIAN_POINT ( 'NONE',  ( 148.1324251345948255, -5.500000000000012434, -2.278174593052012309 ) ) ;
#18012 = DIRECTION ( 'NONE',  ( -7.147005652999508048E-36, 5.642372883946980038E-36, 1.000000000000000000 ) ) ;
#18013 = CARTESIAN_POINT ( 'NONE',  ( 6.350852961086080661, -9.614813431917819062E-14, -130.8750000000000284 ) ) ;
#18014 = CARTESIAN_POINT ( 'NONE',  ( 0.000000000000000000, 0.000000000000000000, 0.000000000000000000 ) ) ;
#18015 = CARTESIAN_POINT ( 'NONE',  ( 104.7401757384973138, -1.135388960144151582, -1.480659523195497096 ) ) ;
#18016 = STYLED_ITEM ( 'NONE', ( #16208 ), #24129 ) ;
#18017 = VERTEX_POINT ( 'NONE', #10367 ) ;
#18018 = FACE_OUTER_BOUND ( 'NONE', #10610, .T. ) ;
#18019 = FACE_OUTER_BOUND ( 'NONE', #15926, .T. ) ;
#18020 = CARTESIAN_POINT ( 'NONE',  ( 141.0148502691896510, -3.535533905932725318, -3.535533905932725318 ) ) ;
#18021 = ORIENTED_EDGE ( 'NONE', *, *, #15780, .F. ) ;
#18022 = CARTESIAN_POINT ( 'NONE',  ( 113.3122167782374277, -0.7662911109077388261, -1.849990392679231599 ) ) ;
#18023 = CARTESIAN_POINT ( 'NONE',  ( 10.78867513459497118, -2.499999999999946709, -5.551115123125782702E-14 ) ) ;
#18024 = CARTESIAN_POINT ( 'NONE',  ( 9.625000000000133227, -1.414213562372979016, -1.414213562373145550 ) ) ;
#18025 = CARTESIAN_POINT ( 'NONE',  ( 7.216878364870455975, -6.409875621278545621E-14, -112.4419872981078186 ) ) ;
#18026 = EDGE_CURVE ( 'NONE', #19914, #12110, #21474, .T. ) ;
#18027 = CARTESIAN_POINT ( 'NONE',  ( 140.0000000000000284, -10.99818166789400919, -4.800000000000004263 ) ) ;
#18028 = EDGE_CURVE ( 'NONE', #15617, #29147, #20650, .T. ) ;
#18029 = CARTESIAN_POINT ( 'NONE',  ( 0.000000000000000000, 0.000000000000000000, 0.000000000000000000 ) ) ;
#18030 = ORIENTED_EDGE ( 'NONE', *, *, #24347, .F. ) ;
#18031 = CARTESIAN_POINT ( 'NONE',  ( 21.83632486540532014, 1.767766952966487448, 1.767766952966376426 ) ) ;
#18032 = CARTESIAN_POINT ( 'NONE',  ( 139.6875000000000284, 4.242640687119269671, 4.242640687119298093 ) ) ;
#18033 = VERTEX_POINT ( 'NONE', #18512 ) ;
#18034 =( NAMED_UNIT ( * ) PLANE_ANGLE_UNIT ( ) SI_UNIT ( $, .RADIAN. ) );
#18035 = CARTESIAN_POINT ( 'NONE',  ( -4.763139720814407951, -2.750000000000016431, -49.00000000000004263 ) ) ;
#18036 = CARTESIAN_POINT ( 'NONE',  ( 21.75000000000007461, 2.220446049250313081E-13, -2.000000000000001776 ) ) ;
#18037 = AXIS2_PLACEMENT_3D ( 'NONE', #18614, #23219, #4303 ) ;
#18038 = CARTESIAN_POINT ( 'NONE',  ( -3.608439182435052128, -6.250000000000110134, -67.30801270189226670 ) ) ;
#18039 =( BOUNDED_CURVE ( )  B_SPLINE_CURVE ( 2, ( #20792, #1139, #15323, #19894, #13436, #22783, #11122, #20470, #16808 ),
 .UNSPECIFIED., .F., .T. ) 
 B_SPLINE_CURVE_WITH_KNOTS ( ( 3, 2, 2, 2, 3 ),
 ( 0.1624999999999987566, 0.1687499999999989564, 0.1749999999999992673, 0.1812499999999994948, 0.1874999999999996947 ),
 .UNSPECIFIED. ) 
 CURVE ( )  GEOMETRIC_REPRESENTATION_ITEM ( )  RATIONAL_B_SPLINE_CURVE ( ( 1.000000000000014877, 0.9238795325112718615, 1.000000000000000000, 0.9238795325112867385, 1.000000000000000000, 0.9238795325112867385, 1.000000000000000000, 0.9238795325112904022, 0.9999999999999963363 ) ) 
 REPRESENTATION_ITEM ( '' )  );
#18040 = CARTESIAN_POINT ( 'NONE',  ( 149.7976497308104058, 0.000000000000000000, 5.000000000000004441 ) ) ;
#18041 = CARTESIAN_POINT ( 'NONE',  ( 3.464101615137757051, -5.999999999999979572, -177.9136751345948255 ) ) ;
#18042 = CYLINDRICAL_SURFACE ( 'NONE', #24343, 0.5000000000000004441 ) ;
#18043 = CARTESIAN_POINT ( 'NONE',  ( -5.999999999999956479, -1.607695154586745057, -67.34668783648702117 ) ) ;
#18044 = CARTESIAN_POINT ( 'NONE',  ( 106.2886751345948255, 2.000000000000029310, 1.110223024625156540E-13 ) ) ;
#18045 = CARTESIAN_POINT ( 'NONE',  ( 3.175426480543072749, -5.500000000000105693, -135.6250000000000284 ) ) ;
#18046 = AXIS2_PLACEMENT_3D ( 'NONE', #4649, #18663, #4502 ) ;
#18047 = CARTESIAN_POINT ( 'NONE',  ( 7.216878364870455975, -6.409875621278545621E-14, -147.8080127018922667 ) ) ;
#18048 = CARTESIAN_POINT ( 'NONE',  ( 0.000000000000000000, 0.000000000000000000, 0.000000000000000000 ) ) ;
#18049 = ORIENTED_EDGE ( 'NONE', *, *, #4729, .T. ) ;
#18050 = CARTESIAN_POINT ( 'NONE',  ( -6.350852961085760029, -1.281975124255709124E-13, -62.62500000000001421 ) ) ;
#18051 = FILL_AREA_STYLE ('',( #8649 ) ) ;
#18052 = DIRECTION ( 'NONE',  ( 1.000000000000000000, 1.734723475976843579E-16, -0.000000000000000000 ) ) ;
#18053 = ORIENTED_EDGE ( 'NONE', *, *, #10409, .F. ) ;
#18054 = AXIS2_PLACEMENT_3D ( 'NONE', #28932, #17312, #695 ) ;
#18055 = CARTESIAN_POINT ( 'NONE',  ( 110.8124999999999432, 1.035533905932719101, -2.499999999999904521 ) ) ;
#18056 = CARTESIAN_POINT ( 'NONE',  ( 146.8125000000000284, 4.242640687119298093, -4.242640687119298093 ) ) ;
#18057 = DIRECTION ( 'NONE',  ( 5.551115123125785167E-17, -1.000000000000000000, -8.881784197001256268E-16 ) ) ;
#18058 = CARTESIAN_POINT ( 'NONE',  ( 116.0000000000000142, 0.000000000000000000, 0.000000000000000000 ) ) ;
#18059 = ADVANCED_FACE ( 'NONE', ( #16077 ), #9269, .T. ) ;
#18060 = ORIENTED_EDGE ( 'NONE', *, *, #27593, .F. ) ;
#18061 = CARTESIAN_POINT ( 'NONE',  ( 140.6250000000000284, 0.000000000000000000, -6.000000000000005329 ) ) ;
#18062 = CARTESIAN_POINT ( 'NONE',  ( -5.999999999999963585, 1.780251999655701777E-13, -103.4136751345948255 ) ) ;
#18063 = VERTEX_POINT ( 'NONE', #23267 ) ;
#18064 = CARTESIAN_POINT ( 'NONE',  ( 4.763139720814407951, 2.750000000000002665, -147.2500000000000000 ) ) ;
#18065 = ORIENTED_EDGE ( 'NONE', *, *, #27920, .T. ) ;
#18066 = CARTESIAN_POINT ( 'NONE',  ( 12.87500000000008171, 1.414213562373312083, -1.414213562373034527 ) ) ;
#18067 = VERTEX_POINT ( 'NONE', #18206 ) ;
#18068 = CARTESIAN_POINT ( 'NONE',  ( 3.175426480543072749, -5.500000000000105693, -71.12500000000004263 ) ) ;
#18069 = ORIENTED_EDGE ( 'NONE', *, *, #11907, .F. ) ;
#18070 = CARTESIAN_POINT ( 'NONE',  ( -3.977757852569110852, -10.25981801084819445, -29.50831862515141424 ) ) ;
#18071 = CARTESIAN_POINT ( 'NONE',  ( 135.5000000000000284, -54.99999999999993605, -7.500000000000007105 ) ) ;
#18072 = CARTESIAN_POINT ( 'NONE',  ( -5.999999999999919176, 1.607695154586804565, -98.40331216351297883 ) ) ;
#18073 = CARTESIAN_POINT ( 'NONE',  ( 6.000000000000052403, -1.607695154586662678, -64.65331216351297883 ) ) ;
#18074 = CIRCLE ( 'NONE', #25890, 16.50000000000000355 ) ;
#18075 = APPLICATION_PROTOCOL_DEFINITION ( 'draft international standard', 'automotive_design', 1998, #24772 ) ;
#18076 = CARTESIAN_POINT ( 'NONE',  ( 6.350852961086080661, -9.614813431917819062E-14, -159.3750000000000284 ) ) ;
#18077 = DIRECTION ( 'NONE',  ( -7.147005652999508048E-36, 5.642372883946980038E-36, 1.000000000000000000 ) ) ;
#18078 = CARTESIAN_POINT ( 'NONE',  ( -3.464101615137725076, 5.999999999999979572, -49.08632486540521711 ) ) ;
#18079 = EDGE_CURVE ( 'NONE', #3562, #4040, #22217, .T. ) ;
#18080 = CARTESIAN_POINT ( 'NONE',  ( -3.175426480542816066, -5.500000000000057732, -89.37500000000001421 ) ) ;
#18081 = DIRECTION ( 'NONE',  ( 0.000000000000000000, 0.000000000000000000, 1.000000000000000000 ) ) ;
#18082 = CARTESIAN_POINT ( 'NONE',  ( -3.175426480542816510, -5.500000000000057732, -77.37500000000001421 ) ) ;
#18083 = CARTESIAN_POINT ( 'NONE',  ( 150.0148502691896510, -3.535533905932725318, -3.535533905932725318 ) ) ;
#18084 = CARTESIAN_POINT ( 'NONE',  ( 3.464101615137852974, 5.999999999999884537, -142.3363248654052029 ) ) ;
#18085 = CARTESIAN_POINT ( 'NONE',  ( 159.0000000000000284, -12.00000000000001066, 4.000000000000003553 ) ) ;
#18086 = CIRCLE ( 'NONE', #16149, 0.9999999999999993339 ) ;
#18087 = CARTESIAN_POINT ( 'NONE',  ( 0.000000000000000000, 5.999999999999977796, -103.7886751345948255 ) ) ;
#18088 = CARTESIAN_POINT ( 'NONE',  ( 116.0000000000000142, 0.000000000000000000, 0.000000000000000000 ) ) ;
#18089 = CARTESIAN_POINT ( 'NONE',  ( 0.000000000000000000, 0.000000000000000000, 0.000000000000000000 ) ) ;
#18090 = EDGE_CURVE ( 'NONE', #16041, #5962, #27484, .T. ) ;
#18091 = ORIENTED_EDGE ( 'NONE', *, *, #22997, .T. ) ;
#18092 = CARTESIAN_POINT ( 'NONE',  ( 156.0937500000000000, 6.000000000000005329, 2.485281374238585972 ) ) ;
#18093 = DIRECTION ( 'NONE',  ( 1.000000000000000000, 0.000000000000000000, 0.000000000000000000 ) ) ;
#18094 = CARTESIAN_POINT ( 'NONE',  ( 116.8127832217622597, -1.849990392679441875, 0.7662911109078888172 ) ) ;
#18095 = CARTESIAN_POINT ( 'NONE',  ( -6.000000000000000888, 1.067854986875958443E-15, 7.560779664488942560E-35 ) ) ;
#18096 = ORIENTED_EDGE ( 'NONE', *, *, #29029, .F. ) ;
#18097 = CARTESIAN_POINT ( 'NONE',  ( 4.763139720814407951, 2.750000000000002665, -96.25000000000000000 ) ) ;
#18098 = LINE ( 'NONE', #5922, #3280 ) ;
#18099 = CARTESIAN_POINT ( 'NONE',  ( -3.608439182435115633, 6.249999999999965361, -112.8080127018922241 ) ) ;
#18100 = ORIENTED_EDGE ( 'NONE', *, *, #14087, .T. ) ;
#18101 = CARTESIAN_POINT ( 'NONE',  ( -19.49999999999998224, -54.99999999999990763, -7.500000000000007105 ) ) ;
#18102 = DIRECTION ( 'NONE',  ( -1.000000000000000000, -1.067522139062651904E-16, 0.000000000000000000 ) ) ;
#18103 = CARTESIAN_POINT ( 'NONE',  ( 3.608439182435180470, 6.249999999999982236, -53.05801270189219565 ) ) ;
#18104 = EDGE_LOOP ( 'NONE', ( #9004, #17529, #24410, #29985 ) ) ;
#18105 =( NAMED_UNIT ( * ) PLANE_ANGLE_UNIT ( ) SI_UNIT ( $, .RADIAN. ) );
#18106 = CARTESIAN_POINT ( 'NONE',  ( 6.000000000000052403, 1.607695154586625819, -136.5193375672973559 ) ) ;
#18107 = CARTESIAN_POINT ( 'NONE',  ( -3.175426480542816510, 5.499999999999865885, -163.3750000000000568 ) ) ;
#18108 = CARTESIAN_POINT ( 'NONE',  ( 118.1249999999999147, 1.767766952966320915, 1.767766952966431937 ) ) ;
#18109 = ADVANCED_FACE ( 'NONE', ( #13924 ), #8661, .F. ) ;
#18110 = CARTESIAN_POINT ( 'NONE',  ( -2.775557561562891351E-14, -5.500000000000115463, -107.2500000000000142 ) ) ;
#18111 = CARTESIAN_POINT ( 'NONE',  ( 105.8988248654050750, 0.8284271247463257382, 2.000000000000271783 ) ) ;
#18112 = CARTESIAN_POINT ( 'NONE',  ( 6.000000000000000888, 7.762456499804235646E-14, -123.6636751345948255 ) ) ;
#18113 =( BOUNDED_CURVE ( )  B_SPLINE_CURVE ( 2, ( #15166, #1621, #20063, #19754, #6371, #22530, #26951, #29099, #10872 ),
 .UNSPECIFIED., .F., .T. ) 
 B_SPLINE_CURVE_WITH_KNOTS ( ( 3, 2, 2, 2, 3 ),
 ( 0.7861111111111112049, 0.7870370370370370905, 0.7888888888888888618, 0.7907407407407407440, 0.7916666666666666297 ),
 .UNSPECIFIED. ) 
 CURVE ( )  GEOMETRIC_REPRESENTATION_ITEM ( )  RATIONAL_B_SPLINE_CURVE ( ( 0.9330127018922194093, 0.9330127018922234061, 1.000000000000000000, 0.8660254037844388186, 1.000000000000000000, 0.8660254037844388186, 1.000000000000000000, 0.9330127018922234061, 0.9330127018922194093 ) ) 
 REPRESENTATION_ITEM ( '' )  );
#18114 = CARTESIAN_POINT ( 'NONE',  ( -4.763139720814407951, 2.749999999999946709, -95.75000000000000000 ) ) ;
#18115 = CARTESIAN_POINT ( 'NONE',  ( 5.999999999999999112, 2.951592740943527306E-14, -162.6636751345948824 ) ) ;
#18116 = ORIENTED_EDGE ( 'NONE', *, *, #18509, .T. ) ;
#18117 = CARTESIAN_POINT ( 'NONE',  ( 13.12500000000010836, -2.649519052838000821, -5.551115123125782702E-14 ) ) ;
#18118 = CARTESIAN_POINT ( 'NONE',  ( 117.8749999999998010, 1.767766952966320915, -1.767766952966209892 ) ) ;
#18119 = CARTESIAN_POINT ( 'NONE',  ( 110.8752832217622029, -1.849990392679495832, 0.000000000000000000 ) ) ;
#18120 = EDGE_CURVE ( 'NONE', #25268, #16010, #21939, .T. ) ;
#18121 = DIRECTION ( 'NONE',  ( -7.147005652999508048E-36, 5.642372883946980038E-36, 1.000000000000000000 ) ) ;
#18122 =( BOUNDED_SURFACE ( )  B_SPLINE_SURFACE ( 3, 2, ( 
 ( #8783, #20306, #27483 ),
 ( #1704, #29503, #19990 ),
 ( #17874, #29651, #8618 ),
 ( #11258, #18027, #13121 ) ),
 .UNSPECIFIED., .F., .F., .T. ) 
 B_SPLINE_SURFACE_WITH_KNOTS ( ( 4, 4 ),
 ( 3, 3 ),
 ( -1.355252715606880543E-18, 0.0002125775066526909465 ),
 ( 0.000000000000000000, 1.000000000000000000 ),
 .UNSPECIFIED. ) 
 GEOMETRIC_REPRESENTATION_ITEM ( )  RATIONAL_B_SPLINE_SURFACE ( (
 ( 1.000000000000000000, 0.7576044462920076272, 1.000000000000000000),
 ( 1.000000000000000000, 0.7424605758826383628, 1.000000000000000000),
 ( 1.000000000000000000, 0.7257758655053253571, 1.000000000000000000),
 ( 1.000000000000000000, 0.7071067811865475727, 1.000000000000000000) ) ) 
 REPRESENTATION_ITEM ( '' )  SURFACE ( )  );
#18123 = EDGE_LOOP ( 'NONE', ( #18919, #29928, #5025, #736 ) ) ;
#18124 = DIRECTION ( 'NONE',  ( -6.938893903907221278E-15, 1.000000000000000000, 0.000000000000000000 ) ) ;
#18125 = CARTESIAN_POINT ( 'NONE',  ( 2.775557561562891351E-14, 6.250000000000033751, -91.06698729810780435 ) ) ;
#18126 = CARTESIAN_POINT ( 'NONE',  ( 3.464101615137757051, -5.999999999999979572, -96.91367513459481131 ) ) ;
#18127 = VERTEX_POINT ( 'NONE', #25077 ) ;
#18128 = CARTESIAN_POINT ( 'NONE',  ( -4.758024543289570474, 9.918640242984139377, -28.66037974350895112 ) ) ;
#18129 = ORIENTED_EDGE ( 'NONE', *, *, #15845, .T. ) ;
#18130 = VERTEX_POINT ( 'NONE', #2060 ) ;
#18131 = CARTESIAN_POINT ( 'NONE',  ( 159.5625000000000284, -4.242640687119298093, 4.242640687119298093 ) ) ;
#18132 = CARTESIAN_POINT ( 'NONE',  ( -4.763139720814407951, 2.749999999999946709, -122.7500000000000284 ) ) ;
#18133 = CIRCLE ( 'NONE', #5349, 0.5000000000000004441 ) ;
#18134 = CARTESIAN_POINT ( 'NONE',  ( 5.412658773652739619, 3.124999999999988898, -140.1830127018922667 ) ) ;
#18135 = ORIENTED_EDGE ( 'NONE', *, *, #14546, .F. ) ;
#18136 = CARTESIAN_POINT ( 'NONE',  ( 6.000000000000000888, -3.330669073875464691E-16, -7.560779664488942560E-35 ) ) ;
#18137 = STYLED_ITEM ( 'NONE', ( #24131 ), #14454 ) ;
#18138 = CARTESIAN_POINT ( 'NONE',  ( -5.412658773652684552, -3.125000000000099920, -120.5669872981078328 ) ) ;
#18139 = CARTESIAN_POINT ( 'NONE',  ( 5.412658773652712085, -3.125000000000086153, -174.0669872981078186 ) ) ;
#18140 = CARTESIAN_POINT ( 'NONE',  ( -3.175426480542816510, -5.500000000000057732, -171.8750000000000284 ) ) ;
#18141 = CARTESIAN_POINT ( 'NONE',  ( 152.9136751345948539, 0.000000000000000000, -5.500000000000005329 ) ) ;
#18142 = DIRECTION ( 'NONE',  ( -7.147005652999508048E-36, 5.642372883946980038E-36, 1.000000000000000000 ) ) ;
#18143 = ORIENTED_EDGE ( 'NONE', *, *, #8844, .F. ) ;
#18144 = LINE ( 'NONE', #29782, #26448 ) ;
#18145 = CARTESIAN_POINT ( 'NONE',  ( 5.000000000000088818, 5.637083940101657433E-14, -6.000000000000056843 ) ) ;
#18146 = CARTESIAN_POINT ( 'NONE',  ( 5.196152422706629359, 3.000000000000002665, -171.5386751345948539 ) ) ;
#18147 = CARTESIAN_POINT ( 'NONE',  ( 157.8675748654052313, -5.500000000000012434, 2.278174593052012309 ) ) ;
#18148 = CARTESIAN_POINT ( 'NONE',  ( 110.9377832217620323, -1.849990392679411677, -0.7662911109076485650 ) ) ;
#18149 = CARTESIAN_POINT ( 'NONE',  ( -5.412658773652684552, -3.125000000000099920, -75.56698729810784698 ) ) ;
#18150 = CARTESIAN_POINT ( 'NONE',  ( -7.216878364870328078, 0.000000000000000000, -62.19198729810784698 ) ) ;
#18151 = CARTESIAN_POINT ( 'NONE',  ( -5.999999999999956479, -1.607695154586745057, -170.8466878364870638 ) ) ;
#18152 = CARTESIAN_POINT ( 'NONE',  ( -6.350852961085760029, -1.281975124255709124E-13, -50.62500000000001421 ) ) ;
#18153 = CARTESIAN_POINT ( 'NONE',  ( 148.4136751345948539, 0.000000000000000000, -5.500000000000005329 ) ) ;
#18154 = EDGE_CURVE ( 'NONE', #16860, #28335, #8971, .T. ) ;
#18155 = CARTESIAN_POINT ( 'NONE',  ( -14.99999999999999289, -54.99999999999990763, 7.500000000000007105 ) ) ;
#18156 = CARTESIAN_POINT ( 'NONE',  ( 3.175426480543072749, -5.500000000000105693, -120.6250000000000284 ) ) ;
#18157 = CARTESIAN_POINT ( 'NONE',  ( -5.999999999999963585, -1.487416814333745711E-14, -80.91367513459482552 ) ) ;
#18158 = ORIENTED_EDGE ( 'NONE', *, *, #1937, .F. ) ;
#18159 = CARTESIAN_POINT ( 'NONE',  ( -5.999999999999957367, 1.607695154586737507, -157.4806624327026157 ) ) ;
#18160 = VECTOR ( 'NONE', #28185, 1000.000000000000000 ) ;
#18161 = DIRECTION ( 'NONE',  ( 1.000000000000000000, -5.551115123125774690E-17, 0.000000000000000000 ) ) ;
#18162 = ADVANCED_FACE ( 'NONE', ( #25696 ), #4034, .F. ) ;
#18163 = CARTESIAN_POINT ( 'NONE',  ( 139.8898502691896510, 3.535533905932725318, -3.535533905932725318 ) ) ;
#18164 = DIRECTION ( 'NONE',  ( -7.147005652999508048E-36, 5.642372883946980038E-36, 1.000000000000000000 ) ) ;
#18165 = VECTOR ( 'NONE', #16254, 1000.000000000000000 ) ;
#18166 = EDGE_LOOP ( 'NONE', ( #16451, #27109, #9019, #22510 ) ) ;
#18167 = CARTESIAN_POINT ( 'NONE',  ( 108.3747167782376124, -1.665334536937734811E-13, -1.849990392679523588 ) ) ;
#18168 = CARTESIAN_POINT ( 'NONE',  ( 116.0000000000000142, 0.000000000000000000, 0.000000000000000000 ) ) ;
#18169 = DIRECTION ( 'NONE',  ( -7.147005652999508048E-36, 5.642372883946980038E-36, 1.000000000000000000 ) ) ;
#18170 = COLOUR_RGB ( '', 0.72549020, 0.75294118, 0.79215686) ;
#18171 = CARTESIAN_POINT ( 'NONE',  ( -3.608439182435115633, 6.249999999999965361, -117.9419872981078470 ) ) ;
#18172 = FACE_OUTER_BOUND ( 'NONE', #25373, .T. ) ;
#18173 = ORIENTED_EDGE ( 'NONE', *, *, #1753, .F. ) ;
#18174 = VERTEX_POINT ( 'NONE', #18062 ) ;
#18175 = CARTESIAN_POINT ( 'NONE',  ( 138.3824251345948255, 5.500000000000012434, 2.278174593052012309 ) ) ;
#18176 = CARTESIAN_POINT ( 'NONE',  ( 143.0625000000000284, -4.242640687119298093, 4.242640687119298093 ) ) ;
#18177 = ORIENTED_EDGE ( 'NONE', *, *, #716, .F. ) ;
#18178 = VERTEX_POINT ( 'NONE', #14080 ) ;
#18179 = CARTESIAN_POINT ( 'NONE',  ( 4.763139720814407951, 2.750000000000002665, -51.25000000000001421 ) ) ;
#18180 = VECTOR ( 'NONE', #5139, 1000.000000000000000 ) ;
#18181 = CARTESIAN_POINT ( 'NONE',  ( 24.00000000000013145, 2.000000000000057288, -1.665334536937734811E-13 ) ) ;
#18182 = CYLINDRICAL_SURFACE ( 'NONE', #474, 6.000000000000000888 ) ;
#18183 = CARTESIAN_POINT ( 'NONE',  ( -3.608439182435052128, -6.250000000000110134, -68.80801270189220986 ) ) ;
#18184 = CARTESIAN_POINT ( 'NONE',  ( 149.5163997308103774, 4.999999999999989342, 2.071067811865468400 ) ) ;
#18185 = CARTESIAN_POINT ( 'NONE',  ( 0.000000000000000000, 5.499999999999991118, -180.0000000000000568 ) ) ;
#18186 = FACE_OUTER_BOUND ( 'NONE', #24546, .T. ) ;
#18187 = CARTESIAN_POINT ( 'NONE',  ( -5.999999999999962697, 3.323446944526963891E-14, -155.9136751345948255 ) ) ;
#18188 = CARTESIAN_POINT ( 'NONE',  ( 12.16367513459487526, 1.767766952966487448, -1.767766952966320915 ) ) ;
#18189 = FILL_AREA_STYLE_COLOUR ( '', #15051 ) ;
#18190 = ADVANCED_FACE ( 'NONE', ( #23416 ), #17575, .T. ) ;
#18191 = CARTESIAN_POINT ( 'NONE',  ( 116.0000000000000142, 0.000000000000000000, -5.500000000000000000 ) ) ;
#18192 = EDGE_CURVE ( 'NONE', #27528, #29800, #29461, .T. ) ;
#18193 = CARTESIAN_POINT ( 'NONE',  ( -2.775557561562891351E-14, -5.500000000000115463, -122.2500000000000284 ) ) ;
#18194 = LINE ( 'NONE', #29363, #16048 ) ;
#18195 = ORIENTED_EDGE ( 'NONE', *, *, #13697, .F. ) ;
#18196 = CARTESIAN_POINT ( 'NONE',  ( -4.763139720814407951, 2.749999999999946709, -65.75000000000002842 ) ) ;
#18197 = CARTESIAN_POINT ( 'NONE',  ( 0.000000000000000000, -5.999999999999991118, -154.0386751345948539 ) ) ;
#18198 = SURFACE_SIDE_STYLE ('',( #25067 ) ) ;
#18199 = CARTESIAN_POINT ( 'NONE',  ( 6.000000000000052403, 1.607695154586625819, -171.0193375672974128 ) ) ;
#18200 = EDGE_LOOP ( 'NONE', ( #15280, #14761, #7142, #2312 ) ) ;
#18201 = CARTESIAN_POINT ( 'NONE',  ( 105.5624999999997726, -2.499999999999874767, -1.035533905932568777 ) ) ;
#18202 = CARTESIAN_POINT ( 'NONE',  ( 147.2812500000000284, 2.485281374238585972, 6.000000000000005329 ) ) ;
#18203 = CARTESIAN_POINT ( 'NONE',  ( 13.25000000000017764, 5.551115123125782702E-14, 1.999999999999890754 ) ) ;
#18204 = PRESENTATION_STYLE_ASSIGNMENT (( #24780 ) ) ;
#18205 = CARTESIAN_POINT ( 'NONE',  ( 138.2812500000000284, 2.485281374238585972, 6.000000000000005329 ) ) ;
#18206 = CARTESIAN_POINT ( 'NONE',  ( 6.000000000000000888, 1.743066579297358182E-13, -92.16367513459482552 ) ) ;
#18207 = ORIENTED_EDGE ( 'NONE', *, *, #4726, .T. ) ;
#18208 = CARTESIAN_POINT ( 'NONE',  ( 4.763139720814407951, 2.750000000000002665, -138.2499999999999716 ) ) ;
#18209 =( BOUNDED_CURVE ( )  B_SPLINE_CURVE ( 2, ( #100, #28041, #7164, #16128, #16579, #18412, #1952, #30359, #25604 ),
 .UNSPECIFIED., .F., .T. ) 
 B_SPLINE_CURVE_WITH_KNOTS ( ( 3, 2, 2, 2, 3 ),
 ( 0.8281250000000000000, 0.8359375000000000000, 0.8437500000000000000, 0.8515625000000000000, 0.8593750000000000000 ),
 .UNSPECIFIED. ) 
 CURVE ( )  GEOMETRIC_REPRESENTATION_ITEM ( )  RATIONAL_B_SPLINE_CURVE ( ( 1.000000000000000000, 0.9238795325112867385, 1.000000000000000000, 0.9238795325112867385, 1.000000000000000000, 0.9238795325112867385, 1.000000000000000000, 0.9238795325112867385, 1.000000000000000000 ) ) 
 REPRESENTATION_ITEM ( '' )  );
#18210 = ORIENTED_EDGE ( 'NONE', *, *, #27531, .T. ) ;
#18211 = CARTESIAN_POINT ( 'NONE',  ( 12.56250000000007638, -1.999999999999851674, -0.8284271247462354770 ) ) ;
#18212 = VERTEX_POINT ( 'NONE', #14638 ) ;
#18213 = CARTESIAN_POINT ( 'NONE',  ( 0.000000000000000000, 5.499999999999991118, -75.00000000000001421 ) ) ;
#18214 = CARTESIAN_POINT ( 'NONE',  ( 18.58632486540534501, 1.767766952966431937, -1.767766952966431937 ) ) ;
#18215 = CARTESIAN_POINT ( 'NONE',  ( 10.37500000000005151, -1.414213562373034527, 1.414213562372756972 ) ) ;
#18216 = CARTESIAN_POINT ( 'NONE',  ( 105.0199988333806544, -0.2475512722506234553, -1.999999999999938938 ) ) ;
#18217 = CARTESIAN_POINT ( 'NONE',  ( -5.999999999999963585, 1.780251999655701777E-13, -83.91367513459482552 ) ) ;
#18218 = CARTESIAN_POINT ( 'NONE',  ( 135.0000000000000284, -54.99999999999993605, 7.500000000000007105 ) ) ;
#18219 =( GEOMETRIC_REPRESENTATION_CONTEXT ( 3 ) GLOBAL_UNCERTAINTY_ASSIGNED_CONTEXT ( ( #14321 ) ) GLOBAL_UNIT_ASSIGNED_CONTEXT ( ( #24252, #21968, #3658 ) ) REPRESENTATION_CONTEXT ( 'NONE', 'WORKASPACE' ) );
#18220 = CARTESIAN_POINT ( 'NONE',  ( 161.0000000000000284, 0.000000000000000000, -5.500000000000000000 ) ) ;
#18221 = CARTESIAN_POINT ( 'NONE',  ( 200.7502279533893272, 150.2326934200727919, 181.9927197319569530 ) ) ;
#18222 = EDGE_CURVE ( 'NONE', #17636, #7780, #9667, .T. ) ;
#18223 = CARTESIAN_POINT ( 'NONE',  ( -2.775557561562891351E-14, -5.500000000000115463, -144.7500000000000568 ) ) ;
#18224 = DIRECTION ( 'NONE',  ( -8.326672684688675286E-17, -2.081668171172168821E-17, 1.000000000000000000 ) ) ;
#18225 = CARTESIAN_POINT ( 'NONE',  ( -0.04562205425674009662, -14.50000000000001243, -8.291335958003937634 ) ) ;
#18226 = CARTESIAN_POINT ( 'NONE',  ( 0.000000000000000000, 5.499999999999991118, -87.00000000000002842 ) ) ;
#18227 = CARTESIAN_POINT ( 'NONE',  ( 0.000000000000000000, 0.000000000000000000, 0.000000000000000000 ) ) ;
#18228 = CARTESIAN_POINT ( 'NONE',  ( -3.175426480542816510, -5.500000000000057732, -69.87500000000005684 ) ) ;
#18229 = DIRECTION ( 'NONE',  ( -7.147005652999508048E-36, 5.642372883946980038E-36, 1.000000000000000000 ) ) ;
#18230 = CARTESIAN_POINT ( 'NONE',  ( 118.7886751345946692, -1.999999999999918510, 2.220446049250313081E-13 ) ) ;
#18231 = CARTESIAN_POINT ( 'NONE',  ( -5.999999999999962697, 3.323446944526963891E-14, -149.3363248654052313 ) ) ;
#18232 = CARTESIAN_POINT ( 'NONE',  ( 147.8363248654052029, 0.000000000000000000, -5.500000000000005329 ) ) ;
#18233 = CARTESIAN_POINT ( 'NONE',  ( 21.00000000000007461, 2.000000000000057288, 0.000000000000000000 ) ) ;
#18234 = CARTESIAN_POINT ( 'NONE',  ( 5.999999999999949374, 1.607695154586804565, -55.51933756729742697 ) ) ;
#18235 = CARTESIAN_POINT ( 'NONE',  ( -4.999999999999886313, -10.00000000000000888, -7.500000000000007105 ) ) ;
#18236 = CARTESIAN_POINT ( 'NONE',  ( -5.999999999999963585, 1.607695154586726627, -169.4806624327026157 ) ) ;
#18237 = EDGE_LOOP ( 'NONE', ( #5576, #21631, #27028, #28723 ) ) ;
#18238 = CARTESIAN_POINT ( 'NONE',  ( 154.3125000000000284, 4.242640687119298093, -4.242640687119298093 ) ) ;
#18239 = FILL_AREA_STYLE ('',( #28021 ) ) ;
#18240 = CARTESIAN_POINT ( 'NONE',  ( 118.0002832217622171, -1.308140751793612777, -1.308140751793418488 ) ) ;
#18241 = CARTESIAN_POINT ( 'NONE',  ( 5.999999999999999112, 2.951592740943527306E-14, -157.5863248654052313 ) ) ;
#18242 = ORIENTED_EDGE ( 'NONE', *, *, #2958, .T. ) ;
#18243 = ORIENTED_EDGE ( 'NONE', *, *, #25965, .T. ) ;
#18244 = VECTOR ( 'NONE', #27144, 1000.000000000000000 ) ;
#18245 = EDGE_LOOP ( 'NONE', ( #27715, #17039, #17003, #11841 ) ) ;
#18246 = EDGE_CURVE ( 'NONE', #18033, #8327, #12792, .T. ) ;
#18247 = CARTESIAN_POINT ( 'NONE',  ( 6.350852961086080661, -9.614813431917819062E-14, -100.8750000000000000 ) ) ;
#18248 = DIRECTION ( 'NONE',  ( -7.147005652999508048E-36, 5.642372883946980038E-36, 1.000000000000000000 ) ) ;
#18249 = CARTESIAN_POINT ( 'NONE',  ( 2.775557561562891351E-14, 6.250000000000033751, -106.9330127018922667 ) ) ;
#18250 = VERTEX_POINT ( 'NONE', #8604 ) ;
#18251 = CARTESIAN_POINT ( 'NONE',  ( 140.3905920374922403, -9.244723267345564821, -7.652122629818983057 ) ) ;
#18252 = AXIS2_PLACEMENT_3D ( 'NONE', #11094, #29947, #6762 ) ;
#18253 = DIRECTION ( 'NONE',  ( -0.000000000000000000, -1.000000000000000000, -0.000000000000000000 ) ) ;
#18254 = CARTESIAN_POINT ( 'NONE',  ( -6.350852961085760029, -1.281975124255709124E-13, -164.6249999999999716 ) ) ;
#18255 =( BOUNDED_CURVE ( )  B_SPLINE_CURVE ( 2, ( #9482, #6708, #2693, #4554, #9626, #2549, #21456, #4697, #243 ),
 .UNSPECIFIED., .F., .F. ) 
 B_SPLINE_CURVE_WITH_KNOTS ( ( 3, 2, 2, 2, 3 ),
 ( 0.1583333333333333259, 0.1592592592592592116, 0.1611111111111110938, 0.1629629629629629761, 0.1638888888888889728 ),
 .UNSPECIFIED. ) 
 CURVE ( )  GEOMETRIC_REPRESENTATION_ITEM ( )  RATIONAL_B_SPLINE_CURVE ( ( 0.9330127018922194093, 0.9330127018922194093, 1.000000000000000000, 0.8660254037844388186, 1.000000000000000000, 0.8660254037844388186, 1.000000000000000000, 0.9330127018922154125, 0.9330127018922194093 ) ) 
 REPRESENTATION_ITEM ( '' )  );
#18256 = CARTESIAN_POINT ( 'NONE',  ( -0.5000000000000004441, -15.00000000000001421, -7.500000000000007105 ) ) ;
#18257 = EDGE_LOOP ( 'NONE', ( #7958, #294, #2796, #27885 ) ) ;
#18258 = CARTESIAN_POINT ( 'NONE',  ( 6.000000000000000888, -1.859271017917181981E-14, -145.5863248654052029 ) ) ;
#18259 = DIRECTION ( 'NONE',  ( 1.000000000000000000, 0.000000000000000000, 0.000000000000000000 ) ) ;
#18260 = EDGE_CURVE ( 'NONE', #16823, #23494, #10788, .T. ) ;
#18261 = CARTESIAN_POINT ( 'NONE',  ( 147.7425748654052313, -2.278174593052259667, -5.499999999999763745 ) ) ;
#18262 = AXIS2_PLACEMENT_3D ( 'NONE', #25762, #21471, #4708 ) ;
#18263 = CARTESIAN_POINT ( 'NONE',  ( 6.350852961086080661, -9.614813431917819062E-14, -165.3750000000000284 ) ) ;
#18264 = CARTESIAN_POINT ( 'NONE',  ( 114.5624999999997442, -2.499999999999934719, -1.035533905932448873 ) ) ;
#18265 = CARTESIAN_POINT ( 'NONE',  ( -2.775557561562891351E-14, -5.500000000000115463, -111.7500000000000142 ) ) ;
#18266 = CARTESIAN_POINT ( 'NONE',  ( 160.3199251345948539, -2.278174593051888408, -5.500000000000135891 ) ) ;
#18267 = DIRECTION ( 'NONE',  ( -7.147005652999508048E-36, 5.642372883946980038E-36, 1.000000000000000000 ) ) ;
#18268 = CARTESIAN_POINT ( 'NONE',  ( 0.000000000000000000, 5.499999999999991118, -96.00000000000002842 ) ) ;
#18269 = CARTESIAN_POINT ( 'NONE',  ( 162.1086002691896795, -2.071067811865468400, -4.999999999999989342 ) ) ;
#18270 = CARTESIAN_POINT ( 'NONE',  ( -5.999999999999962697, 3.323446944526963891E-14, -150.8363248654052029 ) ) ;
#18271 = CARTESIAN_POINT ( 'NONE',  ( 0.7522378546890716722, -15.54348611246722633, 8.040548560309273896 ) ) ;
#18272 = ORIENTED_EDGE ( 'NONE', *, *, #11513, .F. ) ;
#18273 = CARTESIAN_POINT ( 'NONE',  ( 115.3124999999998863, -1.035533905932659149, 2.500000000000205169 ) ) ;
#18274 = CARTESIAN_POINT ( 'NONE',  ( 12.58632486540531303, 1.767766952966487448, -1.767766952966487448 ) ) ;
#18275 = CARTESIAN_POINT ( 'NONE',  ( 110.0627832217622313, -0.7662911109076785410, -1.849990392679171425 ) ) ;
#18276 = CARTESIAN_POINT ( 'NONE',  ( 161.0349825973430313, 2.426008766636172265, 4.985030962988786563 ) ) ;
#18277 = ORIENTED_EDGE ( 'NONE', *, *, #26186, .T. ) ;
#18278 = CARTESIAN_POINT ( 'NONE',  ( -5.999999999999904965, -1.607695154586834541, -170.2693375672974128 ) ) ;
#18279 = CARTESIAN_POINT ( 'NONE',  ( 109.1872167782375413, -1.849990392679441875, -0.7662911109077087390 ) ) ;
#18280 = VECTOR ( 'NONE', #25952, 1000.000000000000000 ) ;
#18281 = CARTESIAN_POINT ( 'NONE',  ( -3.608439182435115633, 6.249999999999965361, -87.94198729810783277 ) ) ;
#18282 = CARTESIAN_POINT ( 'NONE',  ( 111.0863248654051318, -1.414213562373034527, 1.414213562373145550 ) ) ;
#18283 = ORIENTED_EDGE ( 'NONE', *, *, #12685, .T. ) ;
#18284 = CARTESIAN_POINT ( 'NONE',  ( 2.775557561562891351E-14, 10.99999999999998224, -31.00000000000002842 ) ) ;
#18285 = ORIENTED_EDGE ( 'NONE', *, *, #17740, .F. ) ;
#18286 = ORIENTED_EDGE ( 'NONE', *, *, #12812, .F. ) ;
#18287 = CARTESIAN_POINT ( 'NONE',  ( 157.6875000000000284, 4.242640687119269671, 4.242640687119298093 ) ) ;
#18288 = EDGE_CURVE ( 'NONE', #11814, #25843, #17542, .T. ) ;
#18289 = CARTESIAN_POINT ( 'NONE',  ( 3.175426480543072749, -5.500000000000105693, -117.6250000000000284 ) ) ;
#18290 = CARTESIAN_POINT ( 'NONE',  ( 3.608439182435180470, -6.249999999999997335, -134.5580127018922951 ) ) ;
#18291 = ORIENTED_EDGE ( 'NONE', *, *, #28855, .F. ) ;
#18292 = CARTESIAN_POINT ( 'NONE',  ( -3.464101615137757051, -5.999999999999979572, -57.58632486540518869 ) ) ;
#18293 = CARTESIAN_POINT ( 'NONE',  ( -3.608439182435052128, -6.250000000000110134, -120.4419872981077901 ) ) ;
#18294 = CARTESIAN_POINT ( 'NONE',  ( 7.216878364870455975, -6.409875621278545621E-14, -175.4419872981078470 ) ) ;
#18295 = CARTESIAN_POINT ( 'NONE',  ( 159.6587023700971031, -11.11766146451058113, 4.516663148717062981 ) ) ;
#18296 = CARTESIAN_POINT ( 'NONE',  ( 5.000000000000018652, -5.999999999999914735, 1.056932319443149026E-13 ) ) ;
#18297 = ORIENTED_EDGE ( 'NONE', *, *, #19829, .T. ) ;
#18298 = CARTESIAN_POINT ( 'NONE',  ( 11.81250000000006040, 0.8284271247463557142, -2.000000000000031530 ) ) ;
#18299 = EDGE_CURVE ( 'NONE', #15465, #15294, #25364, .T. ) ;
#18300 = CARTESIAN_POINT ( 'NONE',  ( -5.999999999999963585, -1.487416814333745711E-14, -75.83632486540521711 ) ) ;
#18301 =( BOUNDED_CURVE ( )  B_SPLINE_CURVE ( 2, ( #25562, #7429, #12085, #14393, #2662, #16837, #11784, #19126, #23290 ),
 .UNSPECIFIED., .F., .T. ) 
 B_SPLINE_CURVE_WITH_KNOTS ( ( 3, 2, 2, 2, 3 ),
 ( 0.5194444444444444864, 0.5203703703703703720, 0.5222222222222221433, 0.5240740740740741366, 0.5249999999999999112 ),
 .UNSPECIFIED. ) 
 CURVE ( )  GEOMETRIC_REPRESENTATION_ITEM ( )  RATIONAL_B_SPLINE_CURVE ( ( 0.9330127018922194093, 0.9330127018922194093, 1.000000000000000000, 0.8660254037844388186, 1.000000000000000000, 0.8660254037844388186, 1.000000000000000000, 0.9330127018922274029, 0.9330127018922194093 ) ) 
 REPRESENTATION_ITEM ( '' )  );
#18302 = CARTESIAN_POINT ( 'NONE',  ( 4.884531539228700758, 3.330387827102500253, -180.0000000000000568 ) ) ;
#18303 = FACE_OUTER_BOUND ( 'NONE', #12802, .T. ) ;
#18304 = CARTESIAN_POINT ( 'NONE',  ( 5.999999999999999112, 2.951592740943527306E-14, -150.0863248654052313 ) ) ;
#18305 = CARTESIAN_POINT ( 'NONE',  ( 3.608439182435180470, -6.249999999999997335, -72.19198729810781856 ) ) ;
#18306 = CARTESIAN_POINT ( 'NONE',  ( 5.412658773652712085, -3.125000000000086153, -58.56698729810783277 ) ) ;
#18307 = CARTESIAN_POINT ( 'NONE',  ( -5.999999999999982236, -1.607695154586700426, -121.3466878364870070 ) ) ;
#18308 = CARTESIAN_POINT ( 'NONE',  ( -3.608439182435115633, 6.249999999999965361, -181.8080127018922383 ) ) ;
#18309 = CARTESIAN_POINT ( 'NONE',  ( -5.999999999999963585, 1.780251999655701777E-13, -74.33632486540523132 ) ) ;
#18310 = CARTESIAN_POINT ( 'NONE',  ( 6.000000000000052403, -1.607695154586662678, -123.1533121635129788 ) ) ;
#18311 = DIRECTION ( 'NONE',  ( 1.000000000000000000, 0.000000000000000000, 0.000000000000000000 ) ) ;
#18312 = CARTESIAN_POINT ( 'NONE',  ( -2.775557561562891351E-14, -5.500000000000115463, -125.2500000000000284 ) ) ;
#18313 =( BOUNDED_CURVE ( )  B_SPLINE_CURVE ( 2, ( #10789, #12793, #26862, #26571, #3673, #3364, #19536, #5520, #20138 ),
 .UNSPECIFIED., .F., .T. ) 
 B_SPLINE_CURVE_WITH_KNOTS ( ( 3, 2, 2, 2, 3 ),
 ( 0.7647058823529411242, 0.7720588235294117974, 0.7794117647058823595, 0.7867647058823529216, 0.7941176470588234837 ),
 .UNSPECIFIED. ) 
 CURVE ( )  GEOMETRIC_REPRESENTATION_ITEM ( )  RATIONAL_B_SPLINE_CURVE ( ( 1.000000000000000000, 0.9238795325112867385, 1.000000000000000000, 0.9238795325112867385, 1.000000000000000000, 0.9238795325112867385, 1.000000000000000000, 0.9238795325112867385, 1.000000000000000000 ) ) 
 REPRESENTATION_ITEM ( '' )  );
#18314 = DIRECTION ( 'NONE',  ( -1.000000000000000000, 0.000000000000000000, 0.000000000000000000 ) ) ;
#18315 = VERTEX_POINT ( 'NONE', #6291 ) ;
#18316 = CARTESIAN_POINT ( 'NONE',  ( 20.06250000000002842, -2.649519052838238409, 1.097466725451559322 ) ) ;
#18317 = CARTESIAN_POINT ( 'NONE',  ( 108.2113248654050892, -1.999999999999946265, 0.000000000000000000 ) ) ;
#18318 = CARTESIAN_POINT ( 'NONE',  ( 1.000000000000000888, 0.000000000000000000, 0.000000000000000000 ) ) ;
#18319 = CARTESIAN_POINT ( 'NONE',  ( 137.1711002691896795, 4.999999999999989342, 2.071067811865468400 ) ) ;
#18320 = ORIENTED_EDGE ( 'NONE', *, *, #19792, .T. ) ;
#18321 = CARTESIAN_POINT ( 'NONE',  ( 107.8747167782375840, 0.000000000000000000, 1.849990392679523588 ) ) ;
#18322 = CARTESIAN_POINT ( 'NONE',  ( 6.000000000000000888, -1.859271017917181981E-14, -114.6636751345948255 ) ) ;
#18323 = CARTESIAN_POINT ( 'NONE',  ( 113.7497167782375698, 1.308140751793557266, 1.308140751793751555 ) ) ;
#18324 = CARTESIAN_POINT ( 'NONE',  ( 5.412658773652712085, -3.125000000000086153, -118.5669872981078328 ) ) ;
#18325 = CARTESIAN_POINT ( 'NONE',  ( -5.196152422706601826, 2.999999999999975131, -108.0386751345948682 ) ) ;
#18326 = COLOUR_RGB ( '', 0.40784314, 0.44705882, 0.49803922) ;
#18327 = CARTESIAN_POINT ( 'NONE',  ( 104.7401757384975127, 1.770091586386960403, 0.5493589524125325196 ) ) ;
#18328 = ORIENTED_EDGE ( 'NONE', *, *, #5580, .T. ) ;
#18329 = ORIENTED_EDGE ( 'NONE', *, *, #24019, .T. ) ;
#18330 = DIRECTION ( 'NONE',  ( -7.147005652999508048E-36, 5.642372883946980038E-36, 1.000000000000000000 ) ) ;
#18331 = CARTESIAN_POINT ( 'NONE',  ( 144.9375000000000284, -4.242640687119298093, -4.242640687119298093 ) ) ;
#18332 = EDGE_CURVE ( 'NONE', #16343, #5531, #3520, .T. ) ;
#18333 = CARTESIAN_POINT ( 'NONE',  ( 3.608439182435180470, 6.249999999999982236, -151.1919872981078186 ) ) ;
#18334 = ORIENTED_EDGE ( 'NONE', *, *, #10438, .F. ) ;
#18335 = CARTESIAN_POINT ( 'NONE',  ( -38.99999999999998579, -59.99999999999980105, 4.000000000000003553 ) ) ;
#18336 = CARTESIAN_POINT ( 'NONE',  ( 23.62500000000000711, -1.414213562372923505, -1.414213562373145550 ) ) ;
#18337 = EDGE_CURVE ( 'NONE', #5051, #16955, #26322, .T. ) ;
#18338 = CARTESIAN_POINT ( 'NONE',  ( 124.9999999999999432, -69.50000000000000000, 7.500000000000007105 ) ) ;
#18339 = CARTESIAN_POINT ( 'NONE',  ( 3.608439182435180470, -6.249999999999997335, -70.05801270189228092 ) ) ;
#18340 = PRESENTATION_LAYER_ASSIGNMENT (  '', '', ( #4555 ) ) ;
#18341 = EDGE_CURVE ( 'NONE', #27528, #25684, #16151, .T. ) ;
#18342 = CARTESIAN_POINT ( 'NONE',  ( 143.1413997308104342, 2.071067811865468400, -4.999999999999989342 ) ) ;
#18343 = DIRECTION ( 'NONE',  ( 0.000000000000000000, 0.000000000000000000, 1.000000000000000000 ) ) ;
#18344 = CARTESIAN_POINT ( 'NONE',  ( 111.7113248654050892, 2.000000000000057288, 0.000000000000000000 ) ) ;
#18345 = CARTESIAN_POINT ( 'NONE',  ( 12.47617513459493921, 1.035533905932869425, 2.499999999999844569 ) ) ;
#18346 = SURFACE_STYLE_FILL_AREA ( #8640 ) ;
#18347 = CARTESIAN_POINT ( 'NONE',  ( 110.4374999999997442, -2.500000000000024425, 1.035533905932809473 ) ) ;
#18348 = CARTESIAN_POINT ( 'NONE',  ( 3.464101615137757051, -5.999999999999979572, -94.83632486540517448 ) ) ;
#18349 = CARTESIAN_POINT ( 'NONE',  ( 4.763139720814407951, 2.750000000000002665, -124.7500000000000284 ) ) ;
#18350 = DIRECTION ( 'NONE',  ( -7.147005652999508048E-36, 5.642372883946980038E-36, 1.000000000000000000 ) ) ;
#18351 = ORIENTED_EDGE ( 'NONE', *, *, #21571, .T. ) ;
#18352 = CARTESIAN_POINT ( 'NONE',  ( 3.175426480543072749, -5.500000000000105693, -54.62500000000003553 ) ) ;
#18353 = CARTESIAN_POINT ( 'NONE',  ( 5.196152422706629359, -2.999999999999988898, -153.7886751345948255 ) ) ;
#18354 = CARTESIAN_POINT ( 'NONE',  ( -5.196152422706601826, 2.999999999999975131, -171.9613248654052313 ) ) ;
#18355 = CARTESIAN_POINT ( 'NONE',  ( 5.196152422706629359, -2.999999999999988898, -151.7113248654052313 ) ) ;
#18356 = ORIENTED_EDGE ( 'NONE', *, *, #26976, .F. ) ;
#18357 = CARTESIAN_POINT ( 'NONE',  ( 105.7499999999998010, 1.110223024625156540E-13, -2.499999999999946709 ) ) ;
#18358 = CARTESIAN_POINT ( 'NONE',  ( 138.5625000000000284, -4.242640687119298093, 4.242640687119298093 ) ) ;
#18359 = CARTESIAN_POINT ( 'NONE',  ( 140.5835741348633690, -11.79178706743166494, -4.000000000000005329 ) ) ;
#18360 = CARTESIAN_POINT ( 'NONE',  ( 137.8125000000000284, 4.242640687119298093, -4.242640687119298093 ) ) ;
#18361 = CARTESIAN_POINT ( 'NONE',  ( 14.33632486540525974, -1.767766952966376426, -1.767766952966320915 ) ) ;
#18362 = CIRCLE ( 'NONE', #12971, 15.00000000000000000 ) ;
#18363 = ADVANCED_FACE ( 'NONE', ( #24571 ), #13402, .F. ) ;
#18364 = CARTESIAN_POINT ( 'NONE',  ( 3.175426480543072749, -5.500000000000105693, -134.1250000000000284 ) ) ;
#18365 = EDGE_LOOP ( 'NONE', ( #21843, #17986, #2906, #27904 ) ) ;
#18366 = CARTESIAN_POINT ( 'NONE',  ( 14.50000000000012434, -1.999999999999779732, -5.551115123125782702E-14 ) ) ;
#18367 = ORIENTED_EDGE ( 'NONE', *, *, #2585, .T. ) ;
#18368 = CARTESIAN_POINT ( 'NONE',  ( -6.350852961085760029, -1.281975124255709124E-13, -64.12500000000001421 ) ) ;
#18369 = CARTESIAN_POINT ( 'NONE',  ( -5.999999999999962697, -1.607695154586733288, -164.8466878364870354 ) ) ;
#18370 = EDGE_CURVE ( 'NONE', #21808, #20687, #20064, .T. ) ;
#18371 = CARTESIAN_POINT ( 'NONE',  ( 2.775557561562891351E-14, 6.250000000000033751, -90.43301270189225249 ) ) ;
#18372 = LINE ( 'NONE', #10852, #10375 ) ;
#18373 = CARTESIAN_POINT ( 'NONE',  ( 6.000000000000000888, 1.743066579297358182E-13, -81.08632486540518869 ) ) ;
#18374 = CARTESIAN_POINT ( 'NONE',  ( 140.0000000000000284, -54.99999999999990763, -5.000000000000004441 ) ) ;
#18375 = CARTESIAN_POINT ( 'NONE',  ( 119.0627832217622739, -0.7662911109077388261, -1.849990392679291551 ) ) ;
#18376 = CARTESIAN_POINT ( 'NONE',  ( -3.175426480542816066, 5.499999999999865885, -148.3750000000000000 ) ) ;
#18377 = CARTESIAN_POINT ( 'NONE',  ( 3.608439182435180470, -6.249999999999997335, -164.5580127018922099 ) ) ;
#18378 = CARTESIAN_POINT ( 'NONE',  ( -0.2114713642193710996, -9.788528635780624043, 4.341247053692733004 ) ) ;
#18379 = CARTESIAN_POINT ( 'NONE',  ( 0.000000000000000000, 5.499999999999991118, -180.0000000000000568 ) ) ;
#18380 = CARTESIAN_POINT ( 'NONE',  ( -4.763139720814407951, -2.750000000000016431, -80.50000000000001421 ) ) ;
#18381 = FILL_AREA_STYLE ('',( #13329 ) ) ;
#18382 = CARTESIAN_POINT ( 'NONE',  ( 3.175426480543072749, -5.500000000000105693, -69.62500000000004263 ) ) ;
#18383 = CARTESIAN_POINT ( 'NONE',  ( 147.6711002691896510, 4.999999999999989342, 2.071067811865468400 ) ) ;
#18384 = CARTESIAN_POINT ( 'NONE',  ( -5.196152422706573404, -3.000000000000002665, -114.7113248654052455 ) ) ;
#18385 = DIRECTION ( 'NONE',  ( 0.000000000000000000, 0.000000000000000000, -1.000000000000000000 ) ) ;
#18386 = CARTESIAN_POINT ( 'NONE',  ( -5.999999999999956479, -1.607695154586745057, -71.84668783648706381 ) ) ;
#18387 = CARTESIAN_POINT ( 'NONE',  ( 0.000000000000000000, 0.000000000000000000, 0.000000000000000000 ) ) ;
#18388 = CARTESIAN_POINT ( 'NONE',  ( 18.43749999999999289, -1.999999999999971800, 0.8284271247462354770 ) ) ;
#18389 = DIRECTION ( 'NONE',  ( -1.000000000000000000, -1.665334536937731113E-16, 1.526556658859586792E-16 ) ) ;
#18390 = CARTESIAN_POINT ( 'NONE',  ( 116.8122167782373992, 0.7662911109079189043, 1.849990392679652151 ) ) ;
#18391 = DIRECTION ( 'NONE',  ( 0.8660254037844379305, 0.5000000000000011102, 6.363854784884201318E-16 ) ) ;
#18392 =( BOUNDED_CURVE ( )  B_SPLINE_CURVE ( 2, ( #25799, #14176, #23513, #25646, #19066, #9528, #25480, #7057, #28237 ),
 .UNSPECIFIED., .F., .T. ) 
 B_SPLINE_CURVE_WITH_KNOTS ( ( 3, 2, 2, 2, 3 ),
 ( 0.4305555555555555802, 0.4314814814814814659, 0.4333333333333333481, 0.4351851851851851749, 0.4361111111111111160 ),
 .UNSPECIFIED. ) 
 CURVE ( )  GEOMETRIC_REPRESENTATION_ITEM ( )  RATIONAL_B_SPLINE_CURVE ( ( 0.9330127018922194093, 0.9330127018922214077, 1.000000000000000000, 0.8660254037844388186, 1.000000000000000000, 0.8660254037844388186, 1.000000000000000000, 0.9330127018922194093, 0.9330127018922194093 ) ) 
 REPRESENTATION_ITEM ( '' )  );
#18393 = ORIENTED_EDGE ( 'NONE', *, *, #25628, .F. ) ;
#18394 = CARTESIAN_POINT ( 'NONE',  ( 159.0000000000000284, 6.000000000000005329, 0.000000000000000000 ) ) ;
#18395 = CARTESIAN_POINT ( 'NONE',  ( 0.000000000000000000, 0.000000000000000000, -14.99152654425661702 ) ) ;
#18396 = CARTESIAN_POINT ( 'NONE',  ( 115.8752832217622313, -1.849990392679468076, 1.110223024625156540E-13 ) ) ;
#18397 = EDGE_CURVE ( 'NONE', #28105, #2458, #6510, .T. ) ;
#18398 = CARTESIAN_POINT ( 'NONE',  ( 11.58632486540531126, 1.767766952966487448, -1.767766952966431937 ) ) ;
#18399 = ORIENTED_EDGE ( 'NONE', *, *, #22087, .F. ) ;
#18400 = EDGE_LOOP ( 'NONE', ( #18713, #8980, #14114, #29847, #20065 ) ) ;
#18401 = ADVANCED_FACE ( 'NONE', ( #11707 ), #25337, .F. ) ;
#18402 = EDGE_LOOP ( 'NONE', ( #6268, #28653, #4087, #6845, #16330 ) ) ;
#18403 = CARTESIAN_POINT ( 'NONE',  ( 0.000000000000000000, 5.499999999999991118, -93.00000000000002842 ) ) ;
#18404 = AXIS2_PLACEMENT_3D ( 'NONE', #11321, #1451, #13184 ) ;
#18405 = CARTESIAN_POINT ( 'NONE',  ( 3.608439182435180470, 6.249999999999982236, -105.5580127018922667 ) ) ;
#18406 = LINE ( 'NONE', #6092, #8840 ) ;
#18407 = CARTESIAN_POINT ( 'NONE',  ( 6.000000000000000888, 7.762456499804234384E-14, -143.1636751345948255 ) ) ;
#18408 = CARTESIAN_POINT ( 'NONE',  ( 3.033369321062211466, -10.57893614291642059, -30.19141222485919585 ) ) ;
#18409 = VERTEX_POINT ( 'NONE', #23363 ) ;
#18410 = CARTESIAN_POINT ( 'NONE',  ( 161.0000000000000284, 0.000000000000000000, -12.00000000000000178 ) ) ;
#18411 = CARTESIAN_POINT ( 'NONE',  ( -2.775557561562891351E-14, -5.500000000000115463, -170.2500000000000000 ) ) ;
#18412 = CARTESIAN_POINT ( 'NONE',  ( 23.35117513459490368, 2.500000000000084821, 1.035533905932749299 ) ) ;
#18413 = CARTESIAN_POINT ( 'NONE',  ( -6.350852961085760029, -1.281975124255709124E-13, -164.6249999999999716 ) ) ;
#18414 = CARTESIAN_POINT ( 'NONE',  ( 116.6874999999997726, -1.035533905932659149, -2.499999999999784173 ) ) ;
#18415 =( LENGTH_UNIT ( ) NAMED_UNIT ( * ) SI_UNIT ( .MILLI., .METRE. ) );
#18416 = CARTESIAN_POINT ( 'NONE',  ( 6.000000000000007105, -1.607695154586741060, -165.7306624327025872 ) ) ;
#18417 = CARTESIAN_POINT ( 'NONE',  ( 0.000000000000000000, 5.499999999999991118, -97.50000000000002842 ) ) ;
#18418 = CARTESIAN_POINT ( 'NONE',  ( 162.2023502691896795, 0.000000000000000000, -5.000000000000004441 ) ) ;
#18419 = CARTESIAN_POINT ( 'NONE',  ( -0.07939152865813971227, -15.22963250115830292, 7.558609509503281032 ) ) ;
#18420 = ORIENTED_EDGE ( 'NONE', *, *, #25836, .T. ) ;
#18421 = CARTESIAN_POINT ( 'NONE',  ( 117.6250000000000000, -1.767766952966376426, -1.767766952966320915 ) ) ;
#18422 = CARTESIAN_POINT ( 'NONE',  ( -5.196152422706573404, -3.000000000000002665, -161.7886751345948255 ) ) ;
#18423 = CARTESIAN_POINT ( 'NONE',  ( 107.7502832217622881, -1.308140751793585022, 1.308140751793751555 ) ) ;
#18424 = DIRECTION ( 'NONE',  ( 0.000000000000000000, 1.000000000000000000, -0.000000000000000000 ) ) ;
#18425 = ORIENTED_EDGE ( 'NONE', *, *, #23147, .T. ) ;
#18426 = CIRCLE ( 'NONE', #5134, 4.000000000000010658 ) ;
#18427 = CARTESIAN_POINT ( 'NONE',  ( 0.000000000000000000, 5.999999999999977796, -112.2113248654051887 ) ) ;
#18428 = CARTESIAN_POINT ( 'NONE',  ( 7.216878364870455975, -6.409875621278545621E-14, -88.44198729810783277 ) ) ;
#18429 = VERTEX_POINT ( 'NONE', #27623 ) ;
#18430 = CARTESIAN_POINT ( 'NONE',  ( 5.196152422706629359, -2.999999999999988898, -75.21132486540521711 ) ) ;
#18431 = EDGE_CURVE ( 'NONE', #2429, #278, #19055, .T. ) ;
#18432 = PRESENTATION_LAYER_ASSIGNMENT (  '', '', ( #6122 ) ) ;
#18433 = VERTEX_POINT ( 'NONE', #15873 ) ;
#18434 = CARTESIAN_POINT ( 'NONE',  ( 148.2187500000000568, 2.485281374238555774, -6.000000000000005329 ) ) ;
#18435 = ORIENTED_EDGE ( 'NONE', *, *, #10984, .F. ) ;
#18436 = CIRCLE ( 'NONE', #5146, 9.999999999999998224 ) ;
#18437 =( BOUNDED_CURVE ( )  B_SPLINE_CURVE ( 2, ( #14394, #356, #14101, #11947, #9288, #30173, #9137, #18529, #6976 ),
 .UNSPECIFIED., .F., .F. ) 
 B_SPLINE_CURVE_WITH_KNOTS ( ( 3, 2, 2, 2, 3 ),
 ( 0.3194444444444445308, 0.3203703703703704164, 0.3222222222222221877, 0.3240740740740740700, 0.3249999999999999556 ),
 .UNSPECIFIED. ) 
 CURVE ( )  GEOMETRIC_REPRESENTATION_ITEM ( )  RATIONAL_B_SPLINE_CURVE ( ( 0.9330127018922194093, 0.9330127018922234061, 1.000000000000000000, 0.8660254037844388186, 1.000000000000000000, 0.8660254037844388186, 1.000000000000000000, 0.9330127018922234061, 0.9330127018922194093 ) ) 
 REPRESENTATION_ITEM ( '' )  );
#18438 = CARTESIAN_POINT ( 'NONE',  ( 4.763139720814407951, -2.749999999999988454, -123.5000000000000568 ) ) ;
#18439 = CARTESIAN_POINT ( 'NONE',  ( 23.06250000000007816, -1.097466725451379244, -2.649519052838358757 ) ) ;
#18440 = CARTESIAN_POINT ( 'NONE',  ( 7.216878364870455975, -6.409875621278545621E-14, -134.3080127018922667 ) ) ;
#18441 = EDGE_LOOP ( 'NONE', ( #12762, #13690, #19207, #1362, #23451, #29155, #18291 ) ) ;
#18442 = DIRECTION ( 'NONE',  ( 1.000000000000000000, -5.551115123125773458E-17, -1.260129944081490338E-35 ) ) ;
#18443 = CARTESIAN_POINT ( 'NONE',  ( 5.412658773652712085, -3.125000000000086153, -169.5669872981078186 ) ) ;
#18444 = CARTESIAN_POINT ( 'NONE',  ( -7.216878364870328078, 0.000000000000000000, -173.1919872981078754 ) ) ;
#18445 = CARTESIAN_POINT ( 'NONE',  ( 159.0677334129669873, -12.00000000265806754, 4.000000000000004441 ) ) ;
#18446 = DIRECTION ( 'NONE',  ( -7.147005652999508048E-36, 5.642372883946980038E-36, 1.000000000000000000 ) ) ;
#18447 = ORIENTED_EDGE ( 'NONE', *, *, #17696, .F. ) ;
#18448 = FACE_OUTER_BOUND ( 'NONE', #24424, .T. ) ;
#18449 = DIRECTION ( 'NONE',  ( -0.000000000000000000, -1.000000000000000000, 0.000000000000000000 ) ) ;
#18450 = CARTESIAN_POINT ( 'NONE',  ( -5.999999999999963585, -1.487416814333745711E-14, -132.8363248654052597 ) ) ;
#18451 = CARTESIAN_POINT ( 'NONE',  ( 23.14882486540521711, -2.499999999999964473, 1.035533905932749299 ) ) ;
#18452 = CARTESIAN_POINT ( 'NONE',  ( 110.3752832217623592, 1.849990392679495832, 0.000000000000000000 ) ) ;
#18453 = CARTESIAN_POINT ( 'NONE',  ( -3.608439182435052128, -6.250000000000110134, -75.44198729810784698 ) ) ;
#18454 = CARTESIAN_POINT ( 'NONE',  ( -7.216878364870328078, 0.000000000000000000, -63.69198729810785409 ) ) ;
#18455 = CARTESIAN_POINT ( 'NONE',  ( -3.175426480542816510, -5.500000000000057732, -51.87500000000002132 ) ) ;
#18456 = CARTESIAN_POINT ( 'NONE',  ( 6.000000000000000888, 1.743066579297358182E-13, -103.5863248654052171 ) ) ;
#18457 = CARTESIAN_POINT ( 'NONE',  ( 0.000000000000000000, -5.999999999999991118, -123.4613248654052313 ) ) ;
#18458 = CARTESIAN_POINT ( 'NONE',  ( 6.000000000000052403, -1.607695154586662678, -53.23066243270259434 ) ) ;
#18459 = CARTESIAN_POINT ( 'NONE',  ( 4.763139720814407951, 2.750000000000002665, -121.7500000000000284 ) ) ;
#18460 = CARTESIAN_POINT ( 'NONE',  ( 114.6636751345947829, -1.414213562373034527, 1.414213562373367594 ) ) ;
#18461 = VERTEX_POINT ( 'NONE', #21052 ) ;
#18462 = CARTESIAN_POINT ( 'NONE',  ( 22.00000000000015987, -1.873492889144789952, 1.873492889144900975 ) ) ;
#18463 = EDGE_CURVE ( 'NONE', #15450, #18409, #13555, .T. ) ;
#18464 = CARTESIAN_POINT ( 'NONE',  ( 6.000000000000000888, 1.607695154586715303, -105.5966878364870496 ) ) ;
#18465 = ORIENTED_EDGE ( 'NONE', *, *, #27676, .F. ) ;
#18466 = CARTESIAN_POINT ( 'NONE',  ( 109.8747167782376124, -2.775557561562891351E-14, 1.849990392679523588 ) ) ;
#18467 = CARTESIAN_POINT ( 'NONE',  ( -3.464101615137725076, 5.999999999999979572, -121.6636751345947971 ) ) ;
#18468 = CARTESIAN_POINT ( 'NONE',  ( 112.9997167782376835, -1.308140751793557266, 1.308140751793751555 ) ) ;
#18469 = CARTESIAN_POINT ( 'NONE',  ( -3.608439182435052128, -6.250000000000110134, -109.9419872981078043 ) ) ;
#18470 = CARTESIAN_POINT ( 'NONE',  ( 17.08632486540531659, -1.767766952966209892, 1.767766952966431937 ) ) ;
#18471 = EDGE_CURVE ( 'NONE', #26763, #4156, #4136, .T. ) ;
#18472 = EDGE_CURVE ( 'NONE', #20769, #7022, #25644, .T. ) ;
#18473 = CARTESIAN_POINT ( 'NONE',  ( 104.7401757384972996, 1.536076471655371645, 1.055243095569078138 ) ) ;
#18474 = ORIENTED_EDGE ( 'NONE', *, *, #19591, .T. ) ;
#18475 = VERTEX_POINT ( 'NONE', #18309 ) ;
#18476 = DIRECTION ( 'NONE',  ( 0.000000000000000000, 5.551115123125767911E-17, -1.000000000000000000 ) ) ;
#18477 = PRESENTATION_LAYER_ASSIGNMENT (  '', '', ( #12109 ) ) ;
#18478 = CARTESIAN_POINT ( 'NONE',  ( 135.3750000000000284, 0.000000000000000000, 6.000000000000005329 ) ) ;
#18479 =( BOUNDED_CURVE ( )  B_SPLINE_CURVE ( 2, ( #29865, #15640, #12873, #1145, #13482, #15331, #4059, #24652, #22822 ),
 .UNSPECIFIED., .F., .T. ) 
 B_SPLINE_CURVE_WITH_KNOTS ( ( 3, 2, 2, 2, 3 ),
 ( 0.8750000000000000000, 0.8759259259259258856, 0.8777777777777777679, 0.8796296296296296502, 0.8805555555555555358 ),
 .UNSPECIFIED. ) 
 CURVE ( )  GEOMETRIC_REPRESENTATION_ITEM ( )  RATIONAL_B_SPLINE_CURVE ( ( 0.9330127018922194093, 0.9330127018922194093, 1.000000000000000000, 0.8660254037844388186, 1.000000000000000000, 0.8660254037844388186, 1.000000000000000000, 0.9330127018922234061, 0.9330127018922194093 ) ) 
 REPRESENTATION_ITEM ( '' )  );
#18480 = ORIENTED_EDGE ( 'NONE', *, *, #2357, .F. ) ;
#18481 = CARTESIAN_POINT ( 'NONE',  ( 5.412658773652712085, -3.125000000000086153, -136.5669872981077901 ) ) ;
#18482 = SURFACE_SIDE_STYLE ('',( #13581 ) ) ;
#18483 = CARTESIAN_POINT ( 'NONE',  ( 124.9999999999999432, -70.00000000000000000, 8.000000000000007105 ) ) ;
#18484 = CARTESIAN_POINT ( 'NONE',  ( 23.00000000000013145, 2.000000000000168310, 0.000000000000000000 ) ) ;
#18485 = CARTESIAN_POINT ( 'NONE',  ( 6.000000000000000888, -1.859271017917181981E-14, -120.6636751345948255 ) ) ;
#18486 = CARTESIAN_POINT ( 'NONE',  ( 3.464101615137757051, -5.999999999999979572, -137.4136751345947971 ) ) ;
#18487 = CARTESIAN_POINT ( 'NONE',  ( 3.608439182435180470, -6.249999999999997335, -67.05801270189226670 ) ) ;
#18488 =( BOUNDED_CURVE ( )  B_SPLINE_CURVE ( 2, ( #13507, #29159, #14921, #15071, #29318, #12629, #8276, #29011, #20540 ),
 .UNSPECIFIED., .F., .T. ) 
 B_SPLINE_CURVE_WITH_KNOTS ( ( 3, 2, 2, 2, 3 ),
 ( 0.07500000000000006661, 0.07592592592592595224, 0.07777777777777772350, 0.07962962962962960578, 0.08055555555555549141 ),
 .UNSPECIFIED. ) 
 CURVE ( )  GEOMETRIC_REPRESENTATION_ITEM ( )  RATIONAL_B_SPLINE_CURVE ( ( 0.9330127018922194093, 0.9330127018922234061, 1.000000000000000000, 0.8660254037844388186, 1.000000000000000000, 0.8660254037844388186, 1.000000000000000000, 0.9330127018922234061, 0.9330127018922194093 ) ) 
 REPRESENTATION_ITEM ( '' )  );
#18489 = CARTESIAN_POINT ( 'NONE',  ( 146.1413997308104058, 2.071067811865468400, -4.999999999999989342 ) ) ;
#18490 = CARTESIAN_POINT ( 'NONE',  ( 111.8511751345945839, -2.000000000000061728, -0.8284271247458748766 ) ) ;
#18491 = DIRECTION ( 'NONE',  ( -1.000000000000000000, 0.000000000000000000, 0.000000000000000000 ) ) ;
#18492 = LINE ( 'NONE', #23246, #10970 ) ;
#18493 = CARTESIAN_POINT ( 'NONE',  ( 156.0074251345948824, 2.278174593052074925, -5.499999999999950262 ) ) ;
#18494 = CARTESIAN_POINT ( 'NONE',  ( -5.196152422706573404, -3.000000000000002665, -67.28867513459479710 ) ) ;
#18495 = CARTESIAN_POINT ( 'NONE',  ( 108.6249999999999289, -1.767766952966320915, -1.767766952966320915 ) ) ;
#18496 = CARTESIAN_POINT ( 'NONE',  ( 106.4761751345946834, 0.8284271247463257382, 2.000000000000091926 ) ) ;
#18497 = CARTESIAN_POINT ( 'NONE',  ( 4.763139720814407951, -2.749999999999988454, -122.0000000000000000 ) ) ;
#18498 = CARTESIAN_POINT ( 'NONE',  ( 6.055081547227420202, -9.714451465470096063E-16, 17.50000000000000000 ) ) ;
#18499 = CARTESIAN_POINT ( 'NONE',  ( 0.000000000000000000, 0.000000000000000000, 0.000000000000000000 ) ) ;
#18500 = ORIENTED_EDGE ( 'NONE', *, *, #28478, .T. ) ;
#18501 = ADVANCED_FACE ( 'NONE', ( #23054 ), #14021, .T. ) ;
#18502 = CARTESIAN_POINT ( 'NONE',  ( 4.763139720814407951, -2.749999999999988454, -57.49999999999999289 ) ) ;
#18503 = DIRECTION ( 'NONE',  ( -1.000000000000000000, -0.000000000000000000, -0.000000000000000000 ) ) ;
#18504 = CARTESIAN_POINT ( 'NONE',  ( 5.196152422706629359, -2.999999999999988898, -163.7113248654051745 ) ) ;
#18505 = EDGE_LOOP ( 'NONE', ( #28255, #20184, #3345, #3926 ) ) ;
#18506 = CARTESIAN_POINT ( 'NONE',  ( 106.7499999999999147, -8.326672684688674053E-14, -2.499999999999946709 ) ) ;
#18507 = CARTESIAN_POINT ( 'NONE',  ( 138.1875000000000284, 4.242640687119269671, 4.242640687119298093 ) ) ;
#18508 = CARTESIAN_POINT ( 'NONE',  ( 0.000000000000000000, 5.999999999999977796, -46.21132486540524553 ) ) ;
#18509 = EDGE_CURVE ( 'NONE', #15347, #11375, #24403, .T. ) ;
#18510 = EDGE_CURVE ( 'NONE', #6339, #10447, #12454, .T. ) ;
#18511 = CARTESIAN_POINT ( 'NONE',  ( 138.5625000000000284, -4.242640687119298093, 4.242640687119298093 ) ) ;
#18512 = CARTESIAN_POINT ( 'NONE',  ( 141.0000000000000284, -12.00000000000001066, -4.000000000000003553 ) ) ;
#18513 = CARTESIAN_POINT ( 'NONE',  ( 0.000000000000000000, 5.499999999999991118, -135.0000000000000000 ) ) ;
#18514 = ORIENTED_EDGE ( 'NONE', *, *, #22000, .T. ) ;
#18515 =( GEOMETRIC_REPRESENTATION_CONTEXT ( 3 ) GLOBAL_UNCERTAINTY_ASSIGNED_CONTEXT ( ( #12253 ) ) GLOBAL_UNIT_ASSIGNED_CONTEXT ( ( #4803, #45, #491 ) ) REPRESENTATION_CONTEXT ( 'NONE', 'WORKASPACE' ) );
#18516 = CARTESIAN_POINT ( 'NONE',  ( 12.62500000000013678, -1.414213562372979016, -1.414213562373145550 ) ) ;
#18517 = ORIENTED_EDGE ( 'NONE', *, *, #2292, .T. ) ;
#18518 = CARTESIAN_POINT ( 'NONE',  ( 6.350852961086080661, -9.614813431917819062E-14, -66.37500000000004263 ) ) ;
#18519 = CARTESIAN_POINT ( 'NONE',  ( 5.196152422706629359, -2.999999999999988898, -164.2886751345948824 ) ) ;
#18520 = CARTESIAN_POINT ( 'NONE',  ( 140.0769230769231228, -11.53846153846155254, 4.615384615384604317 ) ) ;
#18521 = CARTESIAN_POINT ( 'NONE',  ( 0.000000000000000000, 5.999999999999977796, -150.2886751345948255 ) ) ;
#18522 = CARTESIAN_POINT ( 'NONE',  ( -5.999999999999963585, 0.000000000000000000, -179.9136751345948255 ) ) ;
#18523 = CARTESIAN_POINT ( 'NONE',  ( 120.1252832217621176, -5.551115123125782702E-14, -1.849990392679523588 ) ) ;
#18524 = CARTESIAN_POINT ( 'NONE',  ( 6.350852961086080661, -9.614813431917819062E-14, -144.3750000000000853 ) ) ;
#18525 = CARTESIAN_POINT ( 'NONE',  ( 2.081668171172167281E-16, 3.582034040661430693E-16, -2.499999999999999112 ) ) ;
#18526 = CARTESIAN_POINT ( 'NONE',  ( -3.175426480542816510, 5.499999999999865885, -142.3750000000000568 ) ) ;
#18527 = CARTESIAN_POINT ( 'NONE',  ( 2.775557561562891351E-14, 6.250000000000033751, -163.9330127018922667 ) ) ;
#18528 = CARTESIAN_POINT ( 'NONE',  ( 21.99999999999993605, -11.00000000000004086, -14.99152654425661879 ) ) ;
#18529 = CARTESIAN_POINT ( 'NONE',  ( 5.999999999999949374, 1.607695154586804565, -90.01933756729741276 ) ) ;
#18530 = EDGE_CURVE ( 'NONE', #7379, #1437, #19102, .T. ) ;
#18531 = CARTESIAN_POINT ( 'NONE',  ( -6.350852961085760029, -1.281975124255709124E-13, -77.62500000000001421 ) ) ;
#18532 = VECTOR ( 'NONE', #3985, 1000.000000000000000 ) ;
#18533 = CARTESIAN_POINT ( 'NONE',  ( 4.763139720814407951, -2.749999999999988454, -72.50000000000001421 ) ) ;
#18534 = CARTESIAN_POINT ( 'NONE',  ( 5.196152422706629359, -2.999999999999988898, -156.2113248654052313 ) ) ;
#18535 = DIRECTION ( 'NONE',  ( 0.000000000000000000, -1.000000000000000000, 0.000000000000000000 ) ) ;
#18536 = CARTESIAN_POINT ( 'NONE',  ( 111.7886751345948255, -1.999999999999974021, 0.000000000000000000 ) ) ;
#18537 = CARTESIAN_POINT ( 'NONE',  ( 156.3750000000000284, 0.000000000000000000, 6.000000000000005329 ) ) ;
#18538 = DIRECTION ( 'NONE',  ( 0.000000000000000000, 5.551115123125767911E-17, -1.000000000000000000 ) ) ;
#18539 = CARTESIAN_POINT ( 'NONE',  ( 20.56250000000014566, -1.999999999999911626, -0.8284271247462354770 ) ) ;
#18540 = CARTESIAN_POINT ( 'NONE',  ( -2.081668171172168020E-16, -5.204170427930420051E-17, 2.499999999999999112 ) ) ;
#18541 = CARTESIAN_POINT ( 'NONE',  ( -3.464101615137757051, -5.999999999999979572, -147.5863248654051745 ) ) ;
#18542 = CARTESIAN_POINT ( 'NONE',  ( 118.2497167782374419, -1.308140751793585022, -1.308140751793640533 ) ) ;
#18543 = ADVANCED_FACE ( 'NONE', ( #14888 ), #4888, .F. ) ;
#18544 = CARTESIAN_POINT ( 'NONE',  ( 0.000000000000000000, 5.999999999999977796, -139.2113248654052313 ) ) ;
#18545 = ORIENTED_EDGE ( 'NONE', *, *, #13344, .T. ) ;
#18546 = CARTESIAN_POINT ( 'NONE',  ( 154.8750000000000284, 0.000000000000000000, 6.000000000000005329 ) ) ;
#18547 = CARTESIAN_POINT ( 'NONE',  ( 5.196152422706629359, -2.999999999999988898, -156.7886751345948255 ) ) ;
#18548 = CARTESIAN_POINT ( 'NONE',  ( 113.6877832217621460, -0.7662911109077987781, 1.849990392679591977 ) ) ;
#18549 = CARTESIAN_POINT ( 'NONE',  ( 6.000000000000000888, -3.330669073875464691E-16, -7.560779664488942560E-35 ) ) ;
#18550 = ORIENTED_EDGE ( 'NONE', *, *, #8515, .T. ) ;
#18551 = ORIENTED_EDGE ( 'NONE', *, *, #6216, .F. ) ;
#18552 = VERTEX_POINT ( 'NONE', #7646 ) ;
#18553 = CARTESIAN_POINT ( 'NONE',  ( -4.763139720814407951, -2.750000000000016431, -86.50000000000002842 ) ) ;
#18554 = PRESENTATION_LAYER_ASSIGNMENT (  '', '', ( #21485 ) ) ;
#18555 = CARTESIAN_POINT ( 'NONE',  ( 2.775557561562891351E-14, -6.250000000000061284, -107.6830127018922383 ) ) ;
#18556 = CARTESIAN_POINT ( 'NONE',  ( 6.000643140593935776, 9.219125907743233483, -25.38858793365676192 ) ) ;
#18557 = DIRECTION ( 'NONE',  ( 0.000000000000000000, 0.5151515151515151381, -0.8570991287109668288 ) ) ;
#18558 = CARTESIAN_POINT ( 'NONE',  ( 3.175426480543072749, 5.499999999999865885, -165.1249999999999716 ) ) ;
#18559 = CARTESIAN_POINT ( 'NONE',  ( 2.775557561562891351E-14, 6.250000000000033751, -46.93301270189220986 ) ) ;
#18560 = ORIENTED_EDGE ( 'NONE', *, *, #22645, .T. ) ;
#18561 = DIRECTION ( 'NONE',  ( 0.000000000000000000, 1.224646799147351482E-16, 1.000000000000000000 ) ) ;
#18562 = CARTESIAN_POINT ( 'NONE',  ( 148.5863248654052313, 0.000000000000000000, 5.500000000000005329 ) ) ;
#18563 = CARTESIAN_POINT ( 'NONE',  ( 6.350852961086080661, -9.614813431917819062E-14, -169.8750000000000853 ) ) ;
#18564 = DIRECTION ( 'NONE',  ( -7.147005652999508048E-36, 5.642372883946980038E-36, 1.000000000000000000 ) ) ;
#18565 = CARTESIAN_POINT ( 'NONE',  ( -4.763139720814407951, 2.749999999999946709, -164.7500000000000000 ) ) ;
#18566 = CARTESIAN_POINT ( 'NONE',  ( 111.2499999999999432, -1.110223024625156540E-13, 2.500000000000057732 ) ) ;
#18567 = ADVANCED_FACE ( 'NONE', ( #24229 ), #2594, .T. ) ;
#18568 = CARTESIAN_POINT ( 'NONE',  ( -2.775557561562891351E-14, -5.500000000000115463, -99.75000000000000000 ) ) ;
#18569 = FILL_AREA_STYLE ('',( #14280 ) ) ;
#18570 = CARTESIAN_POINT ( 'NONE',  ( 3.464101615137852974, 5.999999999999884537, -87.41367513459482552 ) ) ;
#18571 = ADVANCED_FACE ( 'NONE', ( #26529 ), #2888, .F. ) ;
#18572 = CARTESIAN_POINT ( 'NONE',  ( 3.175426480543072749, 5.499999999999865885, -94.62500000000002842 ) ) ;
#18573 =( BOUNDED_CURVE ( )  B_SPLINE_CURVE ( 2, ( #10568, #24372, #17195, #20082, #12742, #29426, #29116, #10889, #22386 ),
 .UNSPECIFIED., .F., .T. ) 
 B_SPLINE_CURVE_WITH_KNOTS ( ( 3, 2, 2, 2, 3 ),
 ( 0.7031250000000000000, 0.7109375000000000000, 0.7187500000000000000, 0.7265625000000000000, 0.7343750000000000000 ),
 .UNSPECIFIED. ) 
 CURVE ( )  GEOMETRIC_REPRESENTATION_ITEM ( )  RATIONAL_B_SPLINE_CURVE ( ( 1.000000000000000000, 0.9238795325112867385, 1.000000000000000000, 0.9238795325112867385, 1.000000000000000000, 0.9238795325112867385, 1.000000000000000000, 0.9238795325112867385, 1.000000000000000000 ) ) 
 REPRESENTATION_ITEM ( '' )  );
#18574 = CARTESIAN_POINT ( 'NONE',  ( 161.8273502691896510, -5.000000000000004441, 0.000000000000000000 ) ) ;
#18575 = CARTESIAN_POINT ( 'NONE',  ( -0.08067167272386344123, -15.01514411294037110, 8.017838343683242996 ) ) ;
#18576 = VERTEX_POINT ( 'NONE', #3037 ) ;
#18577 = CARTESIAN_POINT ( 'NONE',  ( 9.874999999999994671, 1.110223024625156540E-13, 2.649519052838167354 ) ) ;
#18578 = CARTESIAN_POINT ( 'NONE',  ( 118.6249999999998010, -1.767766952966431937, -1.767766952966209892 ) ) ;
#18579 = CARTESIAN_POINT ( 'NONE',  ( 0.000000000000000000, 0.000000000000000000, 0.000000000000000000 ) ) ;
#18580 = CARTESIAN_POINT ( 'NONE',  ( 105.2502832217622881, 1.308140751793668288, -1.308140751793640533 ) ) ;
#18581 = CYLINDRICAL_SURFACE ( 'NONE', #17443, 1.000000000000000000 ) ;
#18582 = ORIENTED_EDGE ( 'NONE', *, *, #18332, .F. ) ;
#18583 = CARTESIAN_POINT ( 'NONE',  ( -5.196152422706601826, 2.999999999999975131, -111.9613248654052171 ) ) ;
#18584 = VERTEX_POINT ( 'NONE', #12309 ) ;
#18585 = CARTESIAN_POINT ( 'NONE',  ( 0.000000000000000000, -5.999999999999991118, -75.46132486540524553 ) ) ;
#18586 = CARTESIAN_POINT ( 'NONE',  ( 153.5625000000000568, -4.242640687119298093, 4.242640687119298093 ) ) ;
#18587 = CARTESIAN_POINT ( 'NONE',  ( 4.763139720814407951, -2.749999999999988454, -115.9999999999999858 ) ) ;
#18588 = CARTESIAN_POINT ( 'NONE',  ( 21.06250000000013500, -1.097466725451439196, -2.649519052838419153 ) ) ;
#18589 = CARTESIAN_POINT ( 'NONE',  ( 2.775557561562891351E-14, 6.250000000000033751, -129.4330127018922383 ) ) ;
#18590 = ORIENTED_EDGE ( 'NONE', *, *, #12965, .F. ) ;
#18591 = CARTESIAN_POINT ( 'NONE',  ( -5.999999999999919176, 1.607695154586804565, -56.98066243270260145 ) ) ;
#18592 = CARTESIAN_POINT ( 'NONE',  ( -5.412658773652684552, -3.125000000000099920, -170.0669872981078186 ) ) ;
#18593 = CARTESIAN_POINT ( 'NONE',  ( 2.775557561562891351E-14, 6.250000000000033751, -176.5669872981078186 ) ) ;
#18594 = CARTESIAN_POINT ( 'NONE',  ( 124.9999999999999432, -65.00000000000000000, 7.500000000000007105 ) ) ;
#18595 = EDGE_LOOP ( 'NONE', ( #9234, #7231, #4154, #6048 ) ) ;
#18596 = CARTESIAN_POINT ( 'NONE',  ( 10.62500000000013500, -1.414213562372979016, -1.414213562373090038 ) ) ;
#18597 = SURFACE_SIDE_STYLE ('',( #13861 ) ) ;
#18598 = AXIS2_PLACEMENT_3D ( 'NONE', #9869, #25682, #4633 ) ;
#18599 = LINE ( 'NONE', #27921, #1074 ) ;
#18600 = DIRECTION ( 'NONE',  ( 5.551115123125785167E-17, -1.000000000000000000, -8.881784197001256268E-16 ) ) ;
#18601 = CARTESIAN_POINT ( 'NONE',  ( -4.999999999999984013, -10.50000000000000888, 7.500000000000007105 ) ) ;
#18602 = CARTESIAN_POINT ( 'NONE',  ( 109.5002832217622881, 1.308140751793640533, 1.308140751793640533 ) ) ;
#18603 = CARTESIAN_POINT ( 'NONE',  ( -5.412658773652684552, -3.125000000000099920, -72.56698729810784698 ) ) ;
#18604 = CARTESIAN_POINT ( 'NONE',  ( 5.412658773652739619, 3.124999999999988898, -62.81698729810780435 ) ) ;
#18605 = CARTESIAN_POINT ( 'NONE',  ( 0.000000000000000000, 5.499999999999991118, -46.49999999999998579 ) ) ;
#18606 = DIRECTION ( 'NONE',  ( 0.000000000000000000, 0.000000000000000000, -1.000000000000000000 ) ) ;
#18607 = FACE_OUTER_BOUND ( 'NONE', #5081, .T. ) ;
#18608 = CARTESIAN_POINT ( 'NONE',  ( 159.5177518860653265, -11.09692667050913428, -4.568096268470709376 ) ) ;
#18609 = EDGE_CURVE ( 'NONE', #26967, #23925, #2219, .T. ) ;
#18610 = CARTESIAN_POINT ( 'NONE',  ( 4.763139720814407951, 2.750000000000002665, -123.2500000000000284 ) ) ;
#18611 = CARTESIAN_POINT ( 'NONE',  ( 6.000000000000000888, -3.330669073875464691E-16, -7.560779664488942560E-35 ) ) ;
#18612 = VERTEX_POINT ( 'NONE', #16619 ) ;
#18613 = CARTESIAN_POINT ( 'NONE',  ( 21.56250000000010303, 2.649519052838419153, -1.097466725451559322 ) ) ;
#18614 = CARTESIAN_POINT ( 'NONE',  ( -4.999999999999990230, -24.99999999999999289, 8.000000000000007105 ) ) ;
#18615 = VERTEX_POINT ( 'NONE', #14317 ) ;
#18616 = CARTESIAN_POINT ( 'NONE',  ( 108.5622167782374277, 1.849990392679501827, -0.7662911109077087390 ) ) ;
#18617 = CARTESIAN_POINT ( 'NONE',  ( -19.99999999999998224, -25.00000000000010658, 7.500000000000007105 ) ) ;
#18618 = CARTESIAN_POINT ( 'NONE',  ( -3.608439182435052128, -6.250000000000110134, -111.4419872981078186 ) ) ;
#18619 =( BOUNDED_CURVE ( )  B_SPLINE_CURVE ( 2, ( #6245, #27423, #6389, #29891, #5931, #8872, #22850, #25269, #25124 ),
 .UNSPECIFIED., .F., .F. ) 
 B_SPLINE_CURVE_WITH_KNOTS ( ( 3, 2, 2, 2, 3 ),
 ( 0.2083333333333333426, 0.2092592592592592560, 0.2111111111111111105, 0.2129629629629629650, 0.2138888888888888784 ),
 .UNSPECIFIED. ) 
 CURVE ( )  GEOMETRIC_REPRESENTATION_ITEM ( )  RATIONAL_B_SPLINE_CURVE ( ( 0.9330127018922194093, 0.9330127018922204085, 1.000000000000000000, 0.8660254037844388186, 1.000000000000000000, 0.8660254037844388186, 1.000000000000000000, 0.9330127018922205195, 0.9330127018922196314 ) ) 
 REPRESENTATION_ITEM ( '' )  );
#18620 = FACE_OUTER_BOUND ( 'NONE', #22767, .T. ) ;
#18621 = AXIS2_PLACEMENT_3D ( 'NONE', #28872, #26424, #5673 ) ;
#18622 = DIRECTION ( 'NONE',  ( -1.000000000000000000, -1.665334536937731113E-16, 1.526556658859586792E-16 ) ) ;
#18623 = ORIENTED_EDGE ( 'NONE', *, *, #22363, .T. ) ;
#18624 = ORIENTED_EDGE ( 'NONE', *, *, #18337, .T. ) ;
#18625 = DIRECTION ( 'NONE',  ( -7.147005652999508048E-36, 5.642372883946980038E-36, 1.000000000000000000 ) ) ;
#18626 = CARTESIAN_POINT ( 'NONE',  ( 138.2812500000000284, 2.485281374238585972, 6.000000000000005329 ) ) ;
#18627 = VERTEX_POINT ( 'NONE', #23658 ) ;
#18628 = CARTESIAN_POINT ( 'NONE',  ( 7.216878364870455975, -6.409875621278545621E-14, -140.9419872981078470 ) ) ;
#18629 = CARTESIAN_POINT ( 'NONE',  ( 10.68750000000007283, -1.097466725451499370, 2.649519052838178457 ) ) ;
#18630 = EDGE_CURVE ( 'NONE', #15775, #10765, #27671, .T. ) ;
#18631 = SURFACE_STYLE_USAGE ( .BOTH. , #6473 ) ;
#18632 = CARTESIAN_POINT ( 'NONE',  ( 21.43750000000007105, -1.999999999999911626, 0.8284271247461753029 ) ) ;
#18633 = LINE ( 'NONE', #28111, #20598 ) ;
#18634 = CARTESIAN_POINT ( 'NONE',  ( -3.608439182435115633, 6.249999999999965361, -66.30801270189226670 ) ) ;
#18635 = CARTESIAN_POINT ( 'NONE',  ( 134.4977709871273248, -7.448582144714649189, -8.000000000000007105 ) ) ;
#18636 = CARTESIAN_POINT ( 'NONE',  ( 144.9226497308104342, 5.000000000000004441, 0.000000000000000000 ) ) ;
#18637 = CARTESIAN_POINT ( 'NONE',  ( 111.9761751345947118, -0.8284271247462053900, -1.999999999999731104 ) ) ;
#18638 = FACE_OUTER_BOUND ( 'NONE', #15104, .T. ) ;
#18639 = CARTESIAN_POINT ( 'NONE',  ( 5.196152422706629359, 3.000000000000002665, -165.5386751345948539 ) ) ;
#18640 = CARTESIAN_POINT ( 'NONE',  ( 24.62490920072287892, -2.016120031034378091, 1.292072678355042914 ) ) ;
#18641 = LINE ( 'NONE', #20632, #12617 ) ;
#18642 = CARTESIAN_POINT ( 'NONE',  ( 111.1874999999999858, 1.035533905932749299, 2.500000000000265121 ) ) ;
#18643 = DIRECTION ( 'NONE',  ( 0.000000000000000000, 1.000000000000000000, -0.000000000000000000 ) ) ;
#18644 =( GEOMETRIC_REPRESENTATION_CONTEXT ( 3 ) GLOBAL_UNCERTAINTY_ASSIGNED_CONTEXT ( ( #21351 ) ) GLOBAL_UNIT_ASSIGNED_CONTEXT ( ( #29969, #22626, #1562 ) ) REPRESENTATION_CONTEXT ( 'NONE', 'WORKASPACE' ) );
#18645 = EDGE_CURVE ( 'NONE', #20381, #15417, #6248, .T. ) ;
#18646 = CARTESIAN_POINT ( 'NONE',  ( -4.763139720814407951, -2.750000000000016431, -122.5000000000000568 ) ) ;
#18647 = VECTOR ( 'NONE', #14632, 1000.000000000000000 ) ;
#18648 = CARTESIAN_POINT ( 'NONE',  ( 114.9761751345945697, -0.8284271247461453269, -1.999999999999791278 ) ) ;
#18649 = SURFACE_STYLE_FILL_AREA ( #4928 ) ;
#18650 = CARTESIAN_POINT ( 'NONE',  ( 2.849036369511732440E-14, 20.00000000000001776, -19.00000000000002132 ) ) ;
#18651 = ORIENTED_EDGE ( 'NONE', *, *, #5092, .F. ) ;
#18652 = CARTESIAN_POINT ( 'NONE',  ( -2.775557561562891351E-14, -5.500000000000115463, -53.25000000000002132 ) ) ;
#18653 = CARTESIAN_POINT ( 'NONE',  ( -3.464101615137757051, -5.999999999999979572, -155.0863248654052029 ) ) ;
#18654 = CARTESIAN_POINT ( 'NONE',  ( 0.000000000000000000, 5.999999999999977796, -121.2113248654052029 ) ) ;
#18655 = CARTESIAN_POINT ( 'NONE',  ( 6.000000000000001776, 5.345404176511898156E-15, -178.5863248654052313 ) ) ;
#18656 = ORIENTED_EDGE ( 'NONE', *, *, #8411, .T. ) ;
#18657 = CARTESIAN_POINT ( 'NONE',  ( 105.4999999999999147, -2.499999999999919176, 1.110223024625156540E-13 ) ) ;
#18658 = CARTESIAN_POINT ( 'NONE',  ( 142.2187500000000284, 2.485281374238556218, -6.000000000000005329 ) ) ;
#18659 = CARTESIAN_POINT ( 'NONE',  ( -3.608439182435115633, 6.249999999999965361, -104.4419872981078470 ) ) ;
#18660 = CARTESIAN_POINT ( 'NONE',  ( 142.7886751345948539, 5.500000000000005329, 0.000000000000000000 ) ) ;
#18661 =( BOUNDED_CURVE ( )  B_SPLINE_CURVE ( 2, ( #20593, #24734, #1693, #6604, #3675, #27180, #15565, #8770, #17863 ),
 .UNSPECIFIED., .F., .F. ) 
 B_SPLINE_CURVE_WITH_KNOTS ( ( 3, 2, 2, 2, 3 ),
 ( 0.03055555555555555802, 0.03148148148148144365, 0.03333333333333332593, 0.03518518518518520821, 0.03611111111111109384 ),
 .UNSPECIFIED. ) 
 CURVE ( )  GEOMETRIC_REPRESENTATION_ITEM ( )  RATIONAL_B_SPLINE_CURVE ( ( 0.9330127018922194093, 0.9330127018922194093, 1.000000000000000000, 0.8660254037844388186, 1.000000000000000000, 0.8660254037844388186, 1.000000000000000000, 0.9330127018922234061, 0.9330127018922194093 ) ) 
 REPRESENTATION_ITEM ( '' )  );
#18662 = CARTESIAN_POINT ( 'NONE',  ( 132.3750000000000284, 0.000000000000000000, 6.000000000000005329 ) ) ;
#18663 = DIRECTION ( 'NONE',  ( -7.147005652999508048E-36, 5.642372883946980038E-36, 1.000000000000000000 ) ) ;
#18664 = CARTESIAN_POINT ( 'NONE',  ( 3.175426480543072749, 5.499999999999865885, -136.6250000000000568 ) ) ;
#18665 = ORIENTED_EDGE ( 'NONE', *, *, #14682, .T. ) ;
#18666 = CARTESIAN_POINT ( 'NONE',  ( 11.25000000000001066, 1.110223024625156540E-13, 1.999999999999946265 ) ) ;
#18667 = ORIENTED_EDGE ( 'NONE', *, *, #20481, .F. ) ;
#18668 = STYLED_ITEM ( 'NONE', ( #26477 ), #979 ) ;
#18669 = EDGE_CURVE ( 'NONE', #18250, #23969, #5500, .T. ) ;
#18670 = CARTESIAN_POINT ( 'NONE',  ( 6.350852961086080661, -9.614813431917819062E-14, -61.87500000000000711 ) ) ;
#18671 = CARTESIAN_POINT ( 'NONE',  ( 125.0000000000000568, -55.00000000000000711, 7.500000000000007105 ) ) ;
#18672 = CARTESIAN_POINT ( 'NONE',  ( 6.000000000000026645, -1.607695154586707753, -123.7306624327026014 ) ) ;
#18673 = ORIENTED_EDGE ( 'NONE', *, *, #22963, .T. ) ;
#18674 = CARTESIAN_POINT ( 'NONE',  ( 106.4997167782374845, 1.308140751793640533, -1.308140751793418488 ) ) ;
#18675 = FACE_OUTER_BOUND ( 'NONE', #18886, .T. ) ;
#18676 = CARTESIAN_POINT ( 'NONE',  ( 117.5002832217622455, 1.308140751793696044, 1.308140751793862577 ) ) ;
#18677 = ADVANCED_FACE ( 'NONE', ( #27695 ), #1197, .F. ) ;
#18678 = CARTESIAN_POINT ( 'NONE',  ( -3.175426480542816066, -5.500000000000057732, -150.8749999999999716 ) ) ;
#18679 = CARTESIAN_POINT ( 'NONE',  ( 19.35117513459490013, 2.500000000000084821, 1.035533905932629173 ) ) ;
#18680 = CARTESIAN_POINT ( 'NONE',  ( 3.175426480543072749, -5.500000000000105693, -134.1250000000000284 ) ) ;
#18681 = CARTESIAN_POINT ( 'NONE',  ( -3.608439182435052128, -6.250000000000110134, -161.8080127018922667 ) ) ;
#18682 = DIRECTION ( 'NONE',  ( -7.147005652999508048E-36, 5.642372883946980038E-36, 1.000000000000000000 ) ) ;
#18683 = CARTESIAN_POINT ( 'NONE',  ( -2.775557561562891351E-14, -5.500000000000115463, -81.74999999999998579 ) ) ;
#18684 = CARTESIAN_POINT ( 'NONE',  ( 6.000000000000026645, -1.607695154586707753, -140.2306624327026157 ) ) ;
#18685 = CARTESIAN_POINT ( 'NONE',  ( 140.5000000000000284, 0.000000000000000000, 0.000000000000000000 ) ) ;
#18686 = CARTESIAN_POINT ( 'NONE',  ( 0.000000000000000000, 5.499999999999991118, -63.00000000000000000 ) ) ;
#18687 = DIRECTION ( 'NONE',  ( -7.147005652999508048E-36, 5.642372883946980038E-36, 1.000000000000000000 ) ) ;
#18688 = CARTESIAN_POINT ( 'NONE',  ( 0.000000000000000000, -5.999999999999991118, -114.4613248654052171 ) ) ;
#18689 = LINE ( 'NONE', #13483, #11594 ) ;
#18690 = CARTESIAN_POINT ( 'NONE',  ( 159.1875000000000284, 4.242640687119269671, 4.242640687119298093 ) ) ;
#18691 = CARTESIAN_POINT ( 'NONE',  ( 19.62500000000008527, -1.414213562372979016, -1.414213562373145550 ) ) ;
#18692 = VECTOR ( 'NONE', #23212, 1000.000000000000000 ) ;
#18693 = CARTESIAN_POINT ( 'NONE',  ( 138.9449251345948824, -5.500000000000012434, 2.278174593052012309 ) ) ;
#18694 = CARTESIAN_POINT ( 'NONE',  ( 119.8511751345945981, -1.999999999999941602, -0.8284271247460553989 ) ) ;
#18695 = CARTESIAN_POINT ( 'NONE',  ( 119.4372167782374419, 0.7662911109078888172, -1.849990392679291551 ) ) ;
#18696 = CARTESIAN_POINT ( 'NONE',  ( 5.196152422706629359, -2.999999999999988898, -97.71132486540523132 ) ) ;
#18697 = VERTEX_POINT ( 'NONE', #20092 ) ;
#18698 = CARTESIAN_POINT ( 'NONE',  ( 149.7187500000000568, 2.485281374238555774, -6.000000000000005329 ) ) ;
#18699 = CARTESIAN_POINT ( 'NONE',  ( 6.000000000000000888, 1.743066579297358182E-13, -108.6636751345948255 ) ) ;
#18700 = CARTESIAN_POINT ( 'NONE',  ( 114.1877832217620892, 0.7662911109078588412, -1.849990392679291551 ) ) ;
#18701 = CARTESIAN_POINT ( 'NONE',  ( 0.000000000000000000, 0.000000000000000000, 0.000000000000000000 ) ) ;
#18702 = VERTEX_POINT ( 'NONE', #13787 ) ;
#18703 = VERTEX_POINT ( 'NONE', #26817 ) ;
#18704 = VERTEX_POINT ( 'NONE', #13219 ) ;
#18705 = EDGE_CURVE ( 'NONE', #13073, #26551, #12908, .T. ) ;
#18706 = CARTESIAN_POINT ( 'NONE',  ( -4.763139720814407951, -2.750000000000016431, -89.50000000000002842 ) ) ;
#18707 = AXIS2_PLACEMENT_3D ( 'NONE', #6135, #26848, #3509 ) ;
#18708 = CARTESIAN_POINT ( 'NONE',  ( 5.412658773652739619, 3.124999999999988898, -110.1830127018922383 ) ) ;
#18709 = VERTEX_POINT ( 'NONE', #8407 ) ;
#18710 = PRESENTATION_STYLE_ASSIGNMENT (( #17120 ) ) ;
#18711 = CARTESIAN_POINT ( 'NONE',  ( 158.8913997308104058, -2.071067811865468400, 4.999999999999989342 ) ) ;
#18712 = CARTESIAN_POINT ( 'NONE',  ( -3.608439182435052128, -6.250000000000110134, -47.80801270189223828 ) ) ;
#18713 = ORIENTED_EDGE ( 'NONE', *, *, #3096, .F. ) ;
#18714 = ADVANCED_FACE ( 'NONE', ( #15363 ), #12755, .T. ) ;
#18715 = EDGE_CURVE ( 'NONE', #3655, #10447, #17306, .T. ) ;
#18716 = VECTOR ( 'NONE', #30262, 1000.000000000000000 ) ;
#18717 = CARTESIAN_POINT ( 'NONE',  ( -4.763139720814407951, -2.750000000000016431, -173.5000000000000000 ) ) ;
#18718 = DIRECTION ( 'NONE',  ( -1.000000000000000000, -1.665334536937736783E-16, -2.220446049250315546E-16 ) ) ;
#18719 = CARTESIAN_POINT ( 'NONE',  ( -3.175426480542816510, 5.499999999999865885, -158.8750000000000000 ) ) ;
#18720 = CARTESIAN_POINT ( 'NONE',  ( 111.9999999999999716, 2.500000000000002220, 0.000000000000000000 ) ) ;
#18721 = CARTESIAN_POINT ( 'NONE',  ( 3.175426480543072749, -5.500000000000105693, -104.1250000000000142 ) ) ;
#18722 = LINE ( 'NONE', #23013, #37 ) ;
#18723 = CARTESIAN_POINT ( 'NONE',  ( 3.175426480543072749, -5.500000000000105693, -96.62500000000004263 ) ) ;
#18724 = CARTESIAN_POINT ( 'NONE',  ( 115.2886751345946550, 2.000000000000112799, 3.330669073875469621E-13 ) ) ;
#18725 = PRESENTATION_STYLE_ASSIGNMENT (( #23329 ) ) ;
#18726 = CARTESIAN_POINT ( 'NONE',  ( 0.1878980370099003760, -15.40048167581654681, 8.313448362010671389 ) ) ;
#18727 = VERTEX_POINT ( 'NONE', #16393 ) ;
#18728 = CARTESIAN_POINT ( 'NONE',  ( 11.56250000000000000, 2.649519052838298805, -1.097466725451559322 ) ) ;
#18729 = CARTESIAN_POINT ( 'NONE',  ( 114.8749999999998295, 1.767766952966320915, -1.767766952966209892 ) ) ;
#18730 = CARTESIAN_POINT ( 'NONE',  ( 3.464101615137757051, -5.999999999999979572, -161.4136751345947971 ) ) ;
#18731 = CIRCLE ( 'NONE', #5430, 5.999999999999992006 ) ;
#18732 = CARTESIAN_POINT ( 'NONE',  ( 106.6252832217623023, 2.775557561562891351E-14, 1.849990392679634610 ) ) ;
#18733 = CARTESIAN_POINT ( 'NONE',  ( 161.0614794248616590, 1.551837106343485706, 5.349811464556154306 ) ) ;
#18734 = ORIENTED_EDGE ( 'NONE', *, *, #25503, .F. ) ;
#18735 = CARTESIAN_POINT ( 'NONE',  ( 113.8511751345944987, -1.999999999999881650, -0.8284271247459952248 ) ) ;
#18736 = DIRECTION ( 'NONE',  ( 1.000000000000000000, 0.000000000000000000, 0.000000000000000000 ) ) ;
#18737 = VECTOR ( 'NONE', #19042, 1000.000000000000000 ) ;
#18738 = CARTESIAN_POINT ( 'NONE',  ( 106.1872167782374703, -1.849990392679381701, -0.7662911109075283278 ) ) ;
#18739 = EDGE_LOOP ( 'NONE', ( #17708, #15999, #120, #16849 ) ) ;
#18740 = DIRECTION ( 'NONE',  ( 0.000000000000000000, 0.000000000000000000, 1.000000000000000000 ) ) ;
#18741 = MECHANICAL_DESIGN_GEOMETRIC_PRESENTATION_REPRESENTATION (  '', ( #28011 ), #9404 ) ;
#18742 = EDGE_LOOP ( 'NONE', ( #535, #527, #3028, #20450 ) ) ;
#18743 = CARTESIAN_POINT ( 'NONE',  ( 148.9687500000000284, -2.485281374238585972, 6.000000000000005329 ) ) ;
#18744 = EDGE_CURVE ( 'NONE', #28218, #6311, #17072, .T. ) ;
#18745 = CARTESIAN_POINT ( 'NONE',  ( 3.175426480543072749, -5.500000000000105693, -114.6250000000000000 ) ) ;
#18746 = CARTESIAN_POINT ( 'NONE',  ( 22.81250000000005329, -2.649519052838178457, 1.097466725451559322 ) ) ;
#18747 = EDGE_CURVE ( 'NONE', #25740, #25500, #18301, .T. ) ;
#18748 = CARTESIAN_POINT ( 'NONE',  ( 2.775557561562891351E-14, -6.250000000000061284, -134.6830127018922667 ) ) ;
#18749 = EDGE_LOOP ( 'NONE', ( #21839, #27411, #13042, #2470 ) ) ;
#18750 = CARTESIAN_POINT ( 'NONE',  ( 5.412658773652739619, 3.124999999999988898, -172.3169872981078470 ) ) ;
#18751 = CARTESIAN_POINT ( 'NONE',  ( 110.0624999999998295, 2.499999999999994671, 1.035533905932809473 ) ) ;
#18752 = VECTOR ( 'NONE', #1071, 1000.000000000000000 ) ;
#18753 =( BOUNDED_CURVE ( )  B_SPLINE_CURVE ( 3, ( #16462, #731, #26083, #14590 ),
 .UNSPECIFIED., .F., .T. ) 
 B_SPLINE_CURVE_WITH_KNOTS ( ( 4, 4 ),
 ( 4.712388980384689674, 6.283185307179586232 ),
 .UNSPECIFIED. ) 
 CURVE ( )  GEOMETRIC_REPRESENTATION_ITEM ( )  RATIONAL_B_SPLINE_CURVE ( ( 1.000000000000000000, 0.8047378541243649375, 0.8047378541243649375, 1.000000000000000000 ) ) 
 REPRESENTATION_ITEM ( '' )  );
#18754 = CARTESIAN_POINT ( 'NONE',  ( 109.3511751345945981, 2.000000000000091926, 0.8284271247462955401 ) ) ;
#18755 = CARTESIAN_POINT ( 'NONE',  ( -0.5000000000000004441, -9.500000000000008882, 8.000000000000007105 ) ) ;
#18756 = CARTESIAN_POINT ( 'NONE',  ( -4.763139720814407951, -2.750000000000016431, -181.0000000000000568 ) ) ;
#18757 = CARTESIAN_POINT ( 'NONE',  ( 107.0002832217622597, -1.308140751793585022, -1.308140751793640533 ) ) ;
#18758 = CARTESIAN_POINT ( 'NONE',  ( 5.196152422706629359, 3.000000000000002665, -110.9613248654052171 ) ) ;
#18759 = CARTESIAN_POINT ( 'NONE',  ( 3.608439182435180470, -6.249999999999997335, -178.0580127018922383 ) ) ;
#18760 = CARTESIAN_POINT ( 'NONE',  ( 5.999999999999949374, 1.607695154586804565, -103.5193375672974412 ) ) ;
#18761 = DIRECTION ( 'NONE',  ( -0.000000000000000000, 1.000000000000000000, 0.000000000000000000 ) ) ;
#18762 = CARTESIAN_POINT ( 'NONE',  ( 136.0000000000000284, -9.165151389911669000, 8.000000000000007105 ) ) ;
#18763 = CARTESIAN_POINT ( 'NONE',  ( -6.350852961085760029, -1.281975124255709124E-13, -124.1250000000000568 ) ) ;
#18765 = AXIS2_PLACEMENT_3D ( 'NONE', #18387, #4370, #73 ) ;
#18764 = CARTESIAN_POINT ( 'NONE',  ( 134.9999999911586883, -7.162772570454863263, -8.424744567432407294 ) ) ;
#18766 = ORIENTED_EDGE ( 'NONE', *, *, #23074, .T. ) ;
#18767 = CARTESIAN_POINT ( 'NONE',  ( 22.68750000000008882, 2.649519052838538613, 1.097466725451499370 ) ) ;
#18768 = AXIS2_PLACEMENT_3D ( 'NONE', #11630, #8986, #27850 ) ;
#18769 = CARTESIAN_POINT ( 'NONE',  ( 6.000000000000000888, -1.859271017917181981E-14, -159.6636751345948539 ) ) ;
#18770 = CARTESIAN_POINT ( 'NONE',  ( 135.0000000000000284, 0.000000000000000000, -5.500000000000000000 ) ) ;
#18771 = CARTESIAN_POINT ( 'NONE',  ( 116.4761751345946124, 0.8284271247462955401, 2.000000000000271783 ) ) ;
#18772 = ORIENTED_EDGE ( 'NONE', *, *, #13583, .T. ) ;
#18773 = VECTOR ( 'NONE', #10095, 1000.000000000000000 ) ;
#18774 = CARTESIAN_POINT ( 'NONE',  ( 108.3122167782374135, -0.7662911109077388261, -1.849990392679351725 ) ) ;
#18775 = CARTESIAN_POINT ( 'NONE',  ( 6.000000000000000888, -3.330669073875464691E-16, -7.560779664488942560E-35 ) ) ;
#18776 = CARTESIAN_POINT ( 'NONE',  ( -5.412658773652684552, -3.125000000000099920, -108.5669872981078186 ) ) ;
#18777 = CARTESIAN_POINT ( 'NONE',  ( 22.02382486540538764, -1.035533905932629173, 2.499999999999904521 ) ) ;
#18778 = CARTESIAN_POINT ( 'NONE',  ( 113.2738248654050182, -1.999999999999941602, -0.8284271247459952248 ) ) ;
#18779 = ORIENTED_EDGE ( 'NONE', *, *, #13916, .F. ) ;
#18780 = EDGE_LOOP ( 'NONE', ( #5119, #16300, #22115, #19187 ) ) ;
#18781 = CARTESIAN_POINT ( 'NONE',  ( 0.000000000000000000, -5.999999999999991118, -142.0386751345948255 ) ) ;
#18782 = CARTESIAN_POINT ( 'NONE',  ( 137.9062500000000568, 6.000000000000005329, -2.485281374238555774 ) ) ;
#18783 = EDGE_CURVE ( 'NONE', #8182, #7800, #4522, .T. ) ;
#18784 = ADVANCED_FACE ( 'NONE', ( #11482 ), #12035, .F. ) ;
#18785 = CARTESIAN_POINT ( 'NONE',  ( 5.412658773652712085, -3.125000000000086153, -138.0669872981078470 ) ) ;
#18786 = CYLINDRICAL_SURFACE ( 'NONE', #25026, 5.500000000000000000 ) ;
#18787 = DIRECTION ( 'NONE',  ( -7.147005652999508048E-36, 5.642372883946980038E-36, 1.000000000000000000 ) ) ;
#18788 = CARTESIAN_POINT ( 'NONE',  ( 6.000000000000000888, 1.743066579297358182E-13, -51.08632486540523132 ) ) ;
#18789 = CARTESIAN_POINT ( 'NONE',  ( 17.93750000000012434, 2.000000000000091926, -0.8284271247463557142 ) ) ;
#18790 = CARTESIAN_POINT ( 'NONE',  ( 1.000000000000000888, -14.99923475244192339, 9.015151515151522688 ) ) ;
#18791 = CARTESIAN_POINT ( 'NONE',  ( 5.412658773652739619, 3.124999999999988898, -59.18301270189224539 ) ) ;
#18792 = CARTESIAN_POINT ( 'NONE',  ( 143.0476497308104058, 0.000000000000000000, -5.000000000000004441 ) ) ;
#18793 = CARTESIAN_POINT ( 'NONE',  ( -3.464101615137757051, -5.999999999999979572, -125.0863248654052029 ) ) ;
#18794 = CARTESIAN_POINT ( 'NONE',  ( 6.000000000000000888, -1.607695154586752384, -160.6533121635129930 ) ) ;
#18795 = LINE ( 'NONE', #8953, #25654 ) ;
#18796 = CARTESIAN_POINT ( 'NONE',  ( 108.8363248654051034, 1.414213562373090038, 1.414213562373034527 ) ) ;
#18797 = CARTESIAN_POINT ( 'NONE',  ( 111.9374999999998010, 2.500000000000115019, -1.035533905932508825 ) ) ;
#18798 = FILL_AREA_STYLE_COLOUR ( '', #23505 ) ;
#18799 = DIRECTION ( 'NONE',  ( -1.000000000000000000, -6.938893903907221278E-15, 0.000000000000000000 ) ) ;
#18800 = ORIENTED_EDGE ( 'NONE', *, *, #20218, .F. ) ;
#18801 =( BOUNDED_CURVE ( )  B_SPLINE_CURVE ( 2, ( #5371, #19388, #2922, #14779, #25980, #7684, #17093, #9561, #23694 ),
 .UNSPECIFIED., .F., .F. ) 
 B_SPLINE_CURVE_WITH_KNOTS ( ( 3, 2, 2, 2, 3 ),
 ( 0.1694444444444443976, 0.1703703703703703942, 0.1722222222222222765, 0.1740740740740740478, 0.1750000000000000444 ),
 .UNSPECIFIED. ) 
 CURVE ( )  GEOMETRIC_REPRESENTATION_ITEM ( )  RATIONAL_B_SPLINE_CURVE ( ( 0.9330127018922194093, 0.9330127018922154125, 1.000000000000000000, 0.8660254037844388186, 1.000000000000000000, 0.8660254037844388186, 1.000000000000000000, 0.9330127018922154125, 0.9330127018922194093 ) ) 
 REPRESENTATION_ITEM ( '' )  );
#18802 = CARTESIAN_POINT ( 'NONE',  ( 4.763139720814407951, -2.749999999999988454, -54.49999999999999289 ) ) ;
#18803 = CARTESIAN_POINT ( 'NONE',  ( -5.196152422706573404, -3.000000000000002665, -155.2113248654052313 ) ) ;
#18804 = FACE_OUTER_BOUND ( 'NONE', #18595, .T. ) ;
#18805 = AXIS2_PLACEMENT_3D ( 'NONE', #20700, #11038, #18259 ) ;
#18806 = CARTESIAN_POINT ( 'NONE',  ( -5.999999999999962697, 3.323446944526963260E-14, -152.3363248654052313 ) ) ;
#18807 = ORIENTED_EDGE ( 'NONE', *, *, #7772, .F. ) ;
#18808 = CARTESIAN_POINT ( 'NONE',  ( 106.2499999999999716, -2.775557561562891351E-14, 2.499999999999946709 ) ) ;
#18809 = CARTESIAN_POINT ( 'NONE',  ( 141.0937500000000284, 6.000000000000005329, 2.485281374238585972 ) ) ;
#18810 = CARTESIAN_POINT ( 'NONE',  ( 5.412658773652739619, 3.124999999999988898, -106.3169872981078470 ) ) ;
#18811 = CARTESIAN_POINT ( 'NONE',  ( 3.464101615137852974, 5.999999999999884537, -176.8363248654051176 ) ) ;
#18812 = CARTESIAN_POINT ( 'NONE',  ( 159.7351497308104058, 3.535533905932725318, -3.535533905932725318 ) ) ;
#18813 = CARTESIAN_POINT ( 'NONE',  ( 6.350852961086080661, -9.614813431917819062E-14, -133.8750000000000284 ) ) ;
#18814 = ADVANCED_FACE ( 'NONE', ( #2232 ), #11633, .T. ) ;
#18815 = AXIS2_PLACEMENT_3D ( 'NONE', #5516, #27170, #17853 ) ;
#18816 = ORIENTED_EDGE ( 'NONE', *, *, #22117, .F. ) ;
#18817 = CARTESIAN_POINT ( 'NONE',  ( 135.0000000000000284, 0.000000000000000000, -11.00000000000000355 ) ) ;
#18818 = CARTESIAN_POINT ( 'NONE',  ( -4.763139720814407951, -2.750000000000016431, -65.50000000000000000 ) ) ;
#18819 = CARTESIAN_POINT ( 'NONE',  ( -6.000000000000007105, -1.607695154586655129, -81.76933756729744118 ) ) ;
#18820 = CARTESIAN_POINT ( 'NONE',  ( 108.9136751345947260, -1.414213562373228816, -1.414213562373034527 ) ) ;
#18821 = CARTESIAN_POINT ( 'NONE',  ( 2.775557561562891351E-14, -6.250000000000061284, -86.68301270189226670 ) ) ;
#18822 = CARTESIAN_POINT ( 'NONE',  ( -5.196152422706573404, -3.000000000000002665, -101.2113248654052455 ) ) ;
#18823 = CARTESIAN_POINT ( 'NONE',  ( 119.9613248654051034, 1.110223024625156540E-13, 2.000000000000001776 ) ) ;
#18824 = CARTESIAN_POINT ( 'NONE',  ( 105.9997167782375982, -1.308140751793612777, 1.308140751793640533 ) ) ;
#18825 = DIRECTION ( 'NONE',  ( 6.938893903907221278E-15, -1.000000000000000000, 0.000000000000000000 ) ) ;
#18826 = CARTESIAN_POINT ( 'NONE',  ( 120.8127832217621318, -1.849990392679411677, 0.7662911109079489913 ) ) ;
#18827 = CARTESIAN_POINT ( 'NONE',  ( -2.775557561562891351E-14, -5.500000000000115463, -147.7500000000000568 ) ) ;
#18828 = CARTESIAN_POINT ( 'NONE',  ( 140.0000000000000000, -10.00000000000000888, 7.500000000000000888 ) ) ;
#18829 = CARTESIAN_POINT ( 'NONE',  ( -7.216878364870328078, 0.000000000000000000, -162.0580127018922099 ) ) ;
#18830 =( LENGTH_UNIT ( ) NAMED_UNIT ( * ) SI_UNIT ( .MILLI., .METRE. ) );
#18831 = CARTESIAN_POINT ( 'NONE',  ( 116.2886751345946124, 2.000000000000168310, 3.330669073875469621E-13 ) ) ;
#18832 = CARTESIAN_POINT ( 'NONE',  ( -2.775557561562891351E-14, -5.500000000000115463, -80.25000000000004263 ) ) ;
#18833 = DIRECTION ( 'NONE',  ( -1.000000000000000000, 0.000000000000000000, 0.000000000000000000 ) ) ;
#18834 = CARTESIAN_POINT ( 'NONE',  ( 4.763139720814407951, 2.750000000000002665, -67.75000000000002842 ) ) ;
#18835 =( BOUNDED_CURVE ( )  B_SPLINE_CURVE ( 2, ( #23668, #2604, #17470, #5749, #12023, #18923, #156, #21360, #21517 ),
 .UNSPECIFIED., .F., .T. ) 
 B_SPLINE_CURVE_WITH_KNOTS ( ( 3, 2, 2, 2, 3 ),
 ( 0.6305555555555555358, 0.6314814814814815325, 0.6333333333333333037, 0.6351851851851851860, 0.6361111111111110716 ),
 .UNSPECIFIED. ) 
 CURVE ( )  GEOMETRIC_REPRESENTATION_ITEM ( )  RATIONAL_B_SPLINE_CURVE ( ( 0.9330127018922194093, 0.9330127018922154125, 1.000000000000000000, 0.8660254037844388186, 1.000000000000000000, 0.8660254037844388186, 1.000000000000000000, 0.9330127018922234061, 0.9330127018922194093 ) ) 
 REPRESENTATION_ITEM ( '' )  );
#18836 = AXIS2_PLACEMENT_3D ( 'NONE', #26578, #12646, #15088 ) ;
#18837 = CARTESIAN_POINT ( 'NONE',  ( -5.196152422706573404, -3.000000000000002665, -156.7113248654052313 ) ) ;
#18838 = DIRECTION ( 'NONE',  ( -0.000000000000000000, -0.000000000000000000, -1.000000000000000000 ) ) ;
#18839 =( GEOMETRIC_REPRESENTATION_CONTEXT ( 3 ) GLOBAL_UNCERTAINTY_ASSIGNED_CONTEXT ( ( #9661 ) ) GLOBAL_UNIT_ASSIGNED_CONTEXT ( ( #29131, #8091, #24232 ) ) REPRESENTATION_CONTEXT ( 'NONE', 'WORKASPACE' ) );
#18840 = CARTESIAN_POINT ( 'NONE',  ( 159.7500000000000284, -6.000000000000005329, 0.000000000000000000 ) ) ;
#18841 = DIRECTION ( 'NONE',  ( 0.000000000000000000, 0.000000000000000000, -1.000000000000000000 ) ) ;
#18842 = CARTESIAN_POINT ( 'NONE',  ( 16.68750000000013856, -0.8284271247461753029, -2.000000000000151879 ) ) ;
#18843 = EDGE_CURVE ( 'NONE', #20404, #2534, #28477, .T. ) ;
#18844 = CARTESIAN_POINT ( 'NONE',  ( -5.999999999999963585, -1.487416814333745711E-14, -50.33632486540523843 ) ) ;
#18845 = CARTESIAN_POINT ( 'NONE',  ( 0.000000000000000000, -5.999999999999991118, -147.4613248654052029 ) ) ;
#18846 = CARTESIAN_POINT ( 'NONE',  ( 117.9997167782376266, -1.308140751793696044, 1.308140751793751555 ) ) ;
#18847 = DIRECTION ( 'NONE',  ( 1.000000000000000000, -5.551115123125773458E-17, -1.260129944081490338E-35 ) ) ;
#18848 = ORIENTED_EDGE ( 'NONE', *, *, #18961, .T. ) ;
#18849 = CARTESIAN_POINT ( 'NONE',  ( 149.0625000000000284, -4.242640687119298093, 4.242640687119298093 ) ) ;
#18850 = DIRECTION ( 'NONE',  ( -1.000000000000000000, -1.665334536937731113E-16, -8.326672684688674053E-17 ) ) ;
#18851 = CARTESIAN_POINT ( 'NONE',  ( 114.5002832217623023, 1.308140751793696044, 1.308140751793640533 ) ) ;
#18852 = CARTESIAN_POINT ( 'NONE',  ( -4.763139720814407951, -2.750000000000016431, -154.0000000000000284 ) ) ;
#18853 = LINE ( 'NONE', #12102, #9209 ) ;
#18854 = ORIENTED_EDGE ( 'NONE', *, *, #29631, .T. ) ;
#18855 = ORIENTED_EDGE ( 'NONE', *, *, #20409, .F. ) ;
#18856 = CARTESIAN_POINT ( 'NONE',  ( 21.37500000000011724, -1.414213562373090038, 1.414213562373034527 ) ) ;
#18857 = EDGE_LOOP ( 'NONE', ( #20918, #18177, #27032, #5868 ) ) ;
#18858 = CARTESIAN_POINT ( 'NONE',  ( 4.763139720814407951, -2.749999999999988454, -90.50000000000002842 ) ) ;
#18859 = ORIENTED_EDGE ( 'NONE', *, *, #14546, .T. ) ;
#18860 = CARTESIAN_POINT ( 'NONE',  ( 1.000434615788146742, 10.95616177385588941, -19.08065934301228594 ) ) ;
#18861 = AXIS2_PLACEMENT_3D ( 'NONE', #9107, #8964, #28 ) ;
#18862 = CARTESIAN_POINT ( 'NONE',  ( 154.2976497308104342, 0.000000000000000000, 5.000000000000004441 ) ) ;
#18863 = CARTESIAN_POINT ( 'NONE',  ( 4.763139720814407951, -2.749999999999988454, -164.0000000000000284 ) ) ;
#18864 = CARTESIAN_POINT ( 'NONE',  ( -3.464101615137757051, -5.999999999999979572, -63.58632486540521711 ) ) ;
#18865 = DIRECTION ( 'NONE',  ( -7.147005652999508048E-36, 5.642372883946980038E-36, 1.000000000000000000 ) ) ;
#18866 = CARTESIAN_POINT ( 'NONE',  ( 4.763139720814407951, -2.749999999999988454, -176.0000000000000568 ) ) ;
#18867 = CARTESIAN_POINT ( 'NONE',  ( 147.2738248654052313, -3.889087296526011706, 3.889087296526011706 ) ) ;
#18868 = CARTESIAN_POINT ( 'NONE',  ( -2.775557561562891351E-14, -5.500000000000115463, -156.7500000000000568 ) ) ;
#18869 = CARTESIAN_POINT ( 'NONE',  ( 113.9374999999997300, 2.500000000000114575, -1.035533905932629173 ) ) ;
#18870 = CARTESIAN_POINT ( 'NONE',  ( 4.763139720814407951, 2.750000000000002665, -100.7500000000000000 ) ) ;
#18871 = CARTESIAN_POINT ( 'NONE',  ( 6.000000000000000888, -1.859271017917181981E-14, -159.0863248654052313 ) ) ;
#18872 = DIRECTION ( 'NONE',  ( -1.000000000000000000, -1.665334536937736783E-16, -2.220446049250315546E-16 ) ) ;
#18874 = CARTESIAN_POINT ( 'NONE',  ( 0.000000000000000000, 5.499999999999991118, -90.00000000000002842 ) ) ;
#18873 = CARTESIAN_POINT ( 'NONE',  ( -3.175426480542816510, -5.500000000000057732, -155.3750000000000000 ) ) ;
#18875 = CARTESIAN_POINT ( 'NONE',  ( 24.48000116661930292, 0.3094390903118284797, -2.499999999999972911 ) ) ;
#18876 = CARTESIAN_POINT ( 'NONE',  ( 161.6398502691896510, -3.535533905932752852, 3.535533905932725318 ) ) ;
#18877 = CARTESIAN_POINT ( 'NONE',  ( 135.0000000000000284, -7.635558407351254573, 8.089926835396470395 ) ) ;
#18878 = ORIENTED_EDGE ( 'NONE', *, *, #29228, .F. ) ;
#18879 = CARTESIAN_POINT ( 'NONE',  ( 24.25000000000018829, 1.110223024625156540E-13, 2.000000000000001776 ) ) ;
#18880 = UNCERTAINTY_MEASURE_WITH_UNIT (LENGTH_MEASURE( 1.000000000000000082E-05 ), #2670, 'distance_accuracy_value', 'NONE');
#18881 = CARTESIAN_POINT ( 'NONE',  ( 113.8124999999998437, 1.035533905932749299, -2.499999999999904521 ) ) ;
#18882 = EDGE_CURVE ( 'NONE', #17680, #9948, #22401, .T. ) ;
#18883 = CARTESIAN_POINT ( 'NONE',  ( 6.000000000000000888, -1.859271017917181981E-14, -168.6636751345947971 ) ) ;
#18884 = CARTESIAN_POINT ( 'NONE',  ( 107.2502832217623450, 1.308140751793640533, -1.308140751793640533 ) ) ;
#18885 = LINE ( 'NONE', #25916, #4169 ) ;
#18886 = EDGE_LOOP ( 'NONE', ( #25625, #619, #25064 ) ) ;
#18887 = FACE_OUTER_BOUND ( 'NONE', #27627, .T. ) ;
#18888 = DIRECTION ( 'NONE',  ( -1.000000000000000000, -1.665334536937731113E-16, 1.526556658859586792E-16 ) ) ;
#18889 = CARTESIAN_POINT ( 'NONE',  ( 106.8122167782374277, 0.7662911109079189043, 1.849990392679712103 ) ) ;
#18890 = CARTESIAN_POINT ( 'NONE',  ( 111.1488248654049329, -1.999999999999941602, 0.8284271247462955401 ) ) ;
#18891 = VECTOR ( 'NONE', #26987, 1000.000000000000000 ) ;
#18892 = EDGE_LOOP ( 'NONE', ( #3734, #7073, #20563, #21671 ) ) ;
#18893 = EDGE_CURVE ( 'NONE', #16955, #20809, #26605, .T. ) ;
#18894 = CARTESIAN_POINT ( 'NONE',  ( 3.464101615137757051, -5.999999999999979572, -52.83632486540517448 ) ) ;
#18895 = EDGE_CURVE ( 'NONE', #3013, #20406, #6697, .T. ) ;
#18896 = VERTEX_POINT ( 'NONE', #15118 ) ;
#18897 = CARTESIAN_POINT ( 'NONE',  ( 150.6562500000000284, -6.000000000000005329, 2.485281374238555774 ) ) ;
#18898 = EDGE_LOOP ( 'NONE', ( #26555, #22291, #17482, #2008 ) ) ;
#18899 = CARTESIAN_POINT ( 'NONE',  ( 6.350852961086080661, -9.614813431917819062E-14, -109.8750000000000426 ) ) ;
#18900 = CARTESIAN_POINT ( 'NONE',  ( 23.56250000000009948, 1.097466725451679892, 2.649519052838298805 ) ) ;
#18901 = CARTESIAN_POINT ( 'NONE',  ( -2.775557561562891351E-14, -5.500000000000115463, -150.7500000000000568 ) ) ;
#18902 = CARTESIAN_POINT ( 'NONE',  ( -5.412658773652739619, 3.124999999999975131, -130.6830127018922667 ) ) ;
#18903 = ORIENTED_EDGE ( 'NONE', *, *, #11013, .T. ) ;
#18904 = DIRECTION ( 'NONE',  ( 1.000000000000000000, 0.000000000000000000, 0.000000000000000000 ) ) ;
#18905 = CARTESIAN_POINT ( 'NONE',  ( -7.216878364870328078, 0.000000000000000000, -171.6919872981078186 ) ) ;
#18906 = CARTESIAN_POINT ( 'NONE',  ( 106.6874999999998010, -1.035533905932689347, -2.499999999999784173 ) ) ;
#18907 = DIRECTION ( 'NONE',  ( -1.000000000000000000, -1.665334536937731113E-16, 1.526556658859586792E-16 ) ) ;
#18908 = VERTEX_POINT ( 'NONE', #17283 ) ;
#18909 = LINE ( 'NONE', #27614, #20721 ) ;
#18910 = CARTESIAN_POINT ( 'NONE',  ( 135.5000000000000000, -24.99999999999999289, 7.500000000000007105 ) ) ;
#18911 = CARTESIAN_POINT ( 'NONE',  ( -6.350852961085760029, -1.281975124255709124E-13, -179.6250000000000284 ) ) ;
#18912 = CARTESIAN_POINT ( 'NONE',  ( 106.2502832217621460, 1.308140751793696044, -1.308140751793640533 ) ) ;
#18913 = CARTESIAN_POINT ( 'NONE',  ( -3.608439182435115633, 6.249999999999965361, -175.8080127018922667 ) ) ;
#18914 = CARTESIAN_POINT ( 'NONE',  ( 6.000000000000052403, -1.607695154586662678, -48.15331216351300725 ) ) ;
#18915 = CARTESIAN_POINT ( 'NONE',  ( -5.196152422706573404, -3.000000000000002665, -53.78867513459483973 ) ) ;
#18916 = UNCERTAINTY_MEASURE_WITH_UNIT (LENGTH_MEASURE( 1.000000000000000082E-05 ), #19637, 'distance_accuracy_value', 'NONE');
#18917 = CARTESIAN_POINT ( 'NONE',  ( 6.350852961086080661, -9.614813431917819062E-14, -111.3750000000000568 ) ) ;
#18918 = CARTESIAN_POINT ( 'NONE',  ( 135.2061204155054099, -8.336295798213267716, -8.142448489966165326 ) ) ;
#18919 = ORIENTED_EDGE ( 'NONE', *, *, #9514, .F. ) ;
#18920 = CARTESIAN_POINT ( 'NONE',  ( 22.81250000000002132, 1.097466725451559322, 2.649519052838298805 ) ) ;
#18921 = EDGE_CURVE ( 'NONE', #17836, #27181, #20423, .T. ) ;
#18922 = FACE_OUTER_BOUND ( 'NONE', #24182, .T. ) ;
#18923 = CARTESIAN_POINT ( 'NONE',  ( 3.464101615137852974, 5.999999999999884537, -131.8363248654052313 ) ) ;
#18924 = ORIENTED_EDGE ( 'NONE', *, *, #26226, .F. ) ;
#18925 = AXIS2_PLACEMENT_3D ( 'NONE', #18227, #13947, #20826 ) ;
#18926 = DIRECTION ( 'NONE',  ( 0.000000000000000000, 0.000000000000000000, -1.000000000000000000 ) ) ;
#18927 = CARTESIAN_POINT ( 'NONE',  ( 118.5863248654051461, 1.414213562373117794, -1.414213562373034527 ) ) ;
#18928 = CARTESIAN_POINT ( 'NONE',  ( 110.4372167782375840, 0.7662911109078888172, -1.849990392679231599 ) ) ;
#18929 = AXIS2_PLACEMENT_3D ( 'NONE', #22982, #1920, #20830 ) ;
#18930 = CARTESIAN_POINT ( 'NONE',  ( 0.000000000000000000, 0.000000000000000000, 0.000000000000000000 ) ) ;
#18931 = VERTEX_POINT ( 'NONE', #29057 ) ;
#18932 = EDGE_CURVE ( 'NONE', #5324, #5195, #22016, .T. ) ;
#18933 = CARTESIAN_POINT ( 'NONE',  ( 3.464101615137757051, -5.999999999999979572, -125.4136751345948113 ) ) ;
#18934 =( BOUNDED_CURVE ( )  B_SPLINE_CURVE ( 2, ( #20208, #19734, #13012, #19886, #17769, #3585, #24938, #8193, #8512 ),
 .UNSPECIFIED., .F., .F. ) 
 B_SPLINE_CURVE_WITH_KNOTS ( ( 3, 2, 2, 2, 3 ),
 ( 0.8235294117647058432, 0.8308823529411765163, 0.8382352941176470784, 0.8455882352941176405, 0.8529411764705882026 ),
 .UNSPECIFIED. ) 
 CURVE ( )  GEOMETRIC_REPRESENTATION_ITEM ( )  RATIONAL_B_SPLINE_CURVE ( ( 1.000000000000000000, 0.9238795325112867385, 1.000000000000000000, 0.9238795325112867385, 1.000000000000000000, 0.9238795325112867385, 1.000000000000000000, 0.9238795325112867385, 1.000000000000000000 ) ) 
 REPRESENTATION_ITEM ( '' )  );
#18935 = DIRECTION ( 'NONE',  ( 1.000000000000000000, -5.551115123125773458E-17, -1.260129944081490338E-35 ) ) ;
#18936 = ORIENTED_EDGE ( 'NONE', *, *, #12182, .T. ) ;
#18937 = ORIENTED_EDGE ( 'NONE', *, *, #20218, .T. ) ;
#18938 = CARTESIAN_POINT ( 'NONE',  ( 151.5863248654052313, 0.000000000000000000, 5.500000000000005329 ) ) ;
#18939 = CARTESIAN_POINT ( 'NONE',  ( 137.1562500000000284, -6.000000000000005329, 2.485281374238555774 ) ) ;
#18940 =( BOUNDED_CURVE ( )  B_SPLINE_CURVE ( 2, ( #22025, #517, #17438, #14971, #22182, #26752, #29214, #29067, #12692 ),
 .UNSPECIFIED., .F., .T. ) 
 B_SPLINE_CURVE_WITH_KNOTS ( ( 3, 2, 2, 2, 3 ),
 ( 0.3235294117647058987, 0.3308823529411764608, 0.3382352941176470784, 0.3455882352941176405, 0.3529411764705882582 ),
 .UNSPECIFIED. ) 
 CURVE ( )  GEOMETRIC_REPRESENTATION_ITEM ( )  RATIONAL_B_SPLINE_CURVE ( ( 1.000000000000000000, 0.9238795325112867385, 1.000000000000000000, 0.9238795325112867385, 1.000000000000000000, 0.9238795325112867385, 1.000000000000000000, 0.9238795325112867385, 1.000000000000000000 ) ) 
 REPRESENTATION_ITEM ( '' )  );
#18941 = ORIENTED_EDGE ( 'NONE', *, *, #21467, .F. ) ;
#18942 = CARTESIAN_POINT ( 'NONE',  ( 3.608439182435180470, 6.249999999999982236, -142.1919872981078470 ) ) ;
#18943 = FILL_AREA_STYLE_COLOUR ( '', #21605 ) ;
#18944 = CARTESIAN_POINT ( 'NONE',  ( 9.937500000000024869, -2.649519052838178457, -1.097466725451559322 ) ) ;
#18945 = DIRECTION ( 'NONE',  ( 0.000000000000000000, 0.000000000000000000, -1.000000000000000000 ) ) ;
#18946 = CARTESIAN_POINT ( 'NONE',  ( 20.31250000000012079, -0.8284271247461152399, 2.000000000000031530 ) ) ;
#18947 = CARTESIAN_POINT ( 'NONE',  ( 142.5788997308104058, -4.999999999999989342, 2.071067811865468400 ) ) ;
#18948 = DIRECTION ( 'NONE',  ( -7.147005652999508048E-36, 5.642372883946980038E-36, 1.000000000000000000 ) ) ;
#18949 = DIRECTION ( 'NONE',  ( -0.000000000000000000, -1.000000000000000000, 0.000000000000000000 ) ) ;
#18950 = CARTESIAN_POINT ( 'NONE',  ( 15.03867513459491967, 1.665334536937734811E-13, -2.500000000000057732 ) ) ;
#18951 = CIRCLE ( 'NONE', #25265, 17.50000000000000355 ) ;
#18952 = CARTESIAN_POINT ( 'NONE',  ( 5.196152422706629359, 3.000000000000002665, -60.53867513459481842 ) ) ;
#18953 = CARTESIAN_POINT ( 'NONE',  ( -5.999999999999963585, -1.487416814333745711E-14, -113.3363248654052029 ) ) ;
#18954 = CARTESIAN_POINT ( 'NONE',  ( 110.7499999999998010, 2.775557561562891351E-14, -2.499999999999946709 ) ) ;
#18955 = DIRECTION ( 'NONE',  ( -1.000000000000000000, -1.665334536937731113E-16, 1.526556658859586792E-16 ) ) ;
#18956 = CARTESIAN_POINT ( 'NONE',  ( 14.41367513459493388, 1.767766952966431937, 1.767766952966376426 ) ) ;
#18957 = ORIENTED_EDGE ( 'NONE', *, *, #12342, .T. ) ;
#18958 = EDGE_CURVE ( 'NONE', #21900, #7029, #30224, .T. ) ;
#18959 = CARTESIAN_POINT ( 'NONE',  ( 3.175426480543072749, 5.499999999999865885, -57.12500000000006395 ) ) ;
#18960 = LINE ( 'NONE', #27973, #3089 ) ;
#18961 = EDGE_CURVE ( 'NONE', #24855, #12501, #23408, .T. ) ;
#18962 = CARTESIAN_POINT ( 'NONE',  ( 0.000000000000000000, -5.999999999999991118, -151.9613248654052597 ) ) ;
#18963 = AXIS2_PLACEMENT_3D ( 'NONE', #17614, #8519, #26932 ) ;
#18964 = EDGE_LOOP ( 'NONE', ( #12223, #22786, #25664, #29615 ) ) ;
#18965 = CARTESIAN_POINT ( 'NONE',  ( 117.6247167782375840, 1.849990392679551343, 0.000000000000000000 ) ) ;
#18966 = CARTESIAN_POINT ( 'NONE',  ( 139.4062500000000284, 6.000000000000005329, -2.485281374238556218 ) ) ;
#18967 = CARTESIAN_POINT ( 'NONE',  ( 12.31250000000004974, -0.8284271247461753029, 2.000000000000091926 ) ) ;
#18968 = CARTESIAN_POINT ( 'NONE',  ( -5.412658773652684552, -3.125000000000099920, -99.56698729810781856 ) ) ;
#18969 = CARTESIAN_POINT ( 'NONE',  ( 6.000000000000000888, 5.577813053751546416E-15, -177.0863248654052597 ) ) ;
#18970 = CARTESIAN_POINT ( 'NONE',  ( 132.6562500000000284, -6.000000000000005329, 2.485281374238555774 ) ) ;
#18971 = CARTESIAN_POINT ( 'NONE',  ( 117.1249999999999432, 1.767766952966320915, 1.767766952966431937 ) ) ;
#18972 =( GEOMETRIC_REPRESENTATION_CONTEXT ( 3 ) GLOBAL_UNCERTAINTY_ASSIGNED_CONTEXT ( ( #23770 ) ) GLOBAL_UNIT_ASSIGNED_CONTEXT ( ( #25367, #6943, #14360 ) ) REPRESENTATION_CONTEXT ( 'NONE', 'WORKASPACE' ) );
#18973 = CARTESIAN_POINT ( 'NONE',  ( 6.350852961086080661, -9.614813431917819062E-14, -129.3750000000000284 ) ) ;
#18974 = ORIENTED_EDGE ( 'NONE', *, *, #20873, .F. ) ;
#18975 = CARTESIAN_POINT ( 'NONE',  ( -2.775557561562891351E-14, -5.500000000000115463, -63.75000000000002842 ) ) ;
#18976 = CARTESIAN_POINT ( 'NONE',  ( 0.000000000000000000, 5.999999999999977796, -115.7886751345948397 ) ) ;
#18977 = CARTESIAN_POINT ( 'NONE',  ( 108.8511751345945981, -1.999999999999941602, -0.8284271247459952248 ) ) ;
#18978 = CARTESIAN_POINT ( 'NONE',  ( 5.999999999999974243, 1.607695154586759934, -140.0966878364870354 ) ) ;
#18979 = CARTESIAN_POINT ( 'NONE',  ( 104.4372167782374419, 0.7662911109077987781, -1.849990392679231599 ) ) ;
#18980 = CARTESIAN_POINT ( 'NONE',  ( 140.8041911596568241, -11.60838231931462339, -4.059228028635601504 ) ) ;
#18981 =( BOUNDED_CURVE ( )  B_SPLINE_CURVE ( 2, ( #9408, #9864, #21543, #11905, #28712, #7249, #18796, #5223, #16944 ),
 .UNSPECIFIED., .F., .F. ) 
 B_SPLINE_CURVE_WITH_KNOTS ( ( 3, 2, 2, 2, 3 ),
 ( 0.6764705882352941568, 0.6838235294117647189, 0.6911764705882352811, 0.6985294117647058432, 0.7058823529411765163 ),
 .UNSPECIFIED. ) 
 CURVE ( )  GEOMETRIC_REPRESENTATION_ITEM ( )  RATIONAL_B_SPLINE_CURVE ( ( 1.000000000000000000, 0.9238795325112867385, 1.000000000000000000, 0.9238795325112867385, 1.000000000000000000, 0.9238795325112867385, 1.000000000000000000, 0.9238795325112867385, 1.000000000000000000 ) ) 
 REPRESENTATION_ITEM ( '' )  );
#18982 = CARTESIAN_POINT ( 'NONE',  ( 120.9377832217621034, -1.849990392679562001, -0.7662911109077087390 ) ) ;
#18983 = AXIS2_PLACEMENT_3D ( 'NONE', #14093, #53, #13780 ) ;
#18984 = CARTESIAN_POINT ( 'NONE',  ( -4.763139720814407951, 2.749999999999946709, -139.2499999999999716 ) ) ;
#18985 = CARTESIAN_POINT ( 'NONE',  ( 0.000000000000000000, -5.999999999999991118, -105.4613248654052171 ) ) ;
#18986 = DIRECTION ( 'NONE',  ( -1.000000000000000000, -1.067522139062651411E-16, 0.000000000000000000 ) ) ;
#18987 = CARTESIAN_POINT ( 'NONE',  ( 18.46132486540535922, 1.665334536937734811E-13, -2.500000000000113243 ) ) ;
#18988 = CARTESIAN_POINT ( 'NONE',  ( -2.775557561562891351E-14, -5.500000000000115463, -78.74999999999998579 ) ) ;
#18989 = CARTESIAN_POINT ( 'NONE',  ( 6.000000000000000888, -1.859271017917181981E-14, -114.6636751345948255 ) ) ;
#18990 = CARTESIAN_POINT ( 'NONE',  ( -3.464101615137725076, 5.999999999999979572, -173.5863248654052313 ) ) ;
#18991 = CARTESIAN_POINT ( 'NONE',  ( -4.763139720814407951, 2.749999999999946709, -64.25000000000002842 ) ) ;
#18992 = ADVANCED_FACE ( 'NONE', ( #21873 ), #8023, .T. ) ;
#18993 = CARTESIAN_POINT ( 'NONE',  ( 142.8898502691896510, 3.535533905932725318, -3.535533905932725318 ) ) ;
#18994 = CARTESIAN_POINT ( 'NONE',  ( -5.999999999999968026, -1.607695154586722186, -148.3466878364870354 ) ) ;
#18995 = CARTESIAN_POINT ( 'NONE',  ( 159.6562500000000568, -6.000000000000005329, 2.485281374238556218 ) ) ;
#18996 = SURFACE_STYLE_FILL_AREA ( #16106 ) ;
#18997 = CARTESIAN_POINT ( 'NONE',  ( -5.999999999999963585, 8.134310703387671600E-14, -140.9136751345947971 ) ) ;
#18998 = CARTESIAN_POINT ( 'NONE',  ( -0.5000000000000004441, -10.50000000000000888, -8.000000000000007105 ) ) ;
#18999 = CARTESIAN_POINT ( 'NONE',  ( 118.9997167782376266, -1.308140751793529510, 1.308140751793973600 ) ) ;
#19000 = LINE ( 'NONE', #2049, #10089 ) ;
#19001 = ORIENTED_EDGE ( 'NONE', *, *, #27883, .T. ) ;
#19002 = CARTESIAN_POINT ( 'NONE',  ( 151.5937500000000284, 6.000000000000005329, 2.485281374238585972 ) ) ;
#19003 = CARTESIAN_POINT ( 'NONE',  ( 115.0002832217621886, -1.308140751793585022, -1.308140751793640533 ) ) ;
#19004 = VECTOR ( 'NONE', #19971, 1000.000000000000000 ) ;
#19005 = FACE_OUTER_BOUND ( 'NONE', #29676, .T. ) ;
#19006 = VERTEX_POINT ( 'NONE', #10351 ) ;
#19007 = CARTESIAN_POINT ( 'NONE',  ( 19.87500000000017053, 1.414213562373312083, -1.414213562373145550 ) ) ;
#19008 = ORIENTED_EDGE ( 'NONE', *, *, #6262, .F. ) ;
#19009 = CARTESIAN_POINT ( 'NONE',  ( 3.175426480543072749, -5.500000000000105693, -87.62500000000000000 ) ) ;
#19010 = CARTESIAN_POINT ( 'NONE',  ( 2.775557561562891351E-14, -6.250000000000061284, -101.6830127018922241 ) ) ;
#19011 = ORIENTED_EDGE ( 'NONE', *, *, #22293, .F. ) ;
#19012 = CARTESIAN_POINT ( 'NONE',  ( 153.9226497308104058, 5.000000000000004441, 0.000000000000000000 ) ) ;
#19013 = EDGE_CURVE ( 'NONE', #11662, #379, #12828, .T. ) ;
#19014 = CARTESIAN_POINT ( 'NONE',  ( 4.763139720814407951, -2.749999999999988454, -167.0000000000000284 ) ) ;
#19015 = CARTESIAN_POINT ( 'NONE',  ( 2.145494852022844068, -10.79031218954989235, -19.39330237445247462 ) ) ;
#19016 = DIRECTION ( 'NONE',  ( -7.147005652999508048E-36, 5.642372883946980038E-36, 1.000000000000000000 ) ) ;
#19017 = PRESENTATION_LAYER_ASSIGNMENT (  '', '', ( #16097 ) ) ;
#19018 = B_SPLINE_CURVE_WITH_KNOTS ( 'NONE', 3,
 ( #19735, #29083, #17611, #20209 ),
 .UNSPECIFIED., .F., .F.,
 ( 4, 4 ),
 ( 0.000000000000000000, 0.0004007166227139782183 ),
 .UNSPECIFIED. ) ;
#19019 =( NAMED_UNIT ( * ) PLANE_ANGLE_UNIT ( ) SI_UNIT ( $, .RADIAN. ) );
#19020 =( BOUNDED_CURVE ( )  B_SPLINE_CURVE ( 2, ( #26450, #26737, #5403, #24297, #14812, #17276, #14958, #3245, #5705 ),
 .UNSPECIFIED., .F., .T. ) 
 B_SPLINE_CURVE_WITH_KNOTS ( ( 3, 2, 2, 2, 3 ),
 ( 0.9027777777777777901, 0.9037037037037036757, 0.9055555555555555580, 0.9074074074074074403, 0.9083333333333333259 ),
 .UNSPECIFIED. ) 
 CURVE ( )  GEOMETRIC_REPRESENTATION_ITEM ( )  RATIONAL_B_SPLINE_CURVE ( ( 0.9330127018922194093, 0.9330127018922194093, 1.000000000000000000, 0.8660254037844388186, 1.000000000000000000, 0.8660254037844388186, 1.000000000000000000, 0.9330127018922194093, 0.9330127018922194093 ) ) 
 REPRESENTATION_ITEM ( '' )  );
#19021 = CARTESIAN_POINT ( 'NONE',  ( -6.350852961085760029, -1.281975124255709124E-13, -172.1250000000000284 ) ) ;
#19022 = CARTESIAN_POINT ( 'NONE',  ( 160.7886751345948255, 5.500000000000005329, 0.000000000000000000 ) ) ;
#19023 = CARTESIAN_POINT ( 'NONE',  ( -3.175426480542816510, -5.500000000000057732, -156.8750000000000284 ) ) ;
#19024 = VECTOR ( 'NONE', #8305, 1000.000000000000000 ) ;
#19025 = CARTESIAN_POINT ( 'NONE',  ( 111.1249999999999289, 1.767766952966320915, 1.767766952966431937 ) ) ;
#19026 = CARTESIAN_POINT ( 'NONE',  ( -5.999999999999963585, 1.780251999655701777E-13, -104.3363248654052313 ) ) ;
#19027 = CARTESIAN_POINT ( 'NONE',  ( -2.775557561562891351E-14, -5.500000000000115463, -104.2500000000000142 ) ) ;
#19028 = CARTESIAN_POINT ( 'NONE',  ( -5.999999999999963585, -1.487416814333745711E-14, -59.33632486540522422 ) ) ;
#19030 = CARTESIAN_POINT ( 'NONE',  ( 3.175426480543072749, -5.500000000000105693, -86.12500000000000000 ) ) ;
#19029 = CARTESIAN_POINT ( 'NONE',  ( 4.763139720814407951, 2.750000000000002665, -156.2500000000000000 ) ) ;
#19031 = EDGE_CURVE ( 'NONE', #5164, #16308, #21421, .T. ) ;
#19032 = CARTESIAN_POINT ( 'NONE',  ( 155.9211002691896510, -4.999999999999989342, -2.071067811865468400 ) ) ;
#19033 = CARTESIAN_POINT ( 'NONE',  ( -9.999999999999765521, -90.00000000000001421, -3.000000000000002665 ) ) ;
#19034 = VERTEX_POINT ( 'NONE', #20471 ) ;
#19035 = CARTESIAN_POINT ( 'NONE',  ( 23.00000000000013145, 2.000000000000168310, 0.000000000000000000 ) ) ;
#19036 = CARTESIAN_POINT ( 'NONE',  ( 111.2499999999999432, -1.110223024625156540E-13, 2.500000000000057732 ) ) ;
#19037 = DIRECTION ( 'NONE',  ( 0.000000000000000000, 0.000000000000000000, -1.000000000000000000 ) ) ;
#19038 = CARTESIAN_POINT ( 'NONE',  ( 106.1252832217622171, -5.551115123125782702E-14, -1.849990392679523588 ) ) ;
#19039 = LINE ( 'NONE', #3006, #21364 ) ;
#19040 = ORIENTED_EDGE ( 'NONE', *, *, #5791, .F. ) ;
#19041 = FILL_AREA_STYLE_COLOUR ( '', #2847 ) ;
#19042 = DIRECTION ( 'NONE',  ( 1.000000000000000000, -3.469446951953694061E-16, -0.000000000000000000 ) ) ;
#19044 = CARTESIAN_POINT ( 'NONE',  ( 106.8747167782375840, 2.775557561562891351E-14, 1.849990392679745632 ) ) ;
#19043 = VECTOR ( 'NONE', #8225, 1000.000000000000000 ) ;
#19045 = ORIENTED_EDGE ( 'NONE', *, *, #9883, .T. ) ;
#19046 = CARTESIAN_POINT ( 'NONE',  ( 146.2500000000000568, -6.000000000000005329, 0.000000000000000000 ) ) ;
#19047 = ORIENTED_EDGE ( 'NONE', *, *, #23220, .T. ) ;
#19048 = CARTESIAN_POINT ( 'NONE',  ( 3.175426480543072749, 5.499999999999865885, -109.6249999999999716 ) ) ;
#19049 = CARTESIAN_POINT ( 'NONE',  ( 18.56250000000008171, 1.097466725451679892, 2.649519052838358757 ) ) ;
#19050 = CARTESIAN_POINT ( 'NONE',  ( -5.412658773652684552, -3.125000000000099920, -122.9330127018922809 ) ) ;
#19051 = VERTEX_POINT ( 'NONE', #22940 ) ;
#19052 = CARTESIAN_POINT ( 'NONE',  ( -3.464101615137725076, 5.999999999999979572, -57.16367513459482552 ) ) ;
#19053 = CARTESIAN_POINT ( 'NONE',  ( -3.608439182435052128, -6.250000000000110134, -172.9419872981078470 ) ) ;
#19054 = CARTESIAN_POINT ( 'NONE',  ( 107.0624999999998010, 2.500000000000114575, 1.035533905932989551 ) ) ;
#19055 = CIRCLE ( 'NONE', #12184, 1.000000000000000000 ) ;
#19056 = EDGE_CURVE ( 'NONE', #14326, #16412, #25211, .T. ) ;
#19057 = ORIENTED_EDGE ( 'NONE', *, *, #28272, .T. ) ;
#19058 = CARTESIAN_POINT ( 'NONE',  ( -1.960615434941527013, 10.82557180451506973, -19.32589338774631926 ) ) ;
#19059 = SURFACE_STYLE_FILL_AREA ( #23946 ) ;
#19060 = CARTESIAN_POINT ( 'NONE',  ( 4.763139720814407951, -2.749999999999988454, -176.0000000000000568 ) ) ;
#19061 = CARTESIAN_POINT ( 'NONE',  ( 107.3127832217622313, 1.849990392679501827, -0.7662911109076485650 ) ) ;
#19062 = CARTESIAN_POINT ( 'NONE',  ( 2.775557561562891351E-14, -6.250000000000061284, -173.6830127018922383 ) ) ;
#19063 = CARTESIAN_POINT ( 'NONE',  ( -5.196152422706601826, 2.999999999999975131, -75.96132486540518869 ) ) ;
#19064 = CIRCLE ( 'NONE', #21971, 11.00000000000001599 ) ;
#19065 = VECTOR ( 'NONE', #29872, 1000.000000000000000 ) ;
#19066 = CARTESIAN_POINT ( 'NONE',  ( 0.000000000000000000, 5.999999999999977796, -123.2886751345948539 ) ) ;
#19067 = EDGE_CURVE ( 'NONE', #15961, #2390, #18194, .T. ) ;
#19068 = CARTESIAN_POINT ( 'NONE',  ( 4.763139720814407951, -2.749999999999988454, -112.9999999999999858 ) ) ;
#19069 = CARTESIAN_POINT ( 'NONE',  ( -5.999999999999963585, -1.487416814333745711E-14, -59.91367513459483263 ) ) ;
#19070 = CARTESIAN_POINT ( 'NONE',  ( -3.464101615137725076, 5.999999999999979572, -88.66367513459483973 ) ) ;
#19071 = EDGE_LOOP ( 'NONE', ( #8553, #27876, #6957, #7706 ) ) ;
#19072 = CARTESIAN_POINT ( 'NONE',  ( 18.81250000000001776, 1.097466725451559322, 2.649519052838419153 ) ) ;
#19073 = DIRECTION ( 'NONE',  ( 0.000000000000000000, 0.000000000000000000, -1.000000000000000000 ) ) ;
#19074 = LINE ( 'NONE', #17214, #7221 ) ;
#19075 = CARTESIAN_POINT ( 'NONE',  ( 0.000000000000000000, 5.999999999999977796, -155.7113248654052313 ) ) ;
#19076 = ORIENTED_EDGE ( 'NONE', *, *, #9744, .T. ) ;
#19077 = CARTESIAN_POINT ( 'NONE',  ( -5.999999999999963585, -1.487416814333745711E-14, -113.3363248654052029 ) ) ;
#19078 = CARTESIAN_POINT ( 'NONE',  ( 3.464101615137852974, 5.999999999999884537, -109.9136751345947971 ) ) ;
#19079 = CARTESIAN_POINT ( 'NONE',  ( 157.3199251345948824, -2.278174593051950136, -5.500000000000074607 ) ) ;
#19080 = CARTESIAN_POINT ( 'NONE',  ( 0.000000000000000000, 0.000000000000000000, 0.000000000000000000 ) ) ;
#19081 = CARTESIAN_POINT ( 'NONE',  ( -5.196152422706601826, 2.999999999999975131, -141.0386751345948255 ) ) ;
#19082 = CARTESIAN_POINT ( 'NONE',  ( 136.4062500000000568, 6.000000000000005329, -2.485281374238555774 ) ) ;
#19083 = VERTEX_POINT ( 'NONE', #8807 ) ;
#19084 = CARTESIAN_POINT ( 'NONE',  ( 2.775557561562891351E-14, 6.250000000000033751, -139.0669872981078470 ) ) ;
#19085 = DIRECTION ( 'NONE',  ( 1.000000000000000000, -0.000000000000000000, -0.000000000000000000 ) ) ;
#19086 = CARTESIAN_POINT ( 'NONE',  ( 11.75000000000012079, -1.873492889144845464, 1.873492889144900975 ) ) ;
#19087 = LINE ( 'NONE', #28408, #22123 ) ;
#19088 = ADVANCED_FACE ( 'NONE', ( #1419 ), #29831, .F. ) ;
#19089 = CARTESIAN_POINT ( 'NONE',  ( 17.62500000000008527, -1.414213562372923505, -1.414213562373145550 ) ) ;
#19090 = CARTESIAN_POINT ( 'NONE',  ( 8.673617379884035472E-16, -14.99923475244192339, 9.015151515151522688 ) ) ;
#19091 = CARTESIAN_POINT ( 'NONE',  ( 136.3913997308104058, -2.071067811865468400, 4.999999999999989342 ) ) ;
#19092 = CARTESIAN_POINT ( 'NONE',  ( -5.196152422706573404, -3.000000000000002665, -119.7886751345948397 ) ) ;
#19093 = CARTESIAN_POINT ( 'NONE',  ( 0.000000000000000000, 5.999999999999977796, -92.71132486540523132 ) ) ;
#19094 = CARTESIAN_POINT ( 'NONE',  ( -5.999999999999963585, -1.487416814333745711E-14, -59.91367513459483263 ) ) ;
#19095 = CARTESIAN_POINT ( 'NONE',  ( 105.3749999999999005, -1.767766952966320915, 1.767766952966431937 ) ) ;
#19096 = ADVANCED_FACE ( 'NONE', ( #8487 ), #24606, .T. ) ;
#19097 = CARTESIAN_POINT ( 'NONE',  ( 15.46132486540530238, 1.110223024625156540E-13, -2.500000000000057732 ) ) ;
#19098 = CARTESIAN_POINT ( 'NONE',  ( 14.28867513459491967, 2.500000000000224265, -5.551115123125782702E-14 ) ) ;
#19099 = ORIENTED_EDGE ( 'NONE', *, *, #14553, .F. ) ;
#19100 = DIRECTION ( 'NONE',  ( 0.000000000000000000, 1.000000000000000000, -1.224646799147353207E-16 ) ) ;
#19101 = CARTESIAN_POINT ( 'NONE',  ( 0.000000000000000000, 5.999999999999977796, -62.71132486540520290 ) ) ;
#19102 =( BOUNDED_CURVE ( )  B_SPLINE_CURVE ( 2, ( #5332, #7496, #23951, #26385, #26234, #14743, #7789, #12602, #28671 ),
 .UNSPECIFIED., .F., .T. ) 
 B_SPLINE_CURVE_WITH_KNOTS ( ( 3, 2, 2, 2, 3 ),
 ( 0.5000000000000000000, 0.5073529411764705621, 0.5147058823529411242, 0.5220588235294116863, 0.5294117647058823595 ),
 .UNSPECIFIED. ) 
 CURVE ( )  GEOMETRIC_REPRESENTATION_ITEM ( )  RATIONAL_B_SPLINE_CURVE ( ( 1.000000000000000000, 0.9238795325112867385, 1.000000000000000000, 0.9238795325112867385, 1.000000000000000000, 0.9238795325112867385, 1.000000000000000000, 0.9238795325112867385, 1.000000000000000000 ) ) 
 REPRESENTATION_ITEM ( '' )  );
#19103 = ORIENTED_EDGE ( 'NONE', *, *, #15498, .T. ) ;
#19104 = CARTESIAN_POINT ( 'NONE',  ( 116.1872167782374987, -1.849990392679532247, -0.7662911109077087390 ) ) ;
#19105 = CARTESIAN_POINT ( 'NONE',  ( 137.0625000000000284, -4.242640687119298093, 4.242640687119298093 ) ) ;
#19106 = CARTESIAN_POINT ( 'NONE',  ( 2.775557561562891351E-14, 6.250000000000033751, -104.5669872981078186 ) ) ;
#19107 = CARTESIAN_POINT ( 'NONE',  ( 138.4613248654052313, -5.500000000000005329, 0.000000000000000000 ) ) ;
#19108 =( BOUNDED_CURVE ( )  B_SPLINE_CURVE ( 2, ( #25497, #6617, #2467, #14188, #2013, #9539, #4904, #20767, #30113 ),
 .UNSPECIFIED., .F., .F. ) 
 B_SPLINE_CURVE_WITH_KNOTS ( ( 3, 2, 2, 2, 3 ),
 ( 0.03611111111111110772, 0.03703703703703703498, 0.03888888888888888951, 0.04074074074074074403, 0.04166666666666667129 ),
 .UNSPECIFIED. ) 
 CURVE ( )  GEOMETRIC_REPRESENTATION_ITEM ( )  RATIONAL_B_SPLINE_CURVE ( ( 0.9330127018922194093, 0.9330127018922191873, 1.000000000000000000, 0.8660254037844388186, 1.000000000000000000, 0.8660254037844388186, 1.000000000000000000, 0.9330127018922191873, 0.9330127018922194093 ) ) 
 REPRESENTATION_ITEM ( '' )  );
#19109 = CARTESIAN_POINT ( 'NONE',  ( 134.6250000000000284, 0.000000000000000000, -6.000000000000005329 ) ) ;
#19110 = CARTESIAN_POINT ( 'NONE',  ( -2.775557561562891351E-14, -5.500000000000115463, -131.2500000000000284 ) ) ;
#19111 = ORIENTED_EDGE ( 'NONE', *, *, #7417, .F. ) ;
#19112 = CARTESIAN_POINT ( 'NONE',  ( -6.350852961085760029, -1.281975124255709124E-13, -56.62500000000004974 ) ) ;
#19113 = EDGE_CURVE ( 'NONE', #23217, #29417, #21882, .T. ) ;
#19114 = CARTESIAN_POINT ( 'NONE',  ( 6.000000000000007105, -1.607695154586741060, -179.2306624327026157 ) ) ;
#19115 = CARTESIAN_POINT ( 'NONE',  ( 140.5384615384615756, -11.07692307692306777, -4.615384615384604317 ) ) ;
#19116 = ADVANCED_FACE ( 'NONE', ( #8960 ), #13596, .T. ) ;
#19117 = CARTESIAN_POINT ( 'NONE',  ( 3.608439182435180470, 6.249999999999982236, -81.55801270189219565 ) ) ;
#19118 = CARTESIAN_POINT ( 'NONE',  ( -0.5000000000000007772, -10.00000000000000711, -4.414213562373099364 ) ) ;
#19119 = CARTESIAN_POINT ( 'NONE',  ( -3.464101615137757051, -5.999999999999979572, -176.0863248654052313 ) ) ;
#19120 = LINE ( 'NONE', #502, #11880 ) ;
#19121 = CARTESIAN_POINT ( 'NONE',  ( 116.9377832217621460, -1.849990392679441875, -0.7662911109077087390 ) ) ;
#19122 = ITEM_DEFINED_TRANSFORMATION ( 'NONE', 'NONE', #27128,  #18805 ) ;
#19123 = CARTESIAN_POINT ( 'NONE',  ( 0.000000000000000000, 5.499999999999991118, -144.0000000000000284 ) ) ;
#19124 = CARTESIAN_POINT ( 'NONE',  ( -5.196152422706573404, -3.000000000000002665, -105.7113248654052455 ) ) ;
#19125 = CARTESIAN_POINT ( 'NONE',  ( -5.412658773652684552, -3.125000000000099920, -155.9330127018922383 ) ) ;
#19126 = CARTESIAN_POINT ( 'NONE',  ( 5.999999999999897859, 1.607695154586893826, -117.0193375672974412 ) ) ;
#19127 = CARTESIAN_POINT ( 'NONE',  ( -6.350852961085760029, -1.281975124255709124E-13, -68.62500000000002842 ) ) ;
#19128 = CARTESIAN_POINT ( 'NONE',  ( 6.000000000000001776, 5.345404176511898156E-15, -174.0863248654052597 ) ) ;
#19129 = CARTESIAN_POINT ( 'NONE',  ( 0.000000000000000000, 5.499999999999991118, -69.00000000000000000 ) ) ;
#19130 = CARTESIAN_POINT ( 'NONE',  ( 104.9735375947738589, -0.8915860325701192579, -1.786451901258863995 ) ) ;
#19131 = CARTESIAN_POINT ( 'NONE',  ( 157.9687500000000568, -2.485281374238585972, 6.000000000000005329 ) ) ;
#19132 = DIRECTION ( 'NONE',  ( -1.000000000000000000, -1.665334536937731113E-16, 1.526556658859586792E-16 ) ) ;
#19133 = CYLINDRICAL_SURFACE ( 'NONE', #23439, 2.499999999999999112 ) ;
#19134 = CARTESIAN_POINT ( 'NONE',  ( 115.2497167782374419, -1.308140751793557266, -1.308140751793751555 ) ) ;
#19135 = ORIENTED_EDGE ( 'NONE', *, *, #1974, .F. ) ;
#19136 = VECTOR ( 'NONE', #11737, 1000.000000000000000 ) ;
#19137 = CARTESIAN_POINT ( 'NONE',  ( 152.7187500000000284, 2.485281374238555774, -6.000000000000005329 ) ) ;
#19138 = CARTESIAN_POINT ( 'NONE',  ( 119.2886751345947260, 1.999999999999946265, 1.110223024625156540E-13 ) ) ;
#19139 = VECTOR ( 'NONE', #10126, 1000.000000000000000 ) ;
#19140 = CARTESIAN_POINT ( 'NONE',  ( 112.9377832217622171, -1.849990392679381701, -0.7662911109076485650 ) ) ;
#19141 = AXIS2_PLACEMENT_3D ( 'NONE', #26337, #14559, #2990 ) ;
#19142 = DIRECTION ( 'NONE',  ( -1.000000000000000000, 0.000000000000000000, 0.000000000000000000 ) ) ;
#19143 = CARTESIAN_POINT ( 'NONE',  ( -3.175426480542816510, -5.500000000000057732, -180.8750000000000000 ) ) ;
#19144 = CARTESIAN_POINT ( 'NONE',  ( 22.75000000000015987, 1.110223024625156540E-13, -2.000000000000168310 ) ) ;
#19145 = CARTESIAN_POINT ( 'NONE',  ( 3.608439182435180470, -6.249999999999997335, -156.1919872981078470 ) ) ;
#19146 = ORIENTED_EDGE ( 'NONE', *, *, #2081, .F. ) ;
#19147 = CARTESIAN_POINT ( 'NONE',  ( -4.763139720814407951, -2.750000000000016431, -82.00000000000001421 ) ) ;
#19148 = CARTESIAN_POINT ( 'NONE',  ( 16.00000000000012434, -1.873492889144789952, -1.873492889145067508 ) ) ;
#19149 = ADVANCED_FACE ( 'NONE', ( #12988 ), #1727, .T. ) ;
#19150 = CARTESIAN_POINT ( 'NONE',  ( -3.608439182435115633, 6.249999999999965361, -100.8080127018922383 ) ) ;
#19151 = EDGE_LOOP ( 'NONE', ( #4345, #18069, #17484, #17233 ) ) ;
#19152 = DIRECTION ( 'NONE',  ( -7.147005652999508048E-36, 5.642372883946980038E-36, 1.000000000000000000 ) ) ;
#19153 = CARTESIAN_POINT ( 'NONE',  ( 156.3601497308104058, -3.535533905932725318, -3.535533905932725318 ) ) ;
#19154 = CARTESIAN_POINT ( 'NONE',  ( -5.999999999999963585, 1.780251999655701777E-13, -53.91367513459482552 ) ) ;
#19155 = FACE_OUTER_BOUND ( 'NONE', #8430, .T. ) ;
#19156 = MECHANICAL_DESIGN_GEOMETRIC_PRESENTATION_REPRESENTATION (  '', ( #13788 ), #8864 ) ;
#19157 = CARTESIAN_POINT ( 'NONE',  ( -4.999999999999990230, -24.99999999999999289, -4.000000000000003553 ) ) ;
#19158 =( LENGTH_UNIT ( ) NAMED_UNIT ( * ) SI_UNIT ( .MILLI., .METRE. ) );
#19159 = CARTESIAN_POINT ( 'NONE',  ( 6.350852961086080661, -9.614813431917819062E-14, -160.8750000000000284 ) ) ;
#19160 = CARTESIAN_POINT ( 'NONE',  ( -5.999999999999963585, 8.134310703387671600E-14, -142.4136751345948539 ) ) ;
#19161 = CARTESIAN_POINT ( 'NONE',  ( -3.175426480542816510, 5.499999999999865885, -155.8750000000000000 ) ) ;
#19162 = CARTESIAN_POINT ( 'NONE',  ( 111.8124999999997584, 1.035533905932779275, -2.499999999999964473 ) ) ;
#19163 = CARTESIAN_POINT ( 'NONE',  ( -6.000000000000007105, -1.607695154586655129, -52.34668783648703538 ) ) ;
#19164 = CARTESIAN_POINT ( 'NONE',  ( -4.763139720814407951, -2.750000000000016431, -94.00000000000002842 ) ) ;
#19165 = CARTESIAN_POINT ( 'NONE',  ( 5.999999999999949374, 1.607695154586804565, -60.01933756729743408 ) ) ;
#19166 = CARTESIAN_POINT ( 'NONE',  ( 6.350852961086080661, -9.614813431917819062E-14, -87.37500000000007105 ) ) ;
#19167 = CARTESIAN_POINT ( 'NONE',  ( 155.2648502691896510, 3.535533905932725318, 3.535533905932752852 ) ) ;
#19168 = CARTESIAN_POINT ( 'NONE',  ( 0.000000000000000000, 0.000000000000000000, 0.000000000000000000 ) ) ;
#19169 = CARTESIAN_POINT ( 'NONE',  ( 24.56250000000017764, -1.999999999999911626, -0.8284271247462354770 ) ) ;
#19170 = CARTESIAN_POINT ( 'NONE',  ( 113.9999999999998153, 2.500000000000085265, 0.000000000000000000 ) ) ;
#19171 = CARTESIAN_POINT ( 'NONE',  ( 24.50000000000010658, 5.551115123125782702E-14, -5.551115123125782702E-14 ) ) ;
#19172 = SURFACE_STYLE_FILL_AREA ( #3149 ) ;
#19173 = CARTESIAN_POINT ( 'NONE',  ( 0.000000000000000000, 0.000000000000000000, 0.000000000000000000 ) ) ;
#19174 = ORIENTED_EDGE ( 'NONE', *, *, #22997, .F. ) ;
#19175 = CARTESIAN_POINT ( 'NONE',  ( 6.000000000000001776, 5.345404176511898156E-15, -179.1636751345948255 ) ) ;
#19176 = CARTESIAN_POINT ( 'NONE',  ( -0.08335392965452037561, -15.22338135603291853, -7.695243043971561114 ) ) ;
#19177 = CARTESIAN_POINT ( 'NONE',  ( 106.0622167782373708, -1.849990392679441875, 0.7662911109080090544 ) ) ;
#19178 = EDGE_CURVE ( 'NONE', #28765, #21961, #7668, .T. ) ;
#19179 = AXIS2_PLACEMENT_3D ( 'NONE', #25469, #18446, #11073 ) ;
#19180 = ORIENTED_EDGE ( 'NONE', *, *, #18028, .F. ) ;
#19181 = ORIENTED_EDGE ( 'NONE', *, *, #4836, .F. ) ;
#19182 = CARTESIAN_POINT ( 'NONE',  ( 3.175426480543072749, 5.499999999999865885, -112.6249999999999858 ) ) ;
#19183 =( BOUNDED_SURFACE ( )  B_SPLINE_SURFACE ( 3, 2, ( 
 ( #6517, #20974, #25398 ),
 ( #25235, #2514, #19425 ),
 ( #14820, #28752, #24162 ),
 ( #665, #24015, #7721 ),
 ( #25868, #12377, #19276 ),
 ( #2660, #21725, #17129 ),
 ( #16689, #7286, #21423 ),
 ( #10047, #26455, #4958 ),
 ( #26011, #354, #14529 ),
 ( #5406, #3104, #5108 ),
 ( #2960, #12530, #21871 ),
 ( #811, #12083, #18828 ) ),
 .UNSPECIFIED., .F., .F., .T. ) 
 B_SPLINE_SURFACE_WITH_KNOTS ( ( 4, 2, 2, 2, 2, 4 ),
 ( 3, 3 ),
 ( 0.0005482801588371855397, 0.001000919478279807106, 0.001227239138001117889, 0.001453558797722428672, 0.001906198117165050238, 0.002358837436607671804 ),
 ( 0.000000000000000000, 1.000000000000000000 ),
 .UNSPECIFIED. ) 
 GEOMETRIC_REPRESENTATION_ITEM ( )  RATIONAL_B_SPLINE_SURFACE ( (
 ( 1.000000000000000000, 0.9165151389911680990, 1.000000000000000000),
 ( 1.000000000000000000, 0.9166361146696374584, 1.000000000000000000),
 ( 1.000000000000000000, 0.9090514103963388548, 1.000000000000000000),
 ( 1.000000000000000000, 0.8902690042825124328, 1.000000000000000000),
 ( 1.000000000000000000, 0.8826973805417798191, 1.000000000000000000),
 ( 1.000000000000000000, 0.8660311221766173739, 1.000000000000000000),
 ( 1.000000000000000000, 0.8568659817695165604, 1.000000000000000000),
 ( 1.000000000000000000, 0.8270719941331442504, 1.000000000000000000),
 ( 1.000000000000000000, 0.8050517830292033272, 1.000000000000000000),
 ( 1.000000000000000000, 0.7576724516402112419, 1.000000000000000000),
 ( 1.000000000000000000, 0.7325062753274510507, 1.000000000000000000),
 ( 1.000000000000000000, 0.7071067811865453523, 1.000000000000000000) ) ) 
 REPRESENTATION_ITEM ( '' )  SURFACE ( )  );
#19184 = EDGE_CURVE ( 'NONE', #9277, #11496, #10668, .T. ) ;
#19185 = CARTESIAN_POINT ( 'NONE',  ( -3.608439182435052128, -6.250000000000110134, -122.8080127018922099 ) ) ;
#19186 = UNCERTAINTY_MEASURE_WITH_UNIT (LENGTH_MEASURE( 1.000000000000000082E-05 ), #18415, 'distance_accuracy_value', 'NONE');
#19187 = ORIENTED_EDGE ( 'NONE', *, *, #8021, .T. ) ;
#19188 = CARTESIAN_POINT ( 'NONE',  ( 113.7738248654049471, 2.000000000000061728, 0.8284271247462955401 ) ) ;
#19189 = CARTESIAN_POINT ( 'NONE',  ( 7.216878364870455975, -6.409875621278545621E-14, -164.9419872981078186 ) ) ;
#19190 = CARTESIAN_POINT ( 'NONE',  ( 108.0624999999998010, 2.500000000000114575, 1.035533905932929599 ) ) ;
#19191 = ORIENTED_EDGE ( 'NONE', *, *, #28736, .F. ) ;
#19192 = CARTESIAN_POINT ( 'NONE',  ( 0.2066402860832207145, -15.46612969915937086, -8.189149229532207031 ) ) ;
#19193 = CARTESIAN_POINT ( 'NONE',  ( 6.000000000000052403, -1.607695154586662678, -132.1533121635129646 ) ) ;
#19194 = CARTESIAN_POINT ( 'NONE',  ( 3.175426480543072749, 5.499999999999865885, -175.6250000000000284 ) ) ;
#19195 = CARTESIAN_POINT ( 'NONE',  ( 109.3127832217620607, 1.849990392679591977, -0.7662911109076485650 ) ) ;
#19196 = CARTESIAN_POINT ( 'NONE',  ( 5.196152422706629359, -2.999999999999988898, -168.7886751345948255 ) ) ;
#19197 = CARTESIAN_POINT ( 'NONE',  ( 5.412658773652739619, 3.124999999999988898, -180.6830127018922383 ) ) ;
#19198 = CARTESIAN_POINT ( 'NONE',  ( 5.999999999999949374, 1.607695154586804565, -76.51933756729745539 ) ) ;
#19199 = DIRECTION ( 'NONE',  ( 1.000000000000000000, -0.000000000000000000, -0.000000000000000000 ) ) ;
#19200 = CARTESIAN_POINT ( 'NONE',  ( -4.763139720814407951, 2.749999999999946709, -127.2500000000000284 ) ) ;
#19201 = CYLINDRICAL_SURFACE ( 'NONE', #25174, 5.500000000000000000 ) ;
#19202 = CARTESIAN_POINT ( 'NONE',  ( -3.175426480542816510, -5.500000000000057732, -110.3750000000000426 ) ) ;
#19203 = COLOUR_RGB ( '', 0.40784314, 0.44705882, 0.49803922) ;
#19204 = ORIENTED_EDGE ( 'NONE', *, *, #24850, .F. ) ;
#19205 = CARTESIAN_POINT ( 'NONE',  ( 6.000000000000000888, -3.330669073875464691E-16, -7.560779664488942560E-35 ) ) ;
#19206 = CARTESIAN_POINT ( 'NONE',  ( 18.02382486540526330, -1.035533905932629173, 2.499999999999904521 ) ) ;
#19207 = ORIENTED_EDGE ( 'NONE', *, *, #16202, .F. ) ;
#19208 = CARTESIAN_POINT ( 'NONE',  ( 118.7113248654050750, 1.999999999999946265, 1.110223024625156540E-13 ) ) ;
#19209 = EDGE_CURVE ( 'NONE', #5164, #1, #24770, .T. ) ;
#19210 = COLOUR_RGB ( '', 0.31764706, 0.68627451, 0.89019608) ;
#19211 = DIRECTION ( 'NONE',  ( -1.000000000000000000, 0.000000000000000000, 0.000000000000000000 ) ) ;
#19212 = CARTESIAN_POINT ( 'NONE',  ( 110.2497167782375698, -1.308140751793585022, -1.308140751793529510 ) ) ;
#19213 = EDGE_CURVE ( 'NONE', #13234, #12154, #6327, .T. ) ;
#19214 = CARTESIAN_POINT ( 'NONE',  ( 0.000000000000000000, 5.999999999999977796, -109.7886751345948397 ) ) ;
#19215 = ORIENTED_EDGE ( 'NONE', *, *, #1151, .F. ) ;
#19216 = CARTESIAN_POINT ( 'NONE',  ( 22.47617513459494631, 1.035533905932869425, 2.499999999999904521 ) ) ;
#19217 = ORIENTED_EDGE ( 'NONE', *, *, #18120, .T. ) ;
#19218 = VERTEX_POINT ( 'NONE', #27060 ) ;
#19219 = CARTESIAN_POINT ( 'NONE',  ( 3.464101615137852974, 5.999999999999884537, -85.33632486540520290 ) ) ;
#19220 = CARTESIAN_POINT ( 'NONE',  ( 134.9211002691897079, -4.999999999999989342, -2.071067811865468400 ) ) ;
#19221 = VECTOR ( 'NONE', #13215, 1000.000000000000000 ) ;
#19222 = ADVANCED_FACE ( 'NONE', ( #6025 ), #13145, .T. ) ;
#19223 = EDGE_LOOP ( 'NONE', ( #13967, #7312, #3151, #22330 ) ) ;
#19224 = CARTESIAN_POINT ( 'NONE',  ( 7.216878364870455975, -6.409875621278545621E-14, -131.9419872981078470 ) ) ;
#19225 = CARTESIAN_POINT ( 'NONE',  ( 24.08632486540529527, -1.767766952966265404, 1.767766952966376426 ) ) ;
#19226 = VECTOR ( 'NONE', #8478, 1000.000000000000000 ) ;
#19227 = CARTESIAN_POINT ( 'NONE',  ( 11.50000000000012079, 1.873492889145067508, 1.873492889144734441 ) ) ;
#19228 = CARTESIAN_POINT ( 'NONE',  ( 144.1949251345948255, 5.500000000000012434, -2.278174593052012309 ) ) ;
#19229 = ORIENTED_EDGE ( 'NONE', *, *, #24816, .F. ) ;
#19230 = CARTESIAN_POINT ( 'NONE',  ( 18.68750000000005329, -0.8284271247461753029, -1.999999999999971800 ) ) ;
#19231 = CARTESIAN_POINT ( 'NONE',  ( 117.7886751345947545, -1.999999999999946265, 1.110223024625156540E-13 ) ) ;
#19232 = CARTESIAN_POINT ( 'NONE',  ( 149.6324251345948539, -5.500000000000012434, -2.278174593052012309 ) ) ;
#19233 = CARTESIAN_POINT ( 'NONE',  ( 135.5476497308104058, 0.000000000000000000, -5.000000000000004441 ) ) ;
#19234 = AXIS2_PLACEMENT_3D ( 'NONE', #16031, #4143, #13723 ) ;
#19235 = CARTESIAN_POINT ( 'NONE',  ( 12.39882486540519047, -1.035533905932629173, -2.500000000000024425 ) ) ;
#19236 = CARTESIAN_POINT ( 'NONE',  ( -5.999999999999904965, -1.607695154586834541, -140.2693375672974412 ) ) ;
#19237 = AXIS2_PLACEMENT_3D ( 'NONE', #4596, #11405, #9065 ) ;
#19238 = CARTESIAN_POINT ( 'NONE',  ( -5.999999999999962697, 3.323446944526963260E-14, -162.8363248654052313 ) ) ;
#19239 = CARTESIAN_POINT ( 'NONE',  ( 107.9374999999997726, 2.500000000000144773, -1.035533905932508825 ) ) ;
#19240 =( BOUNDED_CURVE ( )  B_SPLINE_CURVE ( 2, ( #903, #21682, #28261, #19228, #10003, #28702, #21825, #7240, #26411 ),
 .UNSPECIFIED., .F., .F. ) 
 B_SPLINE_CURVE_WITH_KNOTS ( ( 3, 2, 2, 2, 3 ),
 ( 0.3874999999999999001, 0.3937499999999997669, 0.3999999999999994671, 0.4062499999999992228, 0.4124999999999989786 ),
 .UNSPECIFIED. ) 
 CURVE ( )  GEOMETRIC_REPRESENTATION_ITEM ( )  RATIONAL_B_SPLINE_CURVE ( ( 1.000000000000000666, 0.9238795325112860723, 1.000000000000000000, 0.9238795325112867385, 1.000000000000000000, 0.9238795325112867385, 1.000000000000000000, 0.9238795325112989509, 0.9999999999999877875 ) ) 
 REPRESENTATION_ITEM ( '' )  );
#19241 = CARTESIAN_POINT ( 'NONE',  ( 6.350852961086080661, -9.614813431917819062E-14, -139.8750000000000568 ) ) ;
#19242 = AXIS2_PLACEMENT_3D ( 'NONE', #24199, #14710, #3294 ) ;
#19243 = CARTESIAN_POINT ( 'NONE',  ( 0.000000000000000000, 0.000000000000000000, 0.000000000000000000 ) ) ;
#19244 = ORIENTED_EDGE ( 'NONE', *, *, #17740, .T. ) ;
#19245 = VECTOR ( 'NONE', #12698, 1000.000000000000000 ) ;
#19246 = CARTESIAN_POINT ( 'NONE',  ( -3.175426480542816066, 5.499999999999865885, -47.87500000000000000 ) ) ;
#19247 = CARTESIAN_POINT ( 'NONE',  ( -5.196152422706601826, 2.999999999999975131, -152.4613248654052029 ) ) ;
#19248 = ORIENTED_EDGE ( 'NONE', *, *, #15240, .F. ) ;
#19249 = CARTESIAN_POINT ( 'NONE',  ( 118.6872167782374703, 1.849990392679501827, 0.7662911109080090544 ) ) ;
#19250 = CARTESIAN_POINT ( 'NONE',  ( 6.000000000000000888, -1.859271017917181981E-14, -93.08632486540523132 ) ) ;
#19251 = CARTESIAN_POINT ( 'NONE',  ( 11.75000000000012079, 1.665334536937734811E-13, -2.000000000000057288 ) ) ;
#19252 = EDGE_CURVE ( 'NONE', #23786, #8065, #9844, .T. ) ;
#19253 = CARTESIAN_POINT ( 'NONE',  ( 7.216878364870455975, -6.409875621278545621E-14, -101.9419872981078328 ) ) ;
#19254 =( LENGTH_UNIT ( ) NAMED_UNIT ( * ) SI_UNIT ( .MILLI., .METRE. ) );
#19255 = CARTESIAN_POINT ( 'NONE',  ( 134.9062500000000284, 6.000000000000005329, -2.485281374238555774 ) ) ;
#19256 = CARTESIAN_POINT ( 'NONE',  ( 116.8749999999998863, 1.767766952966320915, -1.767766952966320915 ) ) ;
#19257 = EDGE_CURVE ( 'NONE', #18433, #16280, #21244, .T. ) ;
#19258 = CARTESIAN_POINT ( 'NONE',  ( -4.763139720814407951, 2.749999999999946709, -127.2500000000000284 ) ) ;
#19259 = EDGE_CURVE ( 'NONE', #23968, #20807, #230, .T. ) ;
#19260 = ORIENTED_EDGE ( 'NONE', *, *, #19661, .T. ) ;
#19261 = DIRECTION ( 'NONE',  ( 0.000000000000000000, 5.551115123125767911E-17, -1.000000000000000000 ) ) ;
#19262 = CARTESIAN_POINT ( 'NONE',  ( 0.000000000000000000, 5.499999999999991118, -54.00000000000004974 ) ) ;
#19263 = CARTESIAN_POINT ( 'NONE',  ( 21.96132486540530593, 1.665334536937734811E-13, 2.499999999999946709 ) ) ;
#19264 = CARTESIAN_POINT ( 'NONE',  ( -6.000000000000000888, 1.067854986875958443E-15, 7.560779664488942560E-35 ) ) ;
#19265 = CARTESIAN_POINT ( 'NONE',  ( -3.608439182435052128, -6.250000000000110134, -86.80801270189222407 ) ) ;
#19266 = UNCERTAINTY_MEASURE_WITH_UNIT (LENGTH_MEASURE( 1.000000000000000082E-05 ), #19158, 'distance_accuracy_value', 'NONE');
#19267 = DIRECTION ( 'NONE',  ( -7.147005652999508048E-36, 5.642372883946980038E-36, 1.000000000000000000 ) ) ;
#19268 = CARTESIAN_POINT ( 'NONE',  ( 152.6324251345948824, -5.500000000000012434, -2.278174593052012309 ) ) ;
#19269 = AXIS2_PLACEMENT_3D ( 'NONE', #8156, #3099, #8014 ) ;
#19270 = CARTESIAN_POINT ( 'NONE',  ( 107.6872167782374561, 1.849990392679562001, 0.7662911109080090544 ) ) ;
#19271 = CARTESIAN_POINT ( 'NONE',  ( -5.999999999999963585, 8.134310703387671600E-14, -114.8363248654052171 ) ) ;
#19272 = CARTESIAN_POINT ( 'NONE',  ( -3.464101615137725076, 5.999999999999979572, -61.08632486540521711 ) ) ;
#19273 = CARTESIAN_POINT ( 'NONE',  ( 114.5002832217623023, 1.308140751793696044, 1.308140751793640533 ) ) ;
#19274 =( BOUNDED_CURVE ( )  B_SPLINE_CURVE ( 2, ( #17976, #4105, #1805, #15841, #11210, #6406, #10593, #1657, #26989 ),
 .UNSPECIFIED., .F., .T. ) 
 B_SPLINE_CURVE_WITH_KNOTS ( ( 3, 2, 2, 2, 3 ),
 ( 0.7352941176470588758, 0.7426470588235294379, 0.7500000000000000000, 0.7573529411764705621, 0.7647058823529411242 ),
 .UNSPECIFIED. ) 
 CURVE ( )  GEOMETRIC_REPRESENTATION_ITEM ( )  RATIONAL_B_SPLINE_CURVE ( ( 1.000000000000000000, 0.9238795325112867385, 1.000000000000000000, 0.9238795325112867385, 1.000000000000000000, 0.9238795325112867385, 1.000000000000000000, 0.9238795325112867385, 1.000000000000000000 ) ) 
 REPRESENTATION_ITEM ( '' )  );
#19275 = CARTESIAN_POINT ( 'NONE',  ( 4.763139720814407951, -2.749999999999988454, -137.0000000000000000 ) ) ;
#19276 = CARTESIAN_POINT ( 'NONE',  ( 139.7755489643691078, -9.313758021888212113, 7.918536325242551577 ) ) ;
#19277 = CARTESIAN_POINT ( 'NONE',  ( 2.775557561562891351E-14, 6.250000000000033751, -151.9330127018922383 ) ) ;
#19278 = CARTESIAN_POINT ( 'NONE',  ( 10.00000000000012257, -0.6095397824213422133, -2.424553825687569830 ) ) ;
#19279 = CARTESIAN_POINT ( 'NONE',  ( 5.196152422706629359, -2.999999999999988898, -72.78867513459485394 ) ) ;
#19280 = CARTESIAN_POINT ( 'NONE',  ( 4.763139720814407951, 2.750000000000002665, -72.25000000000004263 ) ) ;
#19281 = CARTESIAN_POINT ( 'NONE',  ( -3.175426480542816510, 5.499999999999865885, -65.87500000000002842 ) ) ;
#19282 =( BOUNDED_CURVE ( )  B_SPLINE_CURVE ( 2, ( #6842, #14119, #23153, #82, #22992, #30346, #16268, #23457, #25586 ),
 .UNSPECIFIED., .F., .T. ) 
 B_SPLINE_CURVE_WITH_KNOTS ( ( 3, 2, 2, 2, 3 ),
 ( 0.7138888888888887951, 0.7148148148148147918, 0.7166666666666666741, 0.7185185185185185563, 0.7194444444444444420 ),
 .UNSPECIFIED. ) 
 CURVE ( )  GEOMETRIC_REPRESENTATION_ITEM ( )  RATIONAL_B_SPLINE_CURVE ( ( 0.9330127018922194093, 0.9330127018922154125, 1.000000000000000000, 0.8660254037844388186, 1.000000000000000000, 0.8660254037844388186, 1.000000000000000000, 0.9330127018922194093, 0.9330127018922194093 ) ) 
 REPRESENTATION_ITEM ( '' )  );
#19283 = CARTESIAN_POINT ( 'NONE',  ( 145.7961002691896510, 2.071067811865468400, -4.999999999999989342 ) ) ;
#19284 = CARTESIAN_POINT ( 'NONE',  ( 151.2187500000000000, 2.485281374238556218, -6.000000000000005329 ) ) ;
#19285 = FACE_OUTER_BOUND ( 'NONE', #23353, .T. ) ;
#19286 = ADVANCED_FACE ( 'NONE', ( #21240 ), #11450, .F. ) ;
#19287 = CARTESIAN_POINT ( 'NONE',  ( -6.000000000000000888, 1.067854986875958443E-15, 7.560779664488942560E-35 ) ) ;
#19288 = AXIS2_PLACEMENT_3D ( 'NONE', #16058, #19, #16505 ) ;
#19289 = EDGE_LOOP ( 'NONE', ( #25455, #19651, #29007, #9840, #9198, #29915, #10728, #26692 ) ) ;
#19290 = CARTESIAN_POINT ( 'NONE',  ( 149.5312500000000284, -2.485281374238555774, -6.000000000000005329 ) ) ;
#19291 = UNCERTAINTY_MEASURE_WITH_UNIT (LENGTH_MEASURE( 1.000000000000000082E-05 ), #16842, 'distance_accuracy_value', 'NONE');
#19292 = ADVANCED_FACE ( 'NONE', ( #9103 ), #16362, .F. ) ;
#19293 = CARTESIAN_POINT ( 'NONE',  ( 104.9580272744090479, -0.1377225354489101661, 1.978757841790981686 ) ) ;
#19294 = PRESENTATION_LAYER_ASSIGNMENT (  '', '', ( #28575 ) ) ;
#19295 = CARTESIAN_POINT ( 'NONE',  ( 2.775557561562891351E-14, 6.250000000000033751, -46.06698729810781856 ) ) ;
#19296 = CARTESIAN_POINT ( 'NONE',  ( 22.31250000000003197, -0.8284271247460553989, 2.000000000000031530 ) ) ;
#19297 = ORIENTED_EDGE ( 'NONE', *, *, #14420, .T. ) ;
#19298 = CARTESIAN_POINT ( 'NONE',  ( 4.763139720814407951, 2.750000000000002665, -78.25000000000004263 ) ) ;
#19299 = CARTESIAN_POINT ( 'NONE',  ( -5.412658773652739619, 3.124999999999975131, -100.6830127018922241 ) ) ;
#19300 = VERTEX_POINT ( 'NONE', #25683 ) ;
#19301 = CARTESIAN_POINT ( 'NONE',  ( 124.9999999999999432, -70.00000000000000000, -5.000000000000004441 ) ) ;
#19302 = CARTESIAN_POINT ( 'NONE',  ( 3.175426480543072749, -5.500000000000105693, -168.6250000000000000 ) ) ;
#19303 = CARTESIAN_POINT ( 'NONE',  ( 104.8415063509460055, -1.908493649053821795, 1.110223024625156540E-13 ) ) ;
#19304 = CARTESIAN_POINT ( 'NONE',  ( 0.000000000000000000, 0.000000000000000000, 0.000000000000000000 ) ) ;
#19305 = CARTESIAN_POINT ( 'NONE',  ( -5.196152422706573404, -3.000000000000002665, -59.21132486540525974 ) ) ;
#19306 = CONICAL_SURFACE ( 'NONE', #6037, 2.499999999999999112, 0.7853981633974522758 ) ;
#19307 = CARTESIAN_POINT ( 'NONE',  ( 4.763139720814407951, -2.749999999999988454, -162.5000000000000284 ) ) ;
#19308 = CARTESIAN_POINT ( 'NONE',  ( 17.03867513459494987, 1.665334536937734811E-13, -2.500000000000002220 ) ) ;
#19309 = CARTESIAN_POINT ( 'NONE',  ( -4.763139720814407951, -2.750000000000016431, -154.0000000000000284 ) ) ;
#19310 = VECTOR ( 'NONE', #12910, 1000.000000000000000 ) ;
#19311 = CARTESIAN_POINT ( 'NONE',  ( -5.999999999999963585, -1.487416814333745711E-14, -76.41367513459481131 ) ) ;
#19312 = CARTESIAN_POINT ( 'NONE',  ( 149.3363248654052029, 0.000000000000000000, -5.500000000000005329 ) ) ;
#19313 = CARTESIAN_POINT ( 'NONE',  ( 0.000000000000000000, 5.499999999999991118, -93.00000000000002842 ) ) ;
#19314 = CARTESIAN_POINT ( 'NONE',  ( 0.000000000000000000, 5.999999999999977796, -125.7113248654052597 ) ) ;
#19315 = CARTESIAN_POINT ( 'NONE',  ( 115.5386751345946408, 1.387778780781445676E-13, 2.000000000000112799 ) ) ;
#19316 = CARTESIAN_POINT ( 'NONE',  ( 6.350852961086080661, -9.614813431917819062E-14, -93.37500000000001421 ) ) ;
#19317 = CARTESIAN_POINT ( 'NONE',  ( 158.2648502691896510, 3.535533905932725318, 3.535533905932752852 ) ) ;
#19318 = CARTESIAN_POINT ( 'NONE',  ( 109.3363248654050182, -1.414213562373034527, -1.414213562373034527 ) ) ;
#19319 =( BOUNDED_CURVE ( )  B_SPLINE_CURVE ( 2, ( #25977, #14350, #23690, #17495, #16803, #17808, #24680, #23835, #3320 ),
 .UNSPECIFIED., .F., .F. ) 
 B_SPLINE_CURVE_WITH_KNOTS ( ( 3, 2, 2, 2, 3 ),
 ( 0.6083333333333333925, 0.6092592592592592782, 0.6111111111111111605, 0.6129629629629629317, 0.6138888888888888173 ),
 .UNSPECIFIED. ) 
 CURVE ( )  GEOMETRIC_REPRESENTATION_ITEM ( )  RATIONAL_B_SPLINE_CURVE ( ( 0.9330127018922194093, 0.9330127018922234061, 1.000000000000000000, 0.8660254037844388186, 1.000000000000000000, 0.8660254037844388186, 1.000000000000000000, 0.9330127018922234061, 0.9330127018922194093 ) ) 
 REPRESENTATION_ITEM ( '' )  );
#19320 = CARTESIAN_POINT ( 'NONE',  ( 9.250000000000092371, -1.873492889144789952, -1.873492889145123019 ) ) ;
#19321 = CARTESIAN_POINT ( 'NONE',  ( 112.8749999999998437, 1.767766952966320915, -1.767766952966320915 ) ) ;
#19322 = DIRECTION ( 'NONE',  ( -7.147005652999508048E-36, 5.642372883946980038E-36, 1.000000000000000000 ) ) ;
#19323 = ADVANCED_FACE ( 'NONE', ( #11748 ), #15559, .F. ) ;
#19324 = CARTESIAN_POINT ( 'NONE',  ( -15.49999999999999289, -54.99999999999990763, 8.000000000000007105 ) ) ;
#19325 = EDGE_CURVE ( 'NONE', #7800, #17999, #10108, .T. ) ;
#19326 = ORIENTED_EDGE ( 'NONE', *, *, #27497, .F. ) ;
#19327 = LINE ( 'NONE', #26357, #4801 ) ;
#19328 = DIRECTION ( 'NONE',  ( -7.147005652999508048E-36, 5.642372883946980038E-36, 1.000000000000000000 ) ) ;
#19329 = CARTESIAN_POINT ( 'NONE',  ( 104.8747167782376550, -2.775557561562891351E-14, 1.849990392679523588 ) ) ;
#19330 = VERTEX_POINT ( 'NONE', #7094 ) ;
#19331 = CIRCLE ( 'NONE', #23268, 1.000000000000000000 ) ;
#19332 = ORIENTED_EDGE ( 'NONE', *, *, #24184, .F. ) ;
#19333 =( GEOMETRIC_REPRESENTATION_CONTEXT ( 3 ) GLOBAL_UNCERTAINTY_ASSIGNED_CONTEXT ( ( #17714 ) ) GLOBAL_UNIT_ASSIGNED_CONTEXT ( ( #17303, #29965, #12550 ) ) REPRESENTATION_CONTEXT ( 'NONE', 'WORKASPACE' ) );
#19334 = ORIENTED_EDGE ( 'NONE', *, *, #8046, .F. ) ;
#19335 = CARTESIAN_POINT ( 'NONE',  ( 4.763139720814407951, -2.749999999999988454, -107.0000000000000426 ) ) ;
#19336 = CARTESIAN_POINT ( 'NONE',  ( 19.37500000000017053, 2.649519052838444910, 0.000000000000000000 ) ) ;
#19337 = CARTESIAN_POINT ( 'NONE',  ( 5.412658773652712085, -3.125000000000086153, -123.9330127018922809 ) ) ;
#19338 = EDGE_LOOP ( 'NONE', ( #15959, #4945, #20698, #4068 ) ) ;
#19339 = DIRECTION ( 'NONE',  ( 1.000000000000000000, -5.551115123125773458E-17, -1.260129944081490338E-35 ) ) ;
#19340 = CARTESIAN_POINT ( 'NONE',  ( -5.412658773652739619, 3.124999999999975131, -158.3169872981078470 ) ) ;
#19341 = CARTESIAN_POINT ( 'NONE',  ( 107.3749999999999574, -1.767766952966293159, 1.767766952966431937 ) ) ;
#19342 = CARTESIAN_POINT ( 'NONE',  ( 133.6726497308104058, -5.000000000000004441, 0.000000000000000000 ) ) ;
#19343 = CARTESIAN_POINT ( 'NONE',  ( 2.775557561562891351E-14, 6.250000000000033751, -60.43301270189227381 ) ) ;
#19344 = VERTEX_POINT ( 'NONE', #23550 ) ;
#19345 = CYLINDRICAL_SURFACE ( 'NONE', #21109, 0.5000000000000004441 ) ;
#19346 = CARTESIAN_POINT ( 'NONE',  ( 3.464101615137757051, -5.999999999999979572, -132.3363248654052313 ) ) ;
#19347 = CARTESIAN_POINT ( 'NONE',  ( 141.6488248654052029, -3.889087296526011706, -3.889087296526011706 ) ) ;
#19348 = CARTESIAN_POINT ( 'NONE',  ( 6.350852961086080661, -9.614813431917819062E-14, -180.3750000000000284 ) ) ;
#19349 = CARTESIAN_POINT ( 'NONE',  ( 119.4374999999997868, -2.499999999999994671, 1.035533905932809473 ) ) ;
#19350 = CARTESIAN_POINT ( 'NONE',  ( -5.999999999999963585, 1.780251999655701777E-13, -99.83632486540521711 ) ) ;
#19351 = CARTESIAN_POINT ( 'NONE',  ( 3.608439182435180470, 6.249999999999982236, -180.5580127018922383 ) ) ;
#19352 = CARTESIAN_POINT ( 'NONE',  ( 5.196152422706629359, -2.999999999999988898, -101.2886751345948255 ) ) ;
#19353 = CARTESIAN_POINT ( 'NONE',  ( 4.763139720814407951, 2.750000000000002665, -114.2500000000000142 ) ) ;
#19354 = CARTESIAN_POINT ( 'NONE',  ( 135.1170067730392361, -7.914203246654652801, 8.323901939971086961 ) ) ;
#19355 = CARTESIAN_POINT ( 'NONE',  ( -4.763139720814407951, 2.749999999999946709, -112.2500000000000142 ) ) ;
#19356 = PRESENTATION_STYLE_ASSIGNMENT (( #29984 ) ) ;
#19357 = CARTESIAN_POINT ( 'NONE',  ( 16.02382486540522777, -1.035533905932629173, 2.499999999999964473 ) ) ;
#19358 = CARTESIAN_POINT ( 'NONE',  ( 149.1636751345948255, 0.000000000000000000, 5.500000000000005329 ) ) ;
#19359 = ORIENTED_EDGE ( 'NONE', *, *, #4238, .T. ) ;
#19360 = CARTESIAN_POINT ( 'NONE',  ( 0.07046192191372500913, -16.32887961881856853, 6.302507423776497752 ) ) ;
#19361 = CARTESIAN_POINT ( 'NONE',  ( -5.999999999999963585, -1.487416814333745711E-14, -167.9136751345948255 ) ) ;
#19362 = CIRCLE ( 'NONE', #6084, 1.999999999999998224 ) ;
#19363 = EDGE_CURVE ( 'NONE', #6339, #29963, #5686, .T. ) ;
#19364 = ORIENTED_EDGE ( 'NONE', *, *, #9114, .F. ) ;
#19365 = CARTESIAN_POINT ( 'NONE',  ( 3.175426480543072749, -5.500000000000105693, -176.1250000000000284 ) ) ;
#19366 = CARTESIAN_POINT ( 'NONE',  ( 22.46132486540528106, 1.665334536937734811E-13, -2.500000000000113243 ) ) ;
#19367 = VERTEX_POINT ( 'NONE', #10169 ) ;
#19368 = CARTESIAN_POINT ( 'NONE',  ( 22.41367513459485750, 1.767766952966598470, 1.767766952966376426 ) ) ;
#19369 =( BOUNDED_CURVE ( )  B_SPLINE_CURVE ( 2, ( #11603, #6794, #22788, #20945, #1730, #2199, #16217, #25216, #8811 ),
 .UNSPECIFIED., .F., .T. ) 
 B_SPLINE_CURVE_WITH_KNOTS ( ( 3, 2, 2, 2, 3 ),
 ( 0.5749999999999999556, 0.5759259259259259522, 0.5777777777777777235, 0.5796296296296296058, 0.5805555555555554914 ),
 .UNSPECIFIED. ) 
 CURVE ( )  GEOMETRIC_REPRESENTATION_ITEM ( )  RATIONAL_B_SPLINE_CURVE ( ( 0.9330127018922194093, 0.9330127018922154125, 1.000000000000000000, 0.8660254037844388186, 1.000000000000000000, 0.8660254037844388186, 1.000000000000000000, 0.9330127018922234061, 0.9330127018922194093 ) ) 
 REPRESENTATION_ITEM ( '' )  );
#19370 = ORIENTED_EDGE ( 'NONE', *, *, #23211, .F. ) ;
#19371 = ORIENTED_EDGE ( 'NONE', *, *, #16274, .F. ) ;
#19372 = DIRECTION ( 'NONE',  ( 0.000000000000000000, 0.000000000000000000, 1.000000000000000000 ) ) ;
#19373 = CARTESIAN_POINT ( 'NONE',  ( 134.3586002691896510, 2.071067811865468400, 4.999999999999989342 ) ) ;
#19374 = CARTESIAN_POINT ( 'NONE',  ( 3.608439182435180470, 6.249999999999982236, -134.6919872981078470 ) ) ;
#19375 = FACE_OUTER_BOUND ( 'NONE', #14481, .T. ) ;
#19376 = CARTESIAN_POINT ( 'NONE',  ( -5.999999999999919176, 1.607695154586804565, -83.40331216351300725 ) ) ;
#19377 = CARTESIAN_POINT ( 'NONE',  ( 161.0000000000000284, 0.000000000000000000, 0.000000000000000000 ) ) ;
#19378 = AXIS2_PLACEMENT_3D ( 'NONE', #8615, #11098, #10953 ) ;
#19379 = ORIENTED_EDGE ( 'NONE', *, *, #26197, .F. ) ;
#19380 = CARTESIAN_POINT ( 'NONE',  ( 20.56250000000014566, -1.999999999999911626, -0.8284271247462354770 ) ) ;
#19381 = CYLINDRICAL_SURFACE ( 'NONE', #20108, 6.000000000000000888 ) ;
#19382 = CARTESIAN_POINT ( 'NONE',  ( 149.5386751345948539, -5.500000000000005329, 0.000000000000000000 ) ) ;
#19383 = CARTESIAN_POINT ( 'NONE',  ( 137.8913997308104058, -2.071067811865468400, 4.999999999999989342 ) ) ;
#19384 = DIRECTION ( 'NONE',  ( -7.147005652999508048E-36, 5.642372883946980038E-36, 1.000000000000000000 ) ) ;
#19385 = CARTESIAN_POINT ( 'NONE',  ( 6.000000000000000888, 7.762456499804234384E-14, -139.5863248654051745 ) ) ;
#19386 = EDGE_CURVE ( 'NONE', #30081, #10990, #9866, .T. ) ;
#19387 = CARTESIAN_POINT ( 'NONE',  ( -3.464101615137757051, -5.999999999999979572, -162.5863248654052313 ) ) ;
#19388 = CARTESIAN_POINT ( 'NONE',  ( 6.000000000000052403, -1.607695154586662678, -69.15331216351300725 ) ) ;
#19389 = CARTESIAN_POINT ( 'NONE',  ( 106.9374999999998010, 2.500000000000054623, -1.035533905932568999 ) ) ;
#19390 = CARTESIAN_POINT ( 'NONE',  ( -5.999999999999963585, -1.487416814333745711E-14, -143.3363248654052029 ) ) ;
#19391 = CARTESIAN_POINT ( 'NONE',  ( -4.763139720814407951, -2.750000000000016431, -136.0000000000000000 ) ) ;
#19392 = CARTESIAN_POINT ( 'NONE',  ( 108.3988248654050324, -0.8284271247460250898, -1.999999999999851674 ) ) ;
#19393 = CARTESIAN_POINT ( 'NONE',  ( 104.7401757384974275, 1.755445637970139305, -0.5961972863698411507 ) ) ;
#19394 = ORIENTED_EDGE ( 'NONE', *, *, #16912, .T. ) ;
#19395 = VECTOR ( 'NONE', #17462, 1000.000000000000000 ) ;
#19396 = AXIS2_PLACEMENT_3D ( 'NONE', #11641, #30027, #11489 ) ;
#19397 = CARTESIAN_POINT ( 'NONE',  ( 108.2261751345945129, 2.000000000000061728, -0.8284271247460553989 ) ) ;
#19398 = CARTESIAN_POINT ( 'NONE',  ( 153.3675748654052597, -5.500000000000012434, 2.278174593052012309 ) ) ;
#19399 = EDGE_CURVE ( 'NONE', #28019, #87, #19979, .T. ) ;
#19400 = ORIENTED_EDGE ( 'NONE', *, *, #11894, .T. ) ;
#19401 = CARTESIAN_POINT ( 'NONE',  ( 117.0622167782374561, -1.849990392679472073, 0.7662911109078888172 ) ) ;
#19402 = DIRECTION ( 'NONE',  ( 0.000000000000000000, 0.000000000000000000, 1.000000000000000000 ) ) ;
#19403 = CARTESIAN_POINT ( 'NONE',  ( -7.216878364870328078, 0.000000000000000000, -93.69198729810780435 ) ) ;
#19404 = CARTESIAN_POINT ( 'NONE',  ( 3.464101615137852974, 5.999999999999884537, -172.9136751345947971 ) ) ;
#19405 = CARTESIAN_POINT ( 'NONE',  ( 117.4374999999997584, -2.499999999999844569, 1.035533905932929599 ) ) ;
#19406 = VECTOR ( 'NONE', #16783, 1000.000000000000000 ) ;
#19407 = DIRECTION ( 'NONE',  ( 1.000000000000000000, -5.551115123125773458E-17, -1.260129944081490338E-35 ) ) ;
#19408 = CARTESIAN_POINT ( 'NONE',  ( -6.350852961085760029, -1.281975124255709124E-13, -127.1249999999999858 ) ) ;
#19409 = ORIENTED_EDGE ( 'NONE', *, *, #24974, .T. ) ;
#19410 = CARTESIAN_POINT ( 'NONE',  ( -5.999999999999963585, 1.780251999655701777E-13, -95.91367513459483973 ) ) ;
#19411 = AXIS2_PLACEMENT_3D ( 'NONE', #8690, #16255, #30334 ) ;
#19412 = CARTESIAN_POINT ( 'NONE',  ( 0.000000000000000000, 5.499999999999991118, -57.00000000000004974 ) ) ;
#19413 =( BOUNDED_CURVE ( )  B_SPLINE_CURVE ( 2, ( #17992, #3656, #24713, #11068, #8588, #18292, #13092, #15857, #4277 ),
 .UNSPECIFIED., .F., .F. ) 
 B_SPLINE_CURVE_WITH_KNOTS ( ( 3, 2, 2, 2, 3 ),
 ( 0.08055555555555549141, 0.08148148148148148806, 0.08333333333333337034, 0.08518518518518514160, 0.08611111111111113825 ),
 .UNSPECIFIED. ) 
 CURVE ( )  GEOMETRIC_REPRESENTATION_ITEM ( )  RATIONAL_B_SPLINE_CURVE ( ( 0.9330127018922194093, 0.9330127018922154125, 1.000000000000000000, 0.8660254037844388186, 1.000000000000000000, 0.8660254037844388186, 1.000000000000000000, 0.9330127018922154125, 0.9330127018922194093 ) ) 
 REPRESENTATION_ITEM ( '' )  );
#19414 = CARTESIAN_POINT ( 'NONE',  ( 5.196152422706629359, 3.000000000000002665, -116.0386751345948113 ) ) ;
#19415 = CARTESIAN_POINT ( 'NONE',  ( 5.999999999999949374, 1.607695154586804565, -66.59668783648703538 ) ) ;
#19416 = CARTESIAN_POINT ( 'NONE',  ( -3.464101615137725076, 5.999999999999979572, -67.66367513459479710 ) ) ;
#19417 = CARTESIAN_POINT ( 'NONE',  ( -3.608439182435115633, 6.249999999999965361, -82.80801270189226670 ) ) ;
#19418 = CARTESIAN_POINT ( 'NONE',  ( -4.999999999999990230, -14.50000000000001243, 7.500000000000007105 ) ) ;
#19419 = ADVANCED_FACE ( 'NONE', ( #2163 ), #11873, .T. ) ;
#19420 = CARTESIAN_POINT ( 'NONE',  ( 6.000000000000000000, 2.951592740943527306E-14, -153.6636751345948539 ) ) ;
#19421 = CARTESIAN_POINT ( 'NONE',  ( 140.6985356443576620, -11.69853564435973503, -4.029618091915715183 ) ) ;
#19422 = CARTESIAN_POINT ( 'NONE',  ( 0.000000000000000000, 0.000000000000000000, -180.0000000000000568 ) ) ;
#19423 = CARTESIAN_POINT ( 'NONE',  ( 115.0627832217623592, -0.7662911109076785410, -1.849990392679171425 ) ) ;
#19424 = CARTESIAN_POINT ( 'NONE',  ( 6.350852961086080661, -9.614813431917819062E-14, -142.8750000000000568 ) ) ;
#19425 = CARTESIAN_POINT ( 'NONE',  ( 139.5759038609257061, -9.165151425709554545, 8.000000000000007105 ) ) ;
#19426 = CARTESIAN_POINT ( 'NONE',  ( 5.412658773652712085, -3.125000000000086153, -156.9330127018922383 ) ) ;
#19427 = CARTESIAN_POINT ( 'NONE',  ( -5.196152422706573404, -3.000000000000002665, -71.21132486540521711 ) ) ;
#19428 = CARTESIAN_POINT ( 'NONE',  ( -5.999999999999971578, 1.607695154586715303, -66.90331216351303567 ) ) ;
#19429 = CARTESIAN_POINT ( 'NONE',  ( 6.350852961086080661, -9.614813431917819062E-14, -69.37500000000004263 ) ) ;
#19430 = EDGE_CURVE ( 'NONE', #10447, #3203, #23576, .T. ) ;
#19431 = CARTESIAN_POINT ( 'NONE',  ( -6.350852961085760029, -1.281975124255709124E-13, -56.62500000000004974 ) ) ;
#19432 = EDGE_CURVE ( 'NONE', #13422, #15655, #8861, .T. ) ;
#19433 = CYLINDRICAL_SURFACE ( 'NONE', #28273, 17.50000000000000355 ) ;
#19434 = CARTESIAN_POINT ( 'NONE',  ( 146.4523502691896510, 0.000000000000000000, 5.000000000000004441 ) ) ;
#19435 = CARTESIAN_POINT ( 'NONE',  ( 149.7187500000000284, 2.485281374238556218, -6.000000000000005329 ) ) ;
#19436 = CARTESIAN_POINT ( 'NONE',  ( 6.000000000000000888, -1.859271017917181981E-14, -59.16367513459483263 ) ) ;
#19437 = CARTESIAN_POINT ( 'NONE',  ( 17.43750000000012790, -1.999999999999851674, 0.8284271247463557142 ) ) ;
#19438 = VECTOR ( 'NONE', #11958, 1000.000000000000000 ) ;
#19439 = CARTESIAN_POINT ( 'NONE',  ( 6.000000000000052403, -1.607695154586662678, -104.2306624327026299 ) ) ;
#19440 = CARTESIAN_POINT ( 'NONE',  ( 114.6872167782375982, 1.849990392679621953, 0.7662911109080090544 ) ) ;
#19441 =( NAMED_UNIT ( * ) SI_UNIT ( $, .STERADIAN. ) SOLID_ANGLE_UNIT ( ) );
#19442 = ORIENTED_EDGE ( 'NONE', *, *, #5382, .F. ) ;
#19443 = CARTESIAN_POINT ( 'NONE',  ( 142.1250000000000284, 0.000000000000000000, -6.000000000000005329 ) ) ;
#19444 = CARTESIAN_POINT ( 'NONE',  ( 22.62500000000017408, -1.414213562372867994, -1.414213562373034527 ) ) ;
#19445 = COLOUR_RGB ( '', 0.66274510, 0.83137255, 0.94901961) ;
#19446 = ORIENTED_EDGE ( 'NONE', *, *, #13878, .T. ) ;
#19447 = CARTESIAN_POINT ( 'NONE',  ( 4.763139720814407951, -2.749999999999988454, -83.00000000000001421 ) ) ;
#19448 =( BOUNDED_CURVE ( )  B_SPLINE_CURVE ( 2, ( #8785, #13574, #6619, #16040, #13731, #14041, #14190, #18778, #163 ),
 .UNSPECIFIED., .F., .T. ) 
 B_SPLINE_CURVE_WITH_KNOTS ( ( 3, 2, 2, 2, 3 ),
 ( 0.4117647058823529216, 0.4191176470588235392, 0.4264705882352941013, 0.4338235294117647189, 0.4411764705882352811 ),
 .UNSPECIFIED. ) 
 CURVE ( )  GEOMETRIC_REPRESENTATION_ITEM ( )  RATIONAL_B_SPLINE_CURVE ( ( 1.000000000000000000, 0.9238795325112867385, 1.000000000000000000, 0.9238795325112867385, 1.000000000000000000, 0.9238795325112867385, 1.000000000000000000, 0.9238795325112867385, 1.000000000000000000 ) ) 
 REPRESENTATION_ITEM ( '' )  );
#19449 = ORIENTED_EDGE ( 'NONE', *, *, #8508, .T. ) ;
#19450 = CARTESIAN_POINT ( 'NONE',  ( 6.000000000000000888, -1.607695154586752384, -127.6533121635130215 ) ) ;
#19451 = VECTOR ( 'NONE', #14893, 1000.000000000000000 ) ;
#19452 = EDGE_CURVE ( 'NONE', #4894, #29768, #10850, .T. ) ;
#19453 = FACE_OUTER_BOUND ( 'NONE', #10016, .T. ) ;
#19454 = CARTESIAN_POINT ( 'NONE',  ( 1.384933631640856255, -10.91424797897491139, -19.15860252534411146 ) ) ;
#19455 = CARTESIAN_POINT ( 'NONE',  ( 135.1084928141470414, -8.790281914036096822, 8.000000000000007105 ) ) ;
#19456 =( LENGTH_UNIT ( ) NAMED_UNIT ( * ) SI_UNIT ( .MILLI., .METRE. ) );
#19457 = CARTESIAN_POINT ( 'NONE',  ( 3.175426480543072749, 5.499999999999865885, -163.6249999999999716 ) ) ;
#19458 = CARTESIAN_POINT ( 'NONE',  ( -5.196152422706573404, -3.000000000000002665, -60.71132486540520290 ) ) ;
#19459 = CARTESIAN_POINT ( 'NONE',  ( 3.175426480543072749, 5.499999999999865885, -150.1250000000000284 ) ) ;
#19460 = CARTESIAN_POINT ( 'NONE',  ( 117.2886751345947971, 2.000000000000140332, 2.220446049250313081E-13 ) ) ;
#19461 = CARTESIAN_POINT ( 'NONE',  ( 3.175426480543072749, -5.500000000000105693, -93.62500000000002842 ) ) ;
#19462 = CARTESIAN_POINT ( 'NONE',  ( 115.7886751345947118, -1.999999999999974021, 0.000000000000000000 ) ) ;
#19463 = EDGE_CURVE ( 'NONE', #3196, #22419, #3347, .T. ) ;
#19464 = CARTESIAN_POINT ( 'NONE',  ( 0.000000000000000000, 5.499999999999991118, -91.50000000000002842 ) ) ;
#19465 = CARTESIAN_POINT ( 'NONE',  ( 157.2336002691896226, -4.999999999999989342, 2.071067811865468400 ) ) ;
#19466 = CYLINDRICAL_SURFACE ( 'NONE', #4722, 6.000000000000000888 ) ;
#19467 = CARTESIAN_POINT ( 'NONE',  ( 24.43750000000014921, -1.999999999999851674, 0.8284271247462354770 ) ) ;
#19468 = CARTESIAN_POINT ( 'NONE',  ( 108.6249999999999289, -1.767766952966320915, -1.767766952966320915 ) ) ;
#19469 = CARTESIAN_POINT ( 'NONE',  ( -5.196152422706573404, -3.000000000000002665, -66.71132486540520290 ) ) ;
#19470 = CARTESIAN_POINT ( 'NONE',  ( -5.196152422706573404, -3.000000000000002665, -74.21132486540521711 ) ) ;
#19471 = CARTESIAN_POINT ( 'NONE',  ( -4.999999999999879208, -71.00000000000002842, 5.000000000000004441 ) ) ;
#19472 = ORIENTED_EDGE ( 'NONE', *, *, #20556, .T. ) ;
#19473 = LINE ( 'NONE', #718, #10716 ) ;
#19474 = CARTESIAN_POINT ( 'NONE',  ( 0.000000000000000000, 5.999999999999977796, -82.78867513459481131 ) ) ;
#19475 = CARTESIAN_POINT ( 'NONE',  ( 119.1252832217622597, -5.551115123125782702E-14, -1.849990392679412565 ) ) ;
#19476 = ORIENTED_EDGE ( 'NONE', *, *, #9715, .T. ) ;
#19477 = ORIENTED_EDGE ( 'NONE', *, *, #13341, .T. ) ;
#19478 = CARTESIAN_POINT ( 'NONE',  ( -4.763139720814407951, -2.750000000000016431, -103.0000000000000426 ) ) ;
#19479 = CARTESIAN_POINT ( 'NONE',  ( 19.68750000000009948, -1.097466725451499370, 2.649519052838238409 ) ) ;
#19480 = CARTESIAN_POINT ( 'NONE',  ( 7.216878364870455975, -6.409875621278545621E-14, -119.3080127018922525 ) ) ;
#19481 = ORIENTED_EDGE ( 'NONE', *, *, #9213, .F. ) ;
#19482 = CARTESIAN_POINT ( 'NONE',  ( 6.350852961086080661, -9.614813431917819062E-14, -151.8749999999999716 ) ) ;
#19483 = CARTESIAN_POINT ( 'NONE',  ( -9.999999999999793943, 10.00000000000000888, -3.000000000000002665 ) ) ;
#19484 = CARTESIAN_POINT ( 'NONE',  ( 2.775557561562891351E-14, -6.250000000000061284, -160.8169872981078470 ) ) ;
#19485 = CARTESIAN_POINT ( 'NONE',  ( 105.0624999999998437, 2.500000000000055067, 1.035533905932869425 ) ) ;
#19486 = AXIS2_PLACEMENT_3D ( 'NONE', #19550, #22150, #21850 ) ;
#19487 = CARTESIAN_POINT ( 'NONE',  ( 132.0788997308104058, -4.999999999999989342, 2.071067811865468400 ) ) ;
#19488 = EDGE_CURVE ( 'NONE', #1706, #28330, #296, .T. ) ;
#19489 = CARTESIAN_POINT ( 'NONE',  ( 7.216878364870455975, -6.409875621278545621E-14, -56.30801270189227381 ) ) ;
#19490 = ORIENTED_EDGE ( 'NONE', *, *, #16877, .F. ) ;
#19491 = CARTESIAN_POINT ( 'NONE',  ( 0.8055949159889823630, -15.44753772930997116, -8.223435417591852925 ) ) ;
#19492 = EDGE_CURVE ( 'NONE', #9960, #22916, #13925, .T. ) ;
#19493 = CARTESIAN_POINT ( 'NONE',  ( -5.990257846049534152, 9.225907948257358271, -24.60347258678507743 ) ) ;
#19494 = CARTESIAN_POINT ( 'NONE',  ( 6.350852961086080661, -9.614813431917819062E-14, -168.3750000000000568 ) ) ;
#19495 = CARTESIAN_POINT ( 'NONE',  ( 118.4999999999998437, -2.499999999999919176, 0.000000000000000000 ) ) ;
#19496 = CARTESIAN_POINT ( 'NONE',  ( 6.000000000000052403, -1.607695154586662678, -112.6533121635129930 ) ) ;
#19497 = CARTESIAN_POINT ( 'NONE',  ( 3.608439182435180470, -6.249999999999997335, -167.5580127018922099 ) ) ;
#19498 = DIRECTION ( 'NONE',  ( 0.000000000000000000, 0.4000000000000005773, -0.9165151389911678770 ) ) ;
#19499 = CARTESIAN_POINT ( 'NONE',  ( 23.18750000000004974, 0.8284271247462955401, 1.999999999999851674 ) ) ;
#19500 = CARTESIAN_POINT ( 'NONE',  ( 3.175426480543072749, -5.500000000000105693, -119.1250000000000284 ) ) ;
#19501 = CARTESIAN_POINT ( 'NONE',  ( 3.175426480543072749, 5.499999999999865885, -115.6250000000000142 ) ) ;
#19502 =( NAMED_UNIT ( * ) PLANE_ANGLE_UNIT ( ) SI_UNIT ( $, .RADIAN. ) );
#19503 = CIRCLE ( 'NONE', #20975, 6.000000000000009770 ) ;
#19504 = DIRECTION ( 'NONE',  ( 1.000000000000000000, 0.000000000000000000, 0.000000000000000000 ) ) ;
#19505 = ORIENTED_EDGE ( 'NONE', *, *, #2756, .F. ) ;
#19506 = CARTESIAN_POINT ( 'NONE',  ( 16.87500000000011369, 1.110223024625156540E-13, 2.649519052838333888 ) ) ;
#19507 = CARTESIAN_POINT ( 'NONE',  ( 119.8124999999998863, 1.035533905932839449, -2.499999999999844569 ) ) ;
#19508 = CARTESIAN_POINT ( 'NONE',  ( -5.999999999999963585, 1.780251999655701777E-13, -108.8363248654052313 ) ) ;
#19509 = TOROIDAL_SURFACE ( 'NONE', #10681, 16.00000000000000000, 1.000000000000000000 ) ;
#19510 = CARTESIAN_POINT ( 'NONE',  ( -5.999999999999963585, 1.780251999655701777E-13, -86.33632486540524553 ) ) ;
#19511 = VERTEX_POINT ( 'NONE', #4301 ) ;
#19512 = PRESENTATION_STYLE_ASSIGNMENT (( #7224 ) ) ;
#19513 = CARTESIAN_POINT ( 'NONE',  ( 3.175426480543072749, -5.500000000000105693, -179.1250000000000568 ) ) ;
#19514 = CARTESIAN_POINT ( 'NONE',  ( -5.412658773652739619, 3.124999999999975131, -81.81698729810781856 ) ) ;
#19515 = ORIENTED_EDGE ( 'NONE', *, *, #25685, .T. ) ;
#19516 = CARTESIAN_POINT ( 'NONE',  ( -3.464101615137725076, 5.999999999999979572, -144.1636751345948255 ) ) ;
#19517 = VECTOR ( 'NONE', #29485, 1000.000000000000000 ) ;
#19518 = VERTEX_POINT ( 'NONE', #5340 ) ;
#19519 = VERTEX_POINT ( 'NONE', #17061 ) ;
#19520 = CARTESIAN_POINT ( 'NONE',  ( -5.196152422706601826, 2.999999999999975131, -84.96132486540520290 ) ) ;
#19521 = CARTESIAN_POINT ( 'NONE',  ( 134.0773502691896510, 5.000000000000004441, 0.000000000000000000 ) ) ;
#19522 = ORIENTED_EDGE ( 'NONE', *, *, #6016, .F. ) ;
#19523 = CARTESIAN_POINT ( 'NONE',  ( -5.412658773652739619, 3.124999999999975131, -132.8169872981078186 ) ) ;
#19524 = CARTESIAN_POINT ( 'NONE',  ( 3.464101615137852974, 5.999999999999884537, -49.91367513459485394 ) ) ;
#19525 = DIRECTION ( 'NONE',  ( 1.000000000000000000, -0.000000000000000000, -0.000000000000000000 ) ) ;
#19526 = ORIENTED_EDGE ( 'NONE', *, *, #7096, .F. ) ;
#19527 = CIRCLE ( 'NONE', #3796, 1.000000000000000000 ) ;
#19528 = CARTESIAN_POINT ( 'NONE',  ( 14.18749999999996270, 0.8284271247462955401, 2.000000000000031530 ) ) ;
#19529 = CARTESIAN_POINT ( 'NONE',  ( -5.999999999999956479, -1.607695154586745057, -139.3466878364870638 ) ) ;
#19530 = EDGE_CURVE ( 'NONE', #22297, #13381, #7952, .T. ) ;
#19531 = CARTESIAN_POINT ( 'NONE',  ( 116.0000000000000142, 0.000000000000000000, 0.000000000000000000 ) ) ;
#19532 = CARTESIAN_POINT ( 'NONE',  ( 136.8601497308104058, -3.535533905932725318, -3.535533905932725318 ) ) ;
#19533 = DIRECTION ( 'NONE',  ( -1.000000000000000000, -1.665334536937736783E-16, -2.220446049250315546E-16 ) ) ;
#19534 = LINE ( 'NONE', #10010, #1118 ) ;
#19535 = CARTESIAN_POINT ( 'NONE',  ( 107.8749999999999858, 1.767766952966431937, -1.767766952966209892 ) ) ;
#19536 = CARTESIAN_POINT ( 'NONE',  ( 107.3363248654051887, -1.414213562373034527, -1.414213562373034527 ) ) ;
#19537 = CARTESIAN_POINT ( 'NONE',  ( -2.775557561562891351E-14, -5.500000000000115463, -138.7500000000000284 ) ) ;
#19539 = CARTESIAN_POINT ( 'NONE',  ( 0.000000000000000000, 5.999999999999977796, -166.7886751345948255 ) ) ;
#19538 = AXIS2_PLACEMENT_3D ( 'NONE', #16888, #16742, #26067 ) ;
#19540 = ORIENTED_EDGE ( 'NONE', *, *, #1712, .F. ) ;
#19541 = CARTESIAN_POINT ( 'NONE',  ( -6.350852961085760029, -1.281975124255709124E-13, -49.12500000000000711 ) ) ;
#19542 = CARTESIAN_POINT ( 'NONE',  ( 159.0000000000000284, -59.99999999999980105, 3.000000000000002665 ) ) ;
#19543 = CARTESIAN_POINT ( 'NONE',  ( 153.6488248654052029, -3.889087296526011706, -3.889087296526011706 ) ) ;
#19544 =( BOUNDED_CURVE ( )  B_SPLINE_CURVE ( 2, ( #13616, #2217, #22962, #6667, #11620, #6345, #18214, #13775, #27685 ),
 .UNSPECIFIED., .F., .T. ) 
 B_SPLINE_CURVE_WITH_KNOTS ( ( 3, 2, 2, 2, 3 ),
 ( 0.3593750000000000000, 0.3671875000000000000, 0.3750000000000000000, 0.3828125000000000000, 0.3906250000000000000 ),
 .UNSPECIFIED. ) 
 CURVE ( )  GEOMETRIC_REPRESENTATION_ITEM ( )  RATIONAL_B_SPLINE_CURVE ( ( 1.000000000000000000, 0.9238795325112867385, 1.000000000000000000, 0.9238795325112867385, 1.000000000000000000, 0.9238795325112867385, 1.000000000000000000, 0.9238795325112867385, 1.000000000000000000 ) ) 
 REPRESENTATION_ITEM ( '' )  );
#19545 = ORIENTED_EDGE ( 'NONE', *, *, #4663, .F. ) ;
#19546 = CARTESIAN_POINT ( 'NONE',  ( 118.4372167782374135, 0.7662911109079189043, -1.849990392679291551 ) ) ;
#19547 = MECHANICAL_DESIGN_GEOMETRIC_PRESENTATION_REPRESENTATION (  '', ( #11728 ), #12214 ) ;
#19548 = CARTESIAN_POINT ( 'NONE',  ( 118.7886751345946692, -1.999999999999918510, 2.220446049250313081E-13 ) ) ;
#19549 = CARTESIAN_POINT ( 'NONE',  ( -5.412658773652684552, -3.125000000000099920, -93.56698729810780435 ) ) ;
#19550 = CARTESIAN_POINT ( 'NONE',  ( 161.0000000000000284, 0.000000000000000000, 0.000000000000000000 ) ) ;
#19551 = CARTESIAN_POINT ( 'NONE',  ( 113.7499999999997584, 0.000000000000000000, -2.500000000000057732 ) ) ;
#19552 = CARTESIAN_POINT ( 'NONE',  ( 5.999999999999949374, 1.607695154586804565, -78.01933756729742697 ) ) ;
#19553 = EDGE_CURVE ( 'NONE', #9311, #6732, #29710, .T. ) ;
#19554 = CARTESIAN_POINT ( 'NONE',  ( 3.175426480543072749, 5.499999999999865885, -127.6249999999999858 ) ) ;
#19555 = ORIENTED_EDGE ( 'NONE', *, *, #1551, .T. ) ;
#19556 = CARTESIAN_POINT ( 'NONE',  ( 6.000000000000000888, 1.743066579297358182E-13, -82.58632486540520290 ) ) ;
#19557 = CARTESIAN_POINT ( 'NONE',  ( -6.350852961085760029, -1.281975124255709124E-13, -53.62500000000002842 ) ) ;
#19558 = CARTESIAN_POINT ( 'NONE',  ( 3.464101615137852974, 5.999999999999884537, -69.41367513459479710 ) ) ;
#19559 = CARTESIAN_POINT ( 'NONE',  ( -5.196152422706573404, -3.000000000000002665, -134.7886751345947971 ) ) ;
#19560 = CARTESIAN_POINT ( 'NONE',  ( 5.803206942314543149, 9.345129262100543954, -26.57517091834634826 ) ) ;
#19561 = CARTESIAN_POINT ( 'NONE',  ( 3.608439182435180470, -6.249999999999997335, -74.55801270189223828 ) ) ;
#19562 = ADVANCED_FACE ( 'NONE', ( #21658 ), #6194, .F. ) ;
#19563 = CARTESIAN_POINT ( 'NONE',  ( 24.84150635094622572, -1.291286745249641628E-13, -2.158493649053927044 ) ) ;
#19564 = CARTESIAN_POINT ( 'NONE',  ( 11.46132486540535389, 1.110223024625156540E-13, -2.500000000000002220 ) ) ;
#19565 = FILL_AREA_STYLE ('',( #2955 ) ) ;
#19566 = CARTESIAN_POINT ( 'NONE',  ( 0.000000000000000000, 5.999999999999977796, -61.21132486540520290 ) ) ;
#19567 = CARTESIAN_POINT ( 'NONE',  ( 4.763139720814407951, -2.749999999999988454, -140.0000000000000000 ) ) ;
#19568 = CARTESIAN_POINT ( 'NONE',  ( 10.16367513459492855, 1.767766952966431937, -1.767766952966431937 ) ) ;
#19569 = CARTESIAN_POINT ( 'NONE',  ( 3.608439182435180470, 6.249999999999982236, -153.5580127018922383 ) ) ;
#19570 = CARTESIAN_POINT ( 'NONE',  ( 0.000000000000000000, 5.999999999999977796, -101.7113248654052455 ) ) ;
#19571 = CARTESIAN_POINT ( 'NONE',  ( 5.999999999999949374, 1.607695154586804565, -51.59668783648704959 ) ) ;
#19572 = CARTESIAN_POINT ( 'NONE',  ( -6.350852961085760029, -1.281975124255709124E-13, -73.12500000000007105 ) ) ;
#19573 = CARTESIAN_POINT ( 'NONE',  ( -3.175426480542816510, 5.499999999999865885, -56.87500000000004974 ) ) ;
#19574 = ORIENTED_EDGE ( 'NONE', *, *, #3218, .T. ) ;
#19575 = CARTESIAN_POINT ( 'NONE',  ( 141.4836002691896510, 4.999999999999989342, -2.071067811865468400 ) ) ;
#19576 = CARTESIAN_POINT ( 'NONE',  ( 149.3437500000000284, -6.000000000000005329, -2.485281374238556218 ) ) ;
#19577 = CARTESIAN_POINT ( 'NONE',  ( -3.464101615137725076, 5.999999999999979572, -133.6636751345948539 ) ) ;
#19578 = CARTESIAN_POINT ( 'NONE',  ( 6.000000000000052403, -1.607695154586662678, -57.73066243270260145 ) ) ;
#19579 = CARTESIAN_POINT ( 'NONE',  ( 114.8122167782375698, 0.7662911109077388261, 1.849990392679591977 ) ) ;
#19580 = ORIENTED_EDGE ( 'NONE', *, *, #7275, .F. ) ;
#19581 = CARTESIAN_POINT ( 'NONE',  ( 146.4375000000000284, -4.242640687119298093, -4.242640687119298093 ) ) ;
#19582 = EDGE_CURVE ( 'NONE', #16955, #11567, #2569, .T. ) ;
#19583 =( BOUNDED_CURVE ( )  B_SPLINE_CURVE ( 2, ( #388, #28935, #7898, #5739, #9931, #12557, #19305, #697, #17313 ),
 .UNSPECIFIED., .F., .F. ) 
 B_SPLINE_CURVE_WITH_KNOTS ( ( 3, 2, 2, 2, 3 ),
 ( 0.09166666666666667407, 0.09259259259259255970, 0.09444444444444444198, 0.09629629629629632426, 0.09722222222222220989 ),
 .UNSPECIFIED. ) 
 CURVE ( )  GEOMETRIC_REPRESENTATION_ITEM ( )  RATIONAL_B_SPLINE_CURVE ( ( 0.9330127018922194093, 0.9330127018922194093, 1.000000000000000000, 0.8660254037844388186, 1.000000000000000000, 0.8660254037844388186, 1.000000000000000000, 0.9330127018922194093, 0.9330127018922194093 ) ) 
 REPRESENTATION_ITEM ( '' )  );
#19584 = LINE ( 'NONE', #17299, #1569 ) ;
#19585 = VECTOR ( 'NONE', #8727, 1000.000000000000000 ) ;
#19586 = CARTESIAN_POINT ( 'NONE',  ( -2.775557561562891351E-14, -5.500000000000115463, -176.2500000000000284 ) ) ;
#19587 = CARTESIAN_POINT ( 'NONE',  ( 15.87500000000008349, 1.414213562373201061, -1.414213562373090038 ) ) ;
#19588 = CARTESIAN_POINT ( 'NONE',  ( 2.775557561562891351E-14, 6.250000000000033751, -149.5669872981077901 ) ) ;
#19589 = FACE_OUTER_BOUND ( 'NONE', #18402, .T. ) ;
#19590 = CARTESIAN_POINT ( 'NONE',  ( 3.175426480543072749, 5.499999999999865885, -81.12500000000002842 ) ) ;
#19591 = EDGE_CURVE ( 'NONE', #13461, #23373, #24530, .T. ) ;
#19592 = CARTESIAN_POINT ( 'NONE',  ( 3.608439182435180470, 6.249999999999982236, -98.05801270189220986 ) ) ;
#19593 = CARTESIAN_POINT ( 'NONE',  ( -5.999999999999963585, -1.487416814333745711E-14, -106.4136751345948113 ) ) ;
#19594 = CARTESIAN_POINT ( 'NONE',  ( -5.999999999999956479, -1.607695154586745057, -96.76933756729742697 ) ) ;
#19595 = CYLINDRICAL_SURFACE ( 'NONE', #29784, 6.000000000000000888 ) ;
#19596 = FILL_AREA_STYLE_COLOUR ( '', #18170 ) ;
#19597 = CARTESIAN_POINT ( 'NONE',  ( 135.2945438920438903, -8.600858288651318517, 8.000000000000007105 ) ) ;
#19598 = CARTESIAN_POINT ( 'NONE',  ( -3.175426480542816066, 5.499999999999865885, -167.8750000000000568 ) ) ;
#19599 = DIRECTION ( 'NONE',  ( -1.000000000000000000, -1.067522139062651904E-16, -0.000000000000000000 ) ) ;
#19600 = CARTESIAN_POINT ( 'NONE',  ( 0.000000000000000000, 5.499999999999991118, -144.0000000000000284 ) ) ;
#19601 = CARTESIAN_POINT ( 'NONE',  ( 135.0000000000000284, -8.500000000000007105, -7.500000000000007105 ) ) ;
#19602 = CARTESIAN_POINT ( 'NONE',  ( -4.763139720814407951, -2.750000000000016431, -91.00000000000002842 ) ) ;
#19603 = CYLINDRICAL_SURFACE ( 'NONE', #15428, 2.499999999999999112 ) ;
#19604 = SURFACE_SIDE_STYLE ('',( #15479 ) ) ;
#19605 = CARTESIAN_POINT ( 'NONE',  ( 3.175426480543072749, 5.499999999999865885, -84.12499999999997158 ) ) ;
#19606 = AXIS2_PLACEMENT_3D ( 'NONE', #15677, #11205, #17970 ) ;
#19607 = CARTESIAN_POINT ( 'NONE',  ( 6.000000000000000888, 7.762456499804234384E-14, -144.0863248654052313 ) ) ;
#19608 = CARTESIAN_POINT ( 'NONE',  ( 10.71132486540515849, 2.500000000000168754, -5.551115123125782702E-14 ) ) ;
#19609 = CARTESIAN_POINT ( 'NONE',  ( 5.196152422706629359, -2.999999999999988898, -73.71132486540521711 ) ) ;
#19610 = VERTEX_POINT ( 'NONE', #28386 ) ;
#19611 = CARTESIAN_POINT ( 'NONE',  ( 160.2187500000000000, 2.485281374238555774, -6.000000000000005329 ) ) ;
#19612 = CYLINDRICAL_SURFACE ( 'NONE', #28817, 6.000000000000000888 ) ;
#19613 = CARTESIAN_POINT ( 'NONE',  ( 110.1636751345947260, 1.414213562373201061, -1.414213562372812483 ) ) ;
#19614 = CARTESIAN_POINT ( 'NONE',  ( 104.9372167782373566, -0.7662911109077388261, 1.849990392679772278 ) ) ;
#19615 = EDGE_CURVE ( 'NONE', #26795, #17525, #12825, .T. ) ;
#19616 = ORIENTED_EDGE ( 'NONE', *, *, #28247, .F. ) ;
#19617 =( BOUNDED_CURVE ( )  B_SPLINE_CURVE ( 2, ( #24197, #24806, #8370, #19744, #10393, #17166, #5595, #14998, #19899 ),
 .UNSPECIFIED., .F., .F. ) 
 B_SPLINE_CURVE_WITH_KNOTS ( ( 3, 2, 2, 2, 3 ),
 ( 0.6250000000000000000, 0.6259259259259259967, 0.6277777777777777679, 0.6296296296296296502, 0.6305555555555555358 ),
 .UNSPECIFIED. ) 
 CURVE ( )  GEOMETRIC_REPRESENTATION_ITEM ( )  RATIONAL_B_SPLINE_CURVE ( ( 0.9330127018922194093, 0.9330127018922194093, 1.000000000000000000, 0.8660254037844388186, 1.000000000000000000, 0.8660254037844388186, 1.000000000000000000, 0.9330127018922234061, 0.9330127018922194093 ) ) 
 REPRESENTATION_ITEM ( '' )  );
#19618 = VERTEX_POINT ( 'NONE', #7795 ) ;
#19619 = EDGE_LOOP ( 'NONE', ( #14338, #17364, #1198, #1591, #16072, #4787, #15217, #16928 ) ) ;
#19620 = CARTESIAN_POINT ( 'NONE',  ( 4.763139720814407951, 2.750000000000002665, -106.7500000000000142 ) ) ;
#19621 = CARTESIAN_POINT ( 'NONE',  ( 20.12500000000003197, 5.551115123125782702E-14, -2.649519052838444910 ) ) ;
#19622 = EDGE_CURVE ( 'NONE', #18908, #10100, #17362, .T. ) ;
#19623 = CARTESIAN_POINT ( 'NONE',  ( -7.216878364870328078, 0.000000000000000000, -121.5580127018922809 ) ) ;
#19624 =( BOUNDED_CURVE ( )  B_SPLINE_CURVE ( 2, ( #9250, #11747, #27964, #18348, #25521, #25361, #4630, #4331, #23252 ),
 .UNSPECIFIED., .F., .F. ) 
 B_SPLINE_CURVE_WITH_KNOTS ( ( 3, 2, 2, 2, 3 ),
 ( 0.3583333333333332815, 0.3592592592592592782, 0.3611111111111111605, 0.3629629629629629317, 0.3638888888888889284 ),
 .UNSPECIFIED. ) 
 CURVE ( )  GEOMETRIC_REPRESENTATION_ITEM ( )  RATIONAL_B_SPLINE_CURVE ( ( 0.9330127018922194093, 0.9330127018922154125, 1.000000000000000000, 0.8660254037844388186, 1.000000000000000000, 0.8660254037844388186, 1.000000000000000000, 0.9330127018922154125, 0.9330127018922194093 ) ) 
 REPRESENTATION_ITEM ( '' )  );
#19625 = EDGE_CURVE ( 'NONE', #22729, #15083, #15978, .T. ) ;
#19626 = ORIENTED_EDGE ( 'NONE', *, *, #29347, .T. ) ;
#19627 = AXIS2_PLACEMENT_3D ( 'NONE', #25311, #23899, #30090 ) ;
#19628 = CARTESIAN_POINT ( 'NONE',  ( 5.412658773652712085, -3.125000000000086153, -165.0669872981078186 ) ) ;
#19629 = CARTESIAN_POINT ( 'NONE',  ( 135.0000000000000568, -8.128079051996127902, 7.787350685426587482 ) ) ;
#19630 = CARTESIAN_POINT ( 'NONE',  ( 6.000000000000000888, -3.330669073875464691E-16, -7.560779664488942560E-35 ) ) ;
#19631 = VECTOR ( 'NONE', #15407, 1000.000000000000000 ) ;
#19632 = CARTESIAN_POINT ( 'NONE',  ( 7.216878364870455975, -6.409875621278545621E-14, -60.80801270189223118 ) ) ;
#19633 = ORIENTED_EDGE ( 'NONE', *, *, #11257, .T. ) ;
#19634 = CARTESIAN_POINT ( 'NONE',  ( 0.1148264294874666441, -15.24996949206075314, -8.589764806507680817 ) ) ;
#19635 = CARTESIAN_POINT ( 'NONE',  ( 116.1011751345945555, 0.8284271247463257382, -1.999999999999791278 ) ) ;
#19636 = CARTESIAN_POINT ( 'NONE',  ( 6.000000000000000888, 7.762456499804234384E-14, -132.0863248654052313 ) ) ;
#19637 =( LENGTH_UNIT ( ) NAMED_UNIT ( * ) SI_UNIT ( .MILLI., .METRE. ) );
#19638 = CARTESIAN_POINT ( 'NONE',  ( -3.175426480542816510, 5.499999999999865885, -169.3750000000000853 ) ) ;
#19639 = CARTESIAN_POINT ( 'NONE',  ( 120.4999999999998437, -2.499999999999891198, 3.330669073875469621E-13 ) ) ;
#19640 = CARTESIAN_POINT ( 'NONE',  ( 7.216878364870455975, -6.409875621278545621E-14, -165.8080127018922951 ) ) ;
#19641 = CARTESIAN_POINT ( 'NONE',  ( -6.110151747003138060E-09, -9.999999993889911565, 4.800749288174370299 ) ) ;
#19642 = CARTESIAN_POINT ( 'NONE',  ( 24.37500000000014566, -1.414213562373034527, 1.414213562373034527 ) ) ;
#19643 = CARTESIAN_POINT ( 'NONE',  ( -3.175426480542816066, 5.499999999999865885, -113.8749999999999858 ) ) ;
#19644 = CARTESIAN_POINT ( 'NONE',  ( 6.000000000000000888, 1.607695154586715303, -84.59668783648704959 ) ) ;
#19645 = CARTESIAN_POINT ( 'NONE',  ( -3.175426480542816510, -5.500000000000057732, -102.8750000000000142 ) ) ;
#19646 = CARTESIAN_POINT ( 'NONE',  ( -1.110223024625164676E-16, 2.000000000000012879, 2.021286199229734960E-15 ) ) ;
#19647 = EDGE_LOOP ( 'NONE', ( #29918, #9419, #3943, #8008 ) ) ;
#19648 = CARTESIAN_POINT ( 'NONE',  ( 19.00000000000012790, -1.873492889144845464, 1.873492889144845464 ) ) ;
#19649 = CARTESIAN_POINT ( 'NONE',  ( 0.8631338372297875372, -15.37878787878788067, -8.351220472436777342 ) ) ;
#19650 = CARTESIAN_POINT ( 'NONE',  ( 3.464101615137757051, -5.999999999999979572, -71.41367513459481131 ) ) ;
#19651 = ORIENTED_EDGE ( 'NONE', *, *, #26865, .T. ) ;
#19652 = CARTESIAN_POINT ( 'NONE',  ( 6.000000000000000888, -1.607695154586752384, -126.7306624327026157 ) ) ;
#19653 = CARTESIAN_POINT ( 'NONE',  ( 3.608439182435180470, 6.249999999999982236, -80.69198729810786119 ) ) ;
#19654 = EDGE_CURVE ( 'NONE', #2429, #28218, #13104, .T. ) ;
#19655 =( NAMED_UNIT ( * ) PLANE_ANGLE_UNIT ( ) SI_UNIT ( $, .RADIAN. ) );
#19656 = ORIENTED_EDGE ( 'NONE', *, *, #14744, .F. ) ;
#19657 = DIRECTION ( 'NONE',  ( 1.000000000000000000, 0.000000000000000000, 0.000000000000000000 ) ) ;
#19658 = ORIENTED_EDGE ( 'NONE', *, *, #25054, .T. ) ;
#19659 = EDGE_LOOP ( 'NONE', ( #1081, #12394, #14415, #25299 ) ) ;
#19660 = CARTESIAN_POINT ( 'NONE',  ( 161.2500000000000284, -6.000000000000005329, 0.000000000000000000 ) ) ;
#19661 = EDGE_CURVE ( 'NONE', #18063, #26173, #26675, .T. ) ;
#19662 = CARTESIAN_POINT ( 'NONE',  ( 2.775557561562891351E-14, 6.250000000000033751, -131.5669872981078470 ) ) ;
#19663 = CARTESIAN_POINT ( 'NONE',  ( 160.0000000000000284, 0.000000000000000000, 0.000000000000000000 ) ) ;
#19664 = CARTESIAN_POINT ( 'NONE',  ( 0.000000000000000000, 5.999999999999977796, -175.2113248654052597 ) ) ;
#19665 = CARTESIAN_POINT ( 'NONE',  ( 20.08632486540521001, -1.767766952966265404, 1.767766952966376426 ) ) ;
#19666 = COLOUR_RGB ( '', 0.40784314, 0.44705882, 0.49803922) ;
#19667 = ORIENTED_EDGE ( 'NONE', *, *, #27994, .T. ) ;
#19668 = CARTESIAN_POINT ( 'NONE',  ( 16.37500000000008527, -1.414213562373090038, 1.414213562373034527 ) ) ;
#19669 = CARTESIAN_POINT ( 'NONE',  ( 8.673617379884035472E-16, -15.50000000000001421, -5.656854249492387687 ) ) ;
#19670 = CARTESIAN_POINT ( 'NONE',  ( 6.000000000000000888, 7.762456499804235646E-14, -132.0863248654052313 ) ) ;
#19671 = CARTESIAN_POINT ( 'NONE',  ( 0.000000000000000000, 0.000000000000000000, 0.000000000000000000 ) ) ;
#19672 = CARTESIAN_POINT ( 'NONE',  ( 136.7663997308104058, -4.999999999999989342, -2.071067811865468400 ) ) ;
#19673 = CARTESIAN_POINT ( 'NONE',  ( 137.3363248654052029, 0.000000000000000000, -5.500000000000005329 ) ) ;
#19674 = CARTESIAN_POINT ( 'NONE',  ( -0.04562205425673532266, -14.50000000000001243, -8.291335958003946516 ) ) ;
#19675 = CARTESIAN_POINT ( 'NONE',  ( 5.412658773652739619, 3.124999999999988898, -70.31698729810781856 ) ) ;
#19676 = CARTESIAN_POINT ( 'NONE',  ( -5.412658773652684552, -3.125000000000099920, -53.06698729810782567 ) ) ;
#19677 = CARTESIAN_POINT ( 'NONE',  ( 135.0000000000000568, 2.227365967767792831, 5.061342792685060488 ) ) ;
#19678 = CARTESIAN_POINT ( 'NONE',  ( 105.6249999999999005, -1.767766952966376426, -1.767766952966320915 ) ) ;
#19679 = PLANE ( 'NONE',  #11331 ) ;
#19680 = CARTESIAN_POINT ( 'NONE',  ( -6.350852961085760029, -1.281975124255709124E-13, -127.1249999999999858 ) ) ;
#19681 = AXIS2_PLACEMENT_3D ( 'NONE', #6351, #24480, #3428 ) ;
#19682 = DIRECTION ( 'NONE',  ( -1.000000000000000000, -0.000000000000000000, 0.000000000000000000 ) ) ;
#19683 = CARTESIAN_POINT ( 'NONE',  ( 154.1324251345948539, -5.500000000000012434, -2.278174593052012309 ) ) ;
#19684 = VERTEX_POINT ( 'NONE', #15522 ) ;
#19685 = CARTESIAN_POINT ( 'NONE',  ( 5.196152422706629359, 3.000000000000002665, -173.9613248654052313 ) ) ;
#19686 = LINE ( 'NONE', #29175, #17545 ) ;
#19687 = CARTESIAN_POINT ( 'NONE',  ( -5.999999999999968026, -1.607695154586722186, -160.3466878364870638 ) ) ;
#19688 = CARTESIAN_POINT ( 'NONE',  ( -10.00000000000000178, -19.99999999999998934, 4.000000000000003553 ) ) ;
#19689 = CARTESIAN_POINT ( 'NONE',  ( 108.7261751345945555, -1.999999999999941602, 0.8284271247463557142 ) ) ;
#19690 = ORIENTED_EDGE ( 'NONE', *, *, #8732, .T. ) ;
#19691 = CARTESIAN_POINT ( 'NONE',  ( 114.8122167782375698, 0.7662911109077388261, 1.849990392679591977 ) ) ;
#19692 = CARTESIAN_POINT ( 'NONE',  ( 10.68750000000004263, -0.8284271247460552878, -1.999999999999971800 ) ) ;
#19693 = EDGE_CURVE ( 'NONE', #9277, #28549, #4348, .T. ) ;
#19694 = CARTESIAN_POINT ( 'NONE',  ( -5.196152422706573404, -3.000000000000002665, -50.78867513459483973 ) ) ;
#19695 = EDGE_CURVE ( 'NONE', #9511, #26400, #406, .T. ) ;
#19696 = CARTESIAN_POINT ( 'NONE',  ( 114.1250000000000142, 1.767766952966293159, 1.767766952966320915 ) ) ;
#19697 = CARTESIAN_POINT ( 'NONE',  ( 116.0000000000000142, 0.000000000000000000, 0.000000000000000000 ) ) ;
#19698 = DIRECTION ( 'NONE',  ( -1.000000000000000000, -1.665334536937736783E-16, -2.220446049250315546E-16 ) ) ;
#19699 = EDGE_LOOP ( 'NONE', ( #11067, #2052, #4606, #19111 ) ) ;
#19700 = CARTESIAN_POINT ( 'NONE',  ( 6.000000000000052403, -1.607695154586662678, -82.65331216351297883 ) ) ;
#19701 = CARTESIAN_POINT ( 'NONE',  ( 4.763139720814407951, 2.750000000000002665, -55.75000000000002132 ) ) ;
#19702 = CARTESIAN_POINT ( 'NONE',  ( -5.999999999999963585, 1.780251999655701777E-13, -86.91367513459485394 ) ) ;
#19703 = CARTESIAN_POINT ( 'NONE',  ( -5.999999999999956479, -1.607695154586745057, -134.8466878364870354 ) ) ;
#19704 = CARTESIAN_POINT ( 'NONE',  ( 5.412658773652712085, -3.125000000000086153, -74.43301270189223828 ) ) ;
#19705 = CARTESIAN_POINT ( 'NONE',  ( 156.6413997308104342, 2.071067811865468400, -4.999999999999989342 ) ) ;
#19706 = CARTESIAN_POINT ( 'NONE',  ( -5.196152422706601826, 2.999999999999975131, -168.9613248654052029 ) ) ;
#19707 = CARTESIAN_POINT ( 'NONE',  ( 6.000000000000000888, 1.607695154586715303, -80.09668783648703538 ) ) ;
#19708 = VECTOR ( 'NONE', #20785, 1000.000000000000000 ) ;
#19709 =( BOUNDED_CURVE ( )  B_SPLINE_CURVE ( 2, ( #12071, #11928, #15963, #2797, #25261, #4946, #28587, #2368, #5248 ),
 .UNSPECIFIED., .F., .T. ) 
 B_SPLINE_CURVE_WITH_KNOTS ( ( 3, 2, 2, 2, 3 ),
 ( 0.2941176470588235392, 0.3014705882352941013, 0.3088235294117647189, 0.3161764705882352811, 0.3235294117647058987 ),
 .UNSPECIFIED. ) 
 CURVE ( )  GEOMETRIC_REPRESENTATION_ITEM ( )  RATIONAL_B_SPLINE_CURVE ( ( 1.000000000000000000, 0.9238795325112867385, 1.000000000000000000, 0.9238795325112867385, 1.000000000000000000, 0.9238795325112867385, 1.000000000000000000, 0.9238795325112867385, 1.000000000000000000 ) ) 
 REPRESENTATION_ITEM ( '' )  );
#19710 = CARTESIAN_POINT ( 'NONE',  ( 0.000000000000000000, 5.499999999999991118, -135.0000000000000000 ) ) ;
#19711 = CARTESIAN_POINT ( 'NONE',  ( 159.0000000000000284, -11.07692307692306777, -4.615384615384604317 ) ) ;
#19712 = CARTESIAN_POINT ( 'NONE',  ( -3.608439182435115633, 6.249999999999965361, -147.3080127018922667 ) ) ;
#19713 = CARTESIAN_POINT ( 'NONE',  ( 140.0000000000000284, -54.99999999999990763, 8.000000000000007105 ) ) ;
#19714 = CARTESIAN_POINT ( 'NONE',  ( -5.999999999999963585, 1.780251999655701777E-13, -81.83632486540521711 ) ) ;
#19715 = CARTESIAN_POINT ( 'NONE',  ( 3.175426480543072749, -5.500000000000105693, -74.12500000000007105 ) ) ;
#19716 = CARTESIAN_POINT ( 'NONE',  ( -3.175426480542816510, -5.500000000000057732, -57.87500000000004974 ) ) ;
#19717 = EDGE_LOOP ( 'NONE', ( #15863, #23499, #13613, #5460 ) ) ;
#19718 = CARTESIAN_POINT ( 'NONE',  ( 153.6562500000000568, -6.000000000000005329, 2.485281374238556218 ) ) ;
#19719 = CARTESIAN_POINT ( 'NONE',  ( 3.464101615137852974, 5.999999999999884537, -127.3363248654051887 ) ) ;
#19720 = CIRCLE ( 'NONE', #23664, 9.999999999999996447 ) ;
#19721 = CARTESIAN_POINT ( 'NONE',  ( -3.464101615137757051, -5.999999999999979572, -58.16367513459481131 ) ) ;
#19722 = ADVANCED_FACE ( 'NONE', ( #12761 ), #1652, .T. ) ;
#19723 = ORIENTED_EDGE ( 'NONE', *, *, #1151, .T. ) ;
#19724 = CARTESIAN_POINT ( 'NONE',  ( 144.0000000000000284, 6.000000000000005329, 0.000000000000000000 ) ) ;
#19725 = CARTESIAN_POINT ( 'NONE',  ( 119.9999999999997868, 1.387778780781445676E-13, 1.110223024625156540E-13 ) ) ;
#19726 = CARTESIAN_POINT ( 'NONE',  ( -3.464101615137725076, 5.999999999999979572, -64.08632486540521711 ) ) ;
#19727 = CARTESIAN_POINT ( 'NONE',  ( 17.56250000000009592, -1.999999999999851674, -0.8284271247461753029 ) ) ;
#19728 = ORIENTED_EDGE ( 'NONE', *, *, #6618, .F. ) ;
#19729 = CARTESIAN_POINT ( 'NONE',  ( -3.608439182435115633, 6.249999999999965361, -146.4419872981078470 ) ) ;
#19730 = CARTESIAN_POINT ( 'NONE',  ( 0.000000000000000000, 5.499999999999991118, -82.50000000000001421 ) ) ;
#19731 = CARTESIAN_POINT ( 'NONE',  ( -7.216878364870328078, 0.000000000000000000, -96.05801270189226670 ) ) ;
#19732 = CARTESIAN_POINT ( 'NONE',  ( 116.0000000000000142, 0.000000000000000000, -5.500000000000000000 ) ) ;
#19733 = PRESENTATION_STYLE_ASSIGNMENT (( #10380 ) ) ;
#19734 = CARTESIAN_POINT ( 'NONE',  ( 106.6488248654051318, 2.000000000000122125, -0.8284271247459350507 ) ) ;
#19735 = CARTESIAN_POINT ( 'NONE',  ( 140.0000000000000284, -11.45643923738959202, -5.000000000000004441 ) ) ;
#19736 = CARTESIAN_POINT ( 'NONE',  ( 6.000000000000000888, 1.743066579297358182E-13, -78.08632486540520290 ) ) ;
#19737 = FILL_AREA_STYLE ('',( #10535 ) ) ;
#19738 = CARTESIAN_POINT ( 'NONE',  ( -4.763139720814407951, -2.750000000000016431, -164.5000000000000284 ) ) ;
#19739 = CARTESIAN_POINT ( 'NONE',  ( 6.000000000000000888, -3.330669073875464691E-16, -7.560779664488942560E-35 ) ) ;
#19740 = CARTESIAN_POINT ( 'NONE',  ( -3.175426480542816510, 5.499999999999865885, -149.8750000000000568 ) ) ;
#19741 = CARTESIAN_POINT ( 'NONE',  ( 135.0000000000000000, 5.116053516637836474, 2.738964164488275621 ) ) ;
#19742 = EDGE_CURVE ( 'NONE', #24590, #750, #2396, .T. ) ;
#19743 = CARTESIAN_POINT ( 'NONE',  ( 4.763139720814407951, 2.750000000000002665, -93.25000000000000000 ) ) ;
#19744 = CARTESIAN_POINT ( 'NONE',  ( 3.464101615137757051, -5.999999999999979572, -130.8363248654052029 ) ) ;
#19745 = CARTESIAN_POINT ( 'NONE',  ( -4.763139720814407951, 2.749999999999946709, -82.25000000000004263 ) ) ;
#19746 = DIRECTION ( 'NONE',  ( 0.000000000000000000, 0.000000000000000000, 1.000000000000000000 ) ) ;
#19747 = CARTESIAN_POINT ( 'NONE',  ( 151.2336002691896510, -4.999999999999989342, 2.071067811865468400 ) ) ;
#19748 = CARTESIAN_POINT ( 'NONE',  ( 3.464101615137757051, -5.999999999999979572, -72.33632486540520290 ) ) ;
#19749 = CARTESIAN_POINT ( 'NONE',  ( 161.4187058191337769, -3.655040188723187367, -4.674867660659138835 ) ) ;
#19750 = CARTESIAN_POINT ( 'NONE',  ( 5.999999999999999112, 2.951592740943527306E-14, -156.0863248654052597 ) ) ;
#19751 = CARTESIAN_POINT ( 'NONE',  ( 21.75000000000007461, 2.220446049250313081E-13, -2.000000000000001776 ) ) ;
#19752 = CARTESIAN_POINT ( 'NONE',  ( 6.000000000000052403, 1.607695154586625819, -129.0193375672974128 ) ) ;
#19753 = CARTESIAN_POINT ( 'NONE',  ( 6.000000000000000888, -1.859271017917181981E-14, -72.66367513459483973 ) ) ;
#19754 = CARTESIAN_POINT ( 'NONE',  ( 3.464101615137852974, 5.999999999999884537, -75.41367513459483973 ) ) ;
#19755 =( GEOMETRIC_REPRESENTATION_CONTEXT ( 3 ) GLOBAL_UNCERTAINTY_ASSIGNED_CONTEXT ( ( #2596 ) ) GLOBAL_UNIT_ASSIGNED_CONTEXT ( ( #27730, #10893, #23006 ) ) REPRESENTATION_CONTEXT ( 'NONE', 'WORKASPACE' ) );
#19756 = ORIENTED_EDGE ( 'NONE', *, *, #4146, .T. ) ;
#19757 = CARTESIAN_POINT ( 'NONE',  ( 159.1875000000000284, 4.242640687119269671, 4.242640687119298093 ) ) ;
#19758 = CARTESIAN_POINT ( 'NONE',  ( 0.000000000000000000, 0.000000000000000000, 0.000000000000000000 ) ) ;
#19759 = CARTESIAN_POINT ( 'NONE',  ( -4.999999999999886313, -69.50000000000001421, 8.000000000000007105 ) ) ;
#19760 = CARTESIAN_POINT ( 'NONE',  ( 120.8127832217621318, -1.849990392679411677, 0.7662911109079489913 ) ) ;
#19761 = ORIENTED_EDGE ( 'NONE', *, *, #25969, .T. ) ;
#19762 = CARTESIAN_POINT ( 'NONE',  ( -4.763139720814407951, -2.750000000000016431, -107.5000000000000426 ) ) ;
#19763 = CARTESIAN_POINT ( 'NONE',  ( 4.763139720814407951, 2.750000000000002665, -150.2500000000000000 ) ) ;
#19764 = CARTESIAN_POINT ( 'NONE',  ( 2.775557561562891351E-14, -6.250000000000061284, -116.6830127018922383 ) ) ;
#19765 =( GEOMETRIC_REPRESENTATION_CONTEXT ( 3 ) GLOBAL_UNCERTAINTY_ASSIGNED_CONTEXT ( ( #18880 ) ) GLOBAL_UNIT_ASSIGNED_CONTEXT ( ( #2670, #16701, #25875 ) ) REPRESENTATION_CONTEXT ( 'NONE', 'WORKASPACE' ) );
#19766 = ORIENTED_EDGE ( 'NONE', *, *, #26197, .T. ) ;
#19767 = CARTESIAN_POINT ( 'NONE',  ( -3.464101615137757051, -5.999999999999979572, -110.6636751345948113 ) ) ;
#19768 = CARTESIAN_POINT ( 'NONE',  ( 2.775557561562891351E-14, 6.250000000000033751, -160.0669872981078754 ) ) ;
#19769 = CARTESIAN_POINT ( 'NONE',  ( 106.1249999999999858, 1.767766952966320915, 1.767766952966431937 ) ) ;
#19770 = CARTESIAN_POINT ( 'NONE',  ( 5.412658773652739619, 3.124999999999988898, -53.18301270189223828 ) ) ;
#19771 = ORIENTED_EDGE ( 'NONE', *, *, #20815, .T. ) ;
#19772 = CARTESIAN_POINT ( 'NONE',  ( 19.99999999999998934, 0.000000000000000000, 0.000000000000000000 ) ) ;
#19773 = CARTESIAN_POINT ( 'NONE',  ( 6.000000000000000888, 1.743066579297358182E-13, -94.58632486540521711 ) ) ;
#19774 = FACE_OUTER_BOUND ( 'NONE', #30001, .T. ) ;
#19775 = CARTESIAN_POINT ( 'NONE',  ( 155.6175748654052313, 5.500000000000012434, -2.278174593052012309 ) ) ;
#19776 = CARTESIAN_POINT ( 'NONE',  ( 3.175426480543072749, 5.499999999999865885, -174.1250000000000284 ) ) ;
#19777 = CARTESIAN_POINT ( 'NONE',  ( 105.5627832217622597, 0.7662911109077686911, 1.849990392679772278 ) ) ;
#19778 = CARTESIAN_POINT ( 'NONE',  ( 152.8050748654052029, 5.500000000000012434, 2.278174593052012309 ) ) ;
#19779 = CARTESIAN_POINT ( 'NONE',  ( 2.775557561562891351E-14, -6.250000000000061284, -166.1830127018922383 ) ) ;
#19780 = CARTESIAN_POINT ( 'NONE',  ( 155.3363248654052313, 0.000000000000000000, -5.500000000000005329 ) ) ;
#19781 = ADVANCED_FACE ( 'NONE', ( #1180 ), #13009, .T. ) ;
#19782 = CARTESIAN_POINT ( 'NONE',  ( -4.763139720814407951, -2.750000000000016431, -119.5000000000000568 ) ) ;
#19783 = PRESENTATION_STYLE_ASSIGNMENT (( #3331 ) ) ;
#19784 = CARTESIAN_POINT ( 'NONE',  ( -4.763139720814407951, 2.749999999999946709, -103.2500000000000142 ) ) ;
#19785 = SURFACE_STYLE_USAGE ( .BOTH. , #12912 ) ;
#19786 = CARTESIAN_POINT ( 'NONE',  ( -5.999999999999963585, 1.780251999655701777E-13, -77.91367513459482552 ) ) ;
#19787 = CARTESIAN_POINT ( 'NONE',  ( 11.22617513459480598, 2.500000000000024425, -1.035533905932869425 ) ) ;
#19788 = VERTEX_POINT ( 'NONE', #30060 ) ;
#19789 = CARTESIAN_POINT ( 'NONE',  ( 15.87500000000000000, 1.665334536937734811E-13, 2.649519052838278377 ) ) ;
#19790 = CARTESIAN_POINT ( 'NONE',  ( 119.3749999999998863, -1.767766952966209892, 1.767766952966542959 ) ) ;
#19791 = CARTESIAN_POINT ( 'NONE',  ( 19.99999999999998934, 0.000000000000000000, 0.000000000000000000 ) ) ;
#19792 = EDGE_CURVE ( 'NONE', #30239, #407, #11523, .T. ) ;
#19793 =( BOUNDED_CURVE ( )  B_SPLINE_CURVE ( 2, ( #1304, #22527, #24654, #29248, #1616, #29868, #3600, #8849, #24952 ),
 .UNSPECIFIED., .F., .F. ) 
 B_SPLINE_CURVE_WITH_KNOTS ( ( 3, 2, 2, 2, 3 ),
 ( 0.2361111111111111049, 0.2370370370370370461, 0.2388888888888889006, 0.2407407407407407274, 0.2416666666666666685 ),
 .UNSPECIFIED. ) 
 CURVE ( )  GEOMETRIC_REPRESENTATION_ITEM ( )  RATIONAL_B_SPLINE_CURVE ( ( 0.9330127018922196314, 0.9330127018922185211, 1.000000000000000000, 0.8660254037844388186, 1.000000000000000000, 0.8660254037844388186, 1.000000000000000000, 0.9330127018922184101, 0.9330127018922194093 ) ) 
 REPRESENTATION_ITEM ( '' )  );
#19794 = ORIENTED_EDGE ( 'NONE', *, *, #9223, .T. ) ;
#19795 = CARTESIAN_POINT ( 'NONE',  ( -6.350852961085760029, -1.281975124255709124E-13, -160.1250000000000284 ) ) ;
#19796 = AXIS2_PLACEMENT_3D ( 'NONE', #21054, #30401, #28083 ) ;
#19797 = CARTESIAN_POINT ( 'NONE',  ( 3.608439182435180470, -6.249999999999997335, -79.69198729810786119 ) ) ;
#19798 = CARTESIAN_POINT ( 'NONE',  ( 0.000000000000000000, 0.000000000000000000, 0.000000000000000000 ) ) ;
#19799 = ORIENTED_EDGE ( 'NONE', *, *, #14818, .F. ) ;
#19800 = DIRECTION ( 'NONE',  ( -7.147005652999508048E-36, 5.642372883946980038E-36, 1.000000000000000000 ) ) ;
#19801 = ORIENTED_EDGE ( 'NONE', *, *, #23425, .T. ) ;
#19802 = VERTEX_POINT ( 'NONE', #9494 ) ;
#19803 = CARTESIAN_POINT ( 'NONE',  ( 161.6250000000000568, 0.000000000000000000, -6.000000000000005329 ) ) ;
#19804 = CARTESIAN_POINT ( 'NONE',  ( 3.608439182435180470, 6.249999999999982236, -138.5580127018922099 ) ) ;
#19805 = EDGE_LOOP ( 'NONE', ( #5215, #7418, #29875, #22265 ) ) ;
#19806 = CARTESIAN_POINT ( 'NONE',  ( 3.608439182435180470, 6.249999999999982236, -130.1919872981078470 ) ) ;
#19807 = CARTESIAN_POINT ( 'NONE',  ( -3.175426480542816510, 5.499999999999865885, -170.8750000000000853 ) ) ;
#19808 = CARTESIAN_POINT ( 'NONE',  ( 135.6566535407617948, -9.123793365789314436, -8.000000000000007105 ) ) ;
#19809 = CARTESIAN_POINT ( 'NONE',  ( 5.999999999999949374, 1.607695154586804565, -48.01933756729744118 ) ) ;
#19810 = VERTEX_POINT ( 'NONE', #2273 ) ;
#19811 = CARTESIAN_POINT ( 'NONE',  ( 16.06250000000006040, 2.000000000000151879, 0.8284271247461152399 ) ) ;
#19812 = DIRECTION ( 'NONE',  ( -7.147005652999508048E-36, 5.642372883946980038E-36, 1.000000000000000000 ) ) ;
#19813 = FILL_AREA_STYLE ('',( #21976 ) ) ;
#19814 = CARTESIAN_POINT ( 'NONE',  ( 6.000000000000000888, -1.859271017917181981E-14, -171.6636751345948539 ) ) ;
#19815 = CARTESIAN_POINT ( 'NONE',  ( 13.53867513459486283, 1.110223024625156540E-13, 2.499999999999946709 ) ) ;
#19816 = CARTESIAN_POINT ( 'NONE',  ( 3.608439182435180470, -6.249999999999997335, -70.69198729810781856 ) ) ;
#19817 = CARTESIAN_POINT ( 'NONE',  ( 5.412658773652712085, -3.125000000000086153, -51.06698729810782567 ) ) ;
#19818 = CARTESIAN_POINT ( 'NONE',  ( 5.999999999999999112, 2.951592740943527306E-14, -162.0863248654052029 ) ) ;
#19819 = CARTESIAN_POINT ( 'NONE',  ( 0.000000000000000000, 0.000000000000000000, 0.000000000000000000 ) ) ;
#19820 = CARTESIAN_POINT ( 'NONE',  ( -3.464101615137725076, 5.999999999999979572, -103.0863248654052171 ) ) ;
#19821 = ADVANCED_FACE ( 'NONE', ( #25612 ), #26498, .T. ) ;
#19822 = CARTESIAN_POINT ( 'NONE',  ( 5.196152422706629359, 3.000000000000002665, -128.0386751345948824 ) ) ;
#19823 = CARTESIAN_POINT ( 'NONE',  ( 4.763139720814407951, -2.749999999999988454, -132.5000000000000000 ) ) ;
#19824 = FILL_AREA_STYLE ('',( #24423 ) ) ;
#19825 = ORIENTED_EDGE ( 'NONE', *, *, #6081, .T. ) ;
#19826 = DIRECTION ( 'NONE',  ( 1.000000000000000000, 1.067522139062651904E-16, -0.000000000000000000 ) ) ;
#19827 = CARTESIAN_POINT ( 'NONE',  ( 6.000000000000000888, -3.330669073875464691E-16, -7.560779664488942560E-35 ) ) ;
#19828 = DIRECTION ( 'NONE',  ( -7.147005652999508048E-36, 5.642372883946980038E-36, 1.000000000000000000 ) ) ;
#19829 = EDGE_CURVE ( 'NONE', #688, #15144, #15142, .T. ) ;
#19830 = CARTESIAN_POINT ( 'NONE',  ( 153.2738248654052313, -3.889087296526011706, 3.889087296526011706 ) ) ;
#19831 = DIRECTION ( 'NONE',  ( 1.000000000000000000, -5.551115123125773458E-17, -1.260129944081490338E-35 ) ) ;
#19832 = EDGE_LOOP ( 'NONE', ( #2614, #9800, #9010, #19925 ) ) ;
#19833 = CARTESIAN_POINT ( 'NONE',  ( 112.1872167782374135, -1.849990392679411677, -0.7662911109075883909 ) ) ;
#19834 = CARTESIAN_POINT ( 'NONE',  ( -3.464101615137725076, 5.999999999999979572, -71.58632486540520290 ) ) ;
#19835 = CARTESIAN_POINT ( 'NONE',  ( -7.216878364870328078, 0.000000000000000000, -96.69198729810780435 ) ) ;
#19836 = CARTESIAN_POINT ( 'NONE',  ( 0.000000000000000000, 5.999999999999977796, -172.7886751345948255 ) ) ;
#19837 = LINE ( 'NONE', #14942, #19024 ) ;
#19838 = CARTESIAN_POINT ( 'NONE',  ( 115.4999999999998153, -2.499999999999891198, 0.000000000000000000 ) ) ;
#19839 = CARTESIAN_POINT ( 'NONE',  ( 161.0000000000000284, 0.000000000000000000, 0.000000000000000000 ) ) ;
#19840 = CARTESIAN_POINT ( 'NONE',  ( -5.196152422706601826, 2.999999999999975131, -77.46132486540524553 ) ) ;
#19841 = ORIENTED_EDGE ( 'NONE', *, *, #6887, .T. ) ;
#19842 = CARTESIAN_POINT ( 'NONE',  ( 6.000000000000000888, 7.762456499804234384E-14, -138.0863248654051745 ) ) ;
#19843 = CARTESIAN_POINT ( 'NONE',  ( -3.175426480542816510, 5.499999999999865885, -47.87500000000000000 ) ) ;
#19844 = CARTESIAN_POINT ( 'NONE',  ( 25.00000000000013500, 2.000000000000279332, -5.551115123125782702E-14 ) ) ;
#19845 = DIRECTION ( 'NONE',  ( -7.147005652999508048E-36, 5.642372883946980038E-36, 1.000000000000000000 ) ) ;
#19846 = CARTESIAN_POINT ( 'NONE',  ( -3.608439182435115633, 6.249999999999965361, -76.80801270189225249 ) ) ;
#19847 = CARTESIAN_POINT ( 'NONE',  ( 6.000000000000000888, 7.762456499804235646E-14, -129.0863248654052029 ) ) ;
#19848 = CARTESIAN_POINT ( 'NONE',  ( 149.9851497308104342, -3.535533905932725318, 3.535533905932725318 ) ) ;
#19849 = CARTESIAN_POINT ( 'NONE',  ( -3.464101615137725076, 5.999999999999979572, -177.1636751345947971 ) ) ;
#19850 = DIRECTION ( 'NONE',  ( 1.000000000000000000, -5.551115123125773458E-17, -1.260129944081490338E-35 ) ) ;
#19851 = DIRECTION ( 'NONE',  ( 5.551115123125783935E-17, -1.000000000000000000, -8.881784197001254296E-16 ) ) ;
#19852 = SURFACE_STYLE_USAGE ( .BOTH. , #26598 ) ;
#19853 = ADVANCED_FACE ( 'NONE', ( #14286 ), #26201, .T. ) ;
#19854 = CARTESIAN_POINT ( 'NONE',  ( 135.0781295278050322, -7.870998221347940138, 8.267028835410057397 ) ) ;
#19855 = EDGE_CURVE ( 'NONE', #28218, #22758, #10096, .T. ) ;
#19856 = CARTESIAN_POINT ( 'NONE',  ( -3.175426480542816066, 5.499999999999865885, -133.3750000000000284 ) ) ;
#19857 = CARTESIAN_POINT ( 'NONE',  ( 10.53867513459491612, 5.551115123125782702E-14, 2.499999999999724665 ) ) ;
#19858 = CARTESIAN_POINT ( 'NONE',  ( -7.216878364870328078, 0.000000000000000000, -147.0580127018922667 ) ) ;
#19859 = CARTESIAN_POINT ( 'NONE',  ( -5.999999999999919176, 1.607695154586804565, -158.4033121635129930 ) ) ;
#19860 = CARTESIAN_POINT ( 'NONE',  ( -3.175426480542816066, 5.499999999999865885, -59.87500000000005684 ) ) ;
#19861 = CARTESIAN_POINT ( 'NONE',  ( 0.000000000000000000, 0.000000000000000000, 0.000000000000000000 ) ) ;
#19862 = CARTESIAN_POINT ( 'NONE',  ( -4.763139720814407951, -2.750000000000016431, -53.49999999999999289 ) ) ;
#19863 = FACE_OUTER_BOUND ( 'NONE', #10636, .T. ) ;
#19864 = ORIENTED_EDGE ( 'NONE', *, *, #20313, .F. ) ;
#19865 = CARTESIAN_POINT ( 'NONE',  ( 153.0937500000000284, 6.000000000000005329, 2.485281374238585972 ) ) ;
#19866 = FACE_OUTER_BOUND ( 'NONE', #2172, .T. ) ;
#19867 = CARTESIAN_POINT ( 'NONE',  ( 15.56250000000003375, -1.999999999999851674, -0.8284271247462354770 ) ) ;
#19868 = CARTESIAN_POINT ( 'NONE',  ( 6.000000000000000888, -1.859271017917181981E-14, -88.58632486540523132 ) ) ;
#19869 = CARTESIAN_POINT ( 'NONE',  ( 111.1247167782376124, -1.849990392679579099, 1.110223024625156540E-13 ) ) ;
#19870 = ORIENTED_EDGE ( 'NONE', *, *, #1117, .F. ) ;
#19871 = CARTESIAN_POINT ( 'NONE',  ( 145.4062500000000284, 6.000000000000005329, -2.485281374238555774 ) ) ;
#19872 = CARTESIAN_POINT ( 'NONE',  ( 161.1460176603489458, -1.573196579648956872, 5.431622084658472183 ) ) ;
#19873 = ORIENTED_EDGE ( 'NONE', *, *, #23661, .F. ) ;
#19874 = AXIS2_PLACEMENT_3D ( 'NONE', #9456, #10323, #21582 ) ;
#19875 = CARTESIAN_POINT ( 'NONE',  ( -4.763139720814407951, 2.749999999999946709, -145.2500000000000000 ) ) ;
#19876 = CARTESIAN_POINT ( 'NONE',  ( 5.412658773652739619, 3.124999999999988898, -49.31698729810784698 ) ) ;
#19877 = CARTESIAN_POINT ( 'NONE',  ( 15.18750000000007105, 0.8284271247462955401, 1.999999999999851674 ) ) ;
#19878 = ORIENTED_EDGE ( 'NONE', *, *, #13203, .T. ) ;
#19879 = CARTESIAN_POINT ( 'NONE',  ( 2.775557561562891351E-14, -6.250000000000061284, -144.3169872981078186 ) ) ;
#19880 = CARTESIAN_POINT ( 'NONE',  ( -3.175426480542816510, -5.500000000000057732, -69.87500000000005684 ) ) ;
#19881 = CARTESIAN_POINT ( 'NONE',  ( 13.93750000000005684, -2.649519052838238409, -1.097466725451559322 ) ) ;
#19882 = CARTESIAN_POINT ( 'NONE',  ( -5.412658773652739619, 3.124999999999975131, -91.68301270189228092 ) ) ;
#19883 =( BOUNDED_CURVE ( )  B_SPLINE_CURVE ( 2, ( #21933, #867, #7933, #17344, #26659, #8075, #17493, #26805, #5771 ),
 .UNSPECIFIED., .F., .T. ) 
 B_SPLINE_CURVE_WITH_KNOTS ( ( 3, 2, 2, 2, 3 ),
 ( 0.4875000000000000444, 0.4937499999999998002, 0.4999999999999995559, 0.5062499999999993117, 0.5124999999999990674 ),
 .UNSPECIFIED. ) 
 CURVE ( )  GEOMETRIC_REPRESENTATION_ITEM ( )  RATIONAL_B_SPLINE_CURVE ( ( 1.000000000000000000, 0.9238795325112867385, 1.000000000000000000, 0.9238795325112867385, 1.000000000000000000, 0.9238795325112867385, 1.000000000000000000, 0.9238795325112975076, 0.9999999999999892308 ) ) 
 REPRESENTATION_ITEM ( '' )  );
#19884 = CARTESIAN_POINT ( 'NONE',  ( -5.196152422706601826, 2.999999999999975131, -175.5386751345948824 ) ) ;
#19885 = CYLINDRICAL_SURFACE ( 'NONE', #13306, 5.500000000000000000 ) ;
#19886 = CARTESIAN_POINT ( 'NONE',  ( 106.5238248654050039, 0.8284271247463855792, -1.999999999999791278 ) ) ;
#19887 = CARTESIAN_POINT ( 'NONE',  ( -14.99999999999999289, -54.99999999999990763, 8.000000000000007105 ) ) ;
#19888 = DIRECTION ( 'NONE',  ( -7.147005652999508048E-36, 5.642372883946980038E-36, 1.000000000000000000 ) ) ;
#19889 = EDGE_CURVE ( 'NONE', #956, #16271, #14014, .T. ) ;
#19890 = CARTESIAN_POINT ( 'NONE',  ( -3.175426480542816066, 5.499999999999865885, -157.3750000000000000 ) ) ;
#19891 = FACE_OUTER_BOUND ( 'NONE', #24575, .T. ) ;
#19892 = CARTESIAN_POINT ( 'NONE',  ( -2.775557561562891351E-14, -5.500000000000115463, -143.2500000000000000 ) ) ;
#19893 = CARTESIAN_POINT ( 'NONE',  ( 6.000000000000000888, 1.743066579297358182E-13, -77.16367513459482552 ) ) ;
#19894 = CARTESIAN_POINT ( 'NONE',  ( 137.4449251345948255, -5.500000000000012434, 2.278174593052012309 ) ) ;
#19895 = MECHANICAL_DESIGN_GEOMETRIC_PRESENTATION_REPRESENTATION (  '', ( #274 ), #16399 ) ;
#19896 = UNCERTAINTY_MEASURE_WITH_UNIT (LENGTH_MEASURE( 1.000000000000000082E-05 ), #13024, 'distance_accuracy_value', 'NONE');
#19897 = CARTESIAN_POINT ( 'NONE',  ( 4.763139720814407951, 2.750000000000002665, -88.75000000000000000 ) ) ;
#19898 = DIRECTION ( 'NONE',  ( 0.000000000000000000, 0.000000000000000000, -1.000000000000000000 ) ) ;
#19899 = CARTESIAN_POINT ( 'NONE',  ( -5.999999999999963585, 8.134310703387671600E-14, -131.3363248654052313 ) ) ;
#19900 = CARTESIAN_POINT ( 'NONE',  ( -4.763139720814407951, -2.750000000000016431, -77.50000000000001421 ) ) ;
#19901 = CARTESIAN_POINT ( 'NONE',  ( 6.000000000000000888, -1.859271017917181981E-14, -79.58632486540520290 ) ) ;
#19902 = CARTESIAN_POINT ( 'NONE',  ( 151.9836002691896226, 4.999999999999989342, -2.071067811865468400 ) ) ;
#19903 = CARTESIAN_POINT ( 'NONE',  ( 161.2178144456196378, -4.907762444546311720, -2.963993361882520272 ) ) ;
#19904 = CARTESIAN_POINT ( 'NONE',  ( 135.1011751345948539, 3.889087296526011706, -3.889087296526011706 ) ) ;
#19905 = CARTESIAN_POINT ( 'NONE',  ( -5.999999999999919176, 1.607695154586804565, -128.4033121635129646 ) ) ;
#19906 = CARTESIAN_POINT ( 'NONE',  ( 0.000000000000000000, 0.000000000000000000, 0.000000000000000000 ) ) ;
#19907 = CARTESIAN_POINT ( 'NONE',  ( -5.999999999999971578, 1.607695154586715303, -138.9033121635130499 ) ) ;
#19908 = EDGE_LOOP ( 'NONE', ( #11501, #30116, #23420, #5679 ) ) ;
#19909 = CARTESIAN_POINT ( 'NONE',  ( 161.7187500000000000, 2.485281374238555774, -6.000000000000005329 ) ) ;
#19910 =( NAMED_UNIT ( * ) SI_UNIT ( $, .STERADIAN. ) SOLID_ANGLE_UNIT ( ) );
#19911 = CARTESIAN_POINT ( 'NONE',  ( -19.49999999999998224, -25.00000000000010658, -8.000000000000007105 ) ) ;
#19912 = CARTESIAN_POINT ( 'NONE',  ( 120.7502832217623308, -1.308140751793640533, 1.308140751793751555 ) ) ;
#19913 = DIRECTION ( 'NONE',  ( -1.000000000000000000, -1.665334536937736783E-16, -2.220446049250315546E-16 ) ) ;
#19914 = VERTEX_POINT ( 'NONE', #23914 ) ;
#19915 = ORIENTED_EDGE ( 'NONE', *, *, #24748, .T. ) ;
#19916 = PRESENTATION_LAYER_ASSIGNMENT (  '', '', ( #8628 ) ) ;
#19917 = ADVANCED_FACE ( 'NONE', ( #12570 ), #19466, .T. ) ;
#19918 = CARTESIAN_POINT ( 'NONE',  ( 4.763139720814407951, -2.749999999999988454, -108.5000000000000426 ) ) ;
#19919 = CARTESIAN_POINT ( 'NONE',  ( 6.000000000000000888, -1.859271017917181981E-14, -46.58632486540520290 ) ) ;
#19920 = CARTESIAN_POINT ( 'NONE',  ( 5.412658773652739619, 3.124999999999988898, -114.6830127018922383 ) ) ;
#19921 = ORIENTED_EDGE ( 'NONE', *, *, #22680, .T. ) ;
#19922 = CARTESIAN_POINT ( 'NONE',  ( -3.464101615137725076, 5.999999999999979572, -140.5863248654051745 ) ) ;
#19923 = CARTESIAN_POINT ( 'NONE',  ( 105.4999999999999147, -2.499999999999919176, 1.110223024625156540E-13 ) ) ;
#19924 = CARTESIAN_POINT ( 'NONE',  ( -3.608439182435115633, 6.249999999999965361, -51.30801270189225249 ) ) ;
#19925 = ORIENTED_EDGE ( 'NONE', *, *, #22715, .F. ) ;
#19926 = CARTESIAN_POINT ( 'NONE',  ( -3.464101615137725076, 5.999999999999979572, -167.5863248654051745 ) ) ;
#19927 = CARTESIAN_POINT ( 'NONE',  ( 3.464101615137757051, -5.999999999999979572, -56.41367513459481131 ) ) ;
#19928 = ADVANCED_FACE ( 'NONE', ( #7757 ), #21766, .T. ) ;
#19929 = DIRECTION ( 'NONE',  ( -7.147005652999508048E-36, 5.642372883946980038E-36, 1.000000000000000000 ) ) ;
#19930 = CARTESIAN_POINT ( 'NONE',  ( 156.0863248654052597, 0.000000000000000000, 5.500000000000005329 ) ) ;
#19931 = CARTESIAN_POINT ( 'NONE',  ( -4.763139720814407951, 2.749999999999946709, -170.7500000000000000 ) ) ;
#19932 = CARTESIAN_POINT ( 'NONE',  ( 119.5624999999998153, -2.499999999999874767, -1.035533905932629173 ) ) ;
#19933 = FACE_OUTER_BOUND ( 'NONE', #8117, .T. ) ;
#19934 = CARTESIAN_POINT ( 'NONE',  ( -5.412658773652684552, -3.125000000000099920, -170.9330127018922099 ) ) ;
#19935 = CARTESIAN_POINT ( 'NONE',  ( -1.000000000000001776, -9.000000000000005329, 4.000000000000005329 ) ) ;
#19936 = CARTESIAN_POINT ( 'NONE',  ( 3.175426480543072749, 5.499999999999865885, -120.1250000000000284 ) ) ;
#19937 = CARTESIAN_POINT ( 'NONE',  ( -4.763139720814407951, -2.750000000000016431, -108.9999999999999858 ) ) ;
#19938 = CARTESIAN_POINT ( 'NONE',  ( -5.999999999999963585, 8.134310703387671600E-14, -142.4136751345948539 ) ) ;
#19939 = CARTESIAN_POINT ( 'NONE',  ( -4.999999999999886313, -71.00000000000002842, -4.000000000000003553 ) ) ;
#19940 = CARTESIAN_POINT ( 'NONE',  ( 135.4618192888269164, -8.932050916383428074, 8.000000000000005329 ) ) ;
#19941 = VERTEX_POINT ( 'NONE', #24056 ) ;
#19942 = CARTESIAN_POINT ( 'NONE',  ( 13.43750000000012612, 1.097466725451619718, -2.649519052838298805 ) ) ;
#19943 = CARTESIAN_POINT ( 'NONE',  ( 118.8749999999998295, 1.767766952966320915, -1.767766952966320915 ) ) ;
#19944 = CARTESIAN_POINT ( 'NONE',  ( 161.5000000000000853, -2.984449860524901688, -5.205099329504969674 ) ) ;
#19945 = CARTESIAN_POINT ( 'NONE',  ( 112.1252832217621460, -5.551115123125782702E-14, -1.849990392679523588 ) ) ;
#19946 = ORIENTED_EDGE ( 'NONE', *, *, #18958, .F. ) ;
#19947 = CARTESIAN_POINT ( 'NONE',  ( -3.175426480542816510, -5.500000000000057732, -161.3750000000000284 ) ) ;
#19948 = CARTESIAN_POINT ( 'NONE',  ( 139.3050748654052313, 5.500000000000012434, 2.278174593052012309 ) ) ;
#19949 = CARTESIAN_POINT ( 'NONE',  ( 109.7497167782375698, 1.308140751793640533, 1.308140751793862577 ) ) ;
#19950 = CARTESIAN_POINT ( 'NONE',  ( -3.608439182435115633, 6.249999999999965361, -84.94198729810781856 ) ) ;
#19951 = CARTESIAN_POINT ( 'NONE',  ( 3.464101615137757051, -5.999999999999979572, -129.3363248654052029 ) ) ;
#19952 = ORIENTED_EDGE ( 'NONE', *, *, #4185, .F. ) ;
#19953 = CARTESIAN_POINT ( 'NONE',  ( 107.0863248654050466, -1.414213562373034527, 1.414213562373145550 ) ) ;
#19954 = EDGE_LOOP ( 'NONE', ( #4723, #9122, #12175, #16066 ) ) ;
#19955 = CARTESIAN_POINT ( 'NONE',  ( 155.5312500000000568, -2.485281374238555774, -6.000000000000005329 ) ) ;
#19956 = EDGE_CURVE ( 'NONE', #12037, #22266, #25910, .T. ) ;
#19957 = CARTESIAN_POINT ( 'NONE',  ( -5.412658773652684552, -3.125000000000099920, -136.4330127018922383 ) ) ;
#19958 = ORIENTED_EDGE ( 'NONE', *, *, #7210, .T. ) ;
#19959 = CARTESIAN_POINT ( 'NONE',  ( 2.775557561562891351E-14, 6.250000000000033751, -124.0669872981078328 ) ) ;
#19960 = CARTESIAN_POINT ( 'NONE',  ( 4.763139720814407951, 2.750000000000002665, -169.7500000000000000 ) ) ;
#19961 = CARTESIAN_POINT ( 'NONE',  ( -3.464101615137725076, 5.999999999999979572, -83.58632486540518869 ) ) ;
#19962 = EDGE_LOOP ( 'NONE', ( #27142, #30148, #3339, #21102 ) ) ;
#19963 = CARTESIAN_POINT ( 'NONE',  ( 14.62500000000008171, -1.414213562372979016, -1.414213562373145550 ) ) ;
#19964 = FACE_OUTER_BOUND ( 'NONE', #20301, .T. ) ;
#19965 = EDGE_CURVE ( 'NONE', #16147, #7342, #29652, .T. ) ;
#19966 = CARTESIAN_POINT ( 'NONE',  ( 0.000000000000000000, 0.000000000000000000, 0.000000000000000000 ) ) ;
#19967 = DIRECTION ( 'NONE',  ( -7.147005652999508048E-36, 5.642372883946980038E-36, 1.000000000000000000 ) ) ;
#19968 = CARTESIAN_POINT ( 'NONE',  ( 116.0002832217622171, -1.308140751793585022, -1.308140751793640533 ) ) ;
#19969 = VECTOR ( 'NONE', #9275, 1000.000000000000000 ) ;
#19970 = CARTESIAN_POINT ( 'NONE',  ( 5.412658773652712085, -3.125000000000086153, -66.06698729810783277 ) ) ;
#19971 = DIRECTION ( 'NONE',  ( -7.147005652999508048E-36, 5.642372883946980038E-36, 1.000000000000000000 ) ) ;
#19972 = CARTESIAN_POINT ( 'NONE',  ( 5.196152422706629359, -2.999999999999988898, -63.78867513459485394 ) ) ;
#19973 = CARTESIAN_POINT ( 'NONE',  ( 147.7574251345948255, -2.278174593051764951, 5.500000000000262013 ) ) ;
#19974 = DIRECTION ( 'NONE',  ( -1.734723475976824844E-16, 1.000000000000000000, 0.000000000000000000 ) ) ;
#19975 = VECTOR ( 'NONE', #2058, 1000.000000000000000 ) ;
#19976 = VECTOR ( 'NONE', #26397, 1000.000000000000000 ) ;
#19977 =( BOUNDED_SURFACE ( )  B_SPLINE_SURFACE ( 3, 2, ( 
 ( #10988, #29840, #2056 ),
 ( #8818, #6498, #25535 ),
 ( #15921, #11459, #30150 ),
 ( #9113, #25222, #22949 ),
 ( #1888, #30302, #11293 ),
 ( #6139, #18003, #22891 ),
 ( #15399, #22591, #29475 ),
 ( #1206, #10615, #8911 ),
 ( #13395, #12943, #1373 ),
 ( #17851, #1522, #10933 ),
 ( #20425, #15554, #29783 ),
 ( #22739, #20283, #1682 ),
 ( #8277, #11080, #8759 ),
 ( #25163, #20583, #4127 ) ),
 .UNSPECIFIED., .F., .F., .T. ) 
 B_SPLINE_SURFACE_WITH_KNOTS ( ( 4, 2, 2, 2, 2, 2, 4 ),
 ( 3, 3 ),
 ( 0.001367763536538648284, 0.002168948318176349387, 0.002569540708995199721, 0.002970133099814050055, 0.003370725490632900390, 0.003771317881451751158, 0.004572502663089452260 ),
 ( 0.000000000000000000, 1.000000000000000000 ),
 .UNSPECIFIED. ) 
 GEOMETRIC_REPRESENTATION_ITEM ( )  RATIONAL_B_SPLINE_SURFACE ( (
 ( 1.000000000000000000, 0.7071067811865475727, 1.000000000000000000),
 ( 1.000000000000000000, 0.7177463599871298783, 1.000000000000000000),
 ( 1.000000000000000000, 0.7309160594376725717, 1.000000000000000000),
 ( 1.000000000000000000, 0.7518982708267778481, 1.000000000000000000),
 ( 1.000000000000000000, 0.7589818330818417502, 1.000000000000000000),
 ( 1.000000000000000000, 0.7730316713029788955, 1.000000000000000000),
 ( 1.000000000000000000, 0.7800646516387804708, 1.000000000000000000),
 ( 1.000000000000000000, 0.7931882794879633325, 1.000000000000000000),
 ( 1.000000000000000000, 0.7993227671868792239, 1.000000000000000000),
 ( 1.000000000000000000, 0.8104421674205291026, 1.000000000000000000),
 ( 1.000000000000000000, 0.8154231620175333983, 1.000000000000000000),
 ( 1.000000000000000000, 0.8275153884601259557, 1.000000000000000000),
 ( 1.000000000000000000, 0.8321080538050803499, 1.000000000000000000),
 ( 1.000000000000000000, 0.8320502943378441651, 1.000000000000000000) ) ) 
 REPRESENTATION_ITEM ( '' )  SURFACE ( )  );
#19978 = CARTESIAN_POINT ( 'NONE',  ( -4.763139720814407951, -2.750000000000016431, -125.5000000000000568 ) ) ;
#19979 = LINE ( 'NONE', #18611, #26290 ) ;
#19980 = ORIENTED_EDGE ( 'NONE', *, *, #17184, .T. ) ;
#19981 = CARTESIAN_POINT ( 'NONE',  ( 24.56250000000011724, 2.649519052838358757, -1.097466725451559322 ) ) ;
#19982 = LINE ( 'NONE', #19827, #16575 ) ;
#19983 = DIRECTION ( 'NONE',  ( 0.000000000000000000, 0.000000000000000000, -1.000000000000000000 ) ) ;
#19984 = CARTESIAN_POINT ( 'NONE',  ( 112.3511751345946976, 2.000000000000061728, 0.8284271247465359034 ) ) ;
#19985 = ORIENTED_EDGE ( 'NONE', *, *, #26629, .T. ) ;
#19986 = AXIS2_PLACEMENT_3D ( 'NONE', #744, #21506, #2732 ) ;
#19987 = CARTESIAN_POINT ( 'NONE',  ( 115.2497167782374419, -1.308140751793557266, -1.308140751793751555 ) ) ;
#19988 = FILL_AREA_STYLE_COLOUR ( '', #28180 ) ;
#19989 = CARTESIAN_POINT ( 'NONE',  ( -5.412658773652684552, -3.125000000000099920, -117.5669872981078328 ) ) ;
#19990 = CARTESIAN_POINT ( 'NONE',  ( 140.0252556714799539, -11.51262782845630817, -4.739386388448244780 ) ) ;
#19991 = CARTESIAN_POINT ( 'NONE',  ( 155.2574251345948255, -2.278174593051826236, 5.500000000000198064 ) ) ;
#19992 = CARTESIAN_POINT ( 'NONE',  ( 115.3124999999998863, -1.035533905932659149, 2.500000000000205169 ) ) ;
#19993 = CARTESIAN_POINT ( 'NONE',  ( 140.8041911596567957, -11.60838231931457365, 4.059228028635632590 ) ) ;
#19994 = CARTESIAN_POINT ( 'NONE',  ( 140.3437500000000284, -6.000000000000005329, -2.485281374238555774 ) ) ;
#19995 = EDGE_CURVE ( 'NONE', #17372, #13456, #21315, .T. ) ;
#19996 = AXIS2_PLACEMENT_3D ( 'NONE', #14480, #12770, #15053 ) ;
#19997 = CARTESIAN_POINT ( 'NONE',  ( 24.56250000000000000, 1.097466725451559322, 2.649519052838419153 ) ) ;
#19998 = CARTESIAN_POINT ( 'NONE',  ( 136.3988248654052313, 3.889087296526011706, 3.889087296526011706 ) ) ;
#19999 = CARTESIAN_POINT ( 'NONE',  ( -3.175426480542816510, 5.499999999999865885, -50.87500000000001421 ) ) ;
#20000 = CARTESIAN_POINT ( 'NONE',  ( -5.196152422706573404, -3.000000000000002665, -59.78867513459484684 ) ) ;
#20001 = EDGE_CURVE ( 'NONE', #15734, #2721, #29836, .T. ) ;
#20002 = DIRECTION ( 'NONE',  ( 0.000000000000000000, 0.000000000000000000, 1.000000000000000000 ) ) ;
#20003 = CARTESIAN_POINT ( 'NONE',  ( 2.775557561562891351E-14, -6.250000000000061284, -71.68301270189225249 ) ) ;
#20004 = CARTESIAN_POINT ( 'NONE',  ( 148.8601497308104058, -3.535533905932725318, -3.535533905932725318 ) ) ;
#20005 = CIRCLE ( 'NONE', #25899, 0.5000000000000004441 ) ;
#20006 = DIRECTION ( 'NONE',  ( -0.2768592823360734867, 0.4367774878841467201, 0.8559055811606609554 ) ) ;
#20007 = CARTESIAN_POINT ( 'NONE',  ( 22.46132486540528106, 1.665334536937734811E-13, -2.500000000000113243 ) ) ;
#20008 = FACE_OUTER_BOUND ( 'NONE', #16632, .T. ) ;
#20009 = CARTESIAN_POINT ( 'NONE',  ( 5.196152422706629359, -2.999999999999988898, -93.78867513459482552 ) ) ;
#20010 = CARTESIAN_POINT ( 'NONE',  ( 4.763139720814407951, -2.749999999999988454, -132.5000000000000000 ) ) ;
#20011 = CARTESIAN_POINT ( 'NONE',  ( 105.5386751345947971, -1.110223024625156540E-13, 2.000000000000001776 ) ) ;
#20012 = CARTESIAN_POINT ( 'NONE',  ( 7.216878364870455975, -6.409875621278545621E-14, -149.3080127018922667 ) ) ;
#20013 = CARTESIAN_POINT ( 'NONE',  ( -6.000000000000000888, 1.067854986875958443E-15, 7.560779664488942560E-35 ) ) ;
#20014 = AXIS2_PLACEMENT_3D ( 'NONE', #13071, #17508, #22404 ) ;
#20015 = ORIENTED_EDGE ( 'NONE', *, *, #2585, .F. ) ;
#20016 = CARTESIAN_POINT ( 'NONE',  ( 3.175426480543072749, 5.499999999999865885, -66.12500000000002842 ) ) ;
#20017 = DIRECTION ( 'NONE',  ( 1.000000000000000000, -5.551115123125773458E-17, -1.260129944081490338E-35 ) ) ;
#20018 = CARTESIAN_POINT ( 'NONE',  ( 4.763139720814407951, 2.750000000000002665, -57.25000000000002132 ) ) ;
#20019 = PRESENTATION_LAYER_ASSIGNMENT (  '', '', ( #24414 ) ) ;
#20020 = DIRECTION ( 'NONE',  ( 0.000000000000000000, 1.000000000000000000, 0.000000000000000000 ) ) ;
#20021 = ORIENTED_EDGE ( 'NONE', *, *, #26836, .F. ) ;
#20022 = CARTESIAN_POINT ( 'NONE',  ( 109.3750000000000142, -1.767766952966320915, 1.767766952966431937 ) ) ;
#20023 = CARTESIAN_POINT ( 'NONE',  ( 144.2812500000000284, 2.485281374238585972, 6.000000000000005329 ) ) ;
#20024 = FACE_OUTER_BOUND ( 'NONE', #6027, .T. ) ;
#20025 = CARTESIAN_POINT ( 'NONE',  ( 15.25000000000012434, 1.110223024625156540E-13, 1.999999999999946265 ) ) ;
#20026 =( LENGTH_UNIT ( ) NAMED_UNIT ( * ) SI_UNIT ( .MILLI., .METRE. ) );
#20027 = CARTESIAN_POINT ( 'NONE',  ( 110.6247167782374987, 1.849990392679551343, 0.000000000000000000 ) ) ;
#20028 = VERTEX_POINT ( 'NONE', #17624 ) ;
#20029 = CARTESIAN_POINT ( 'NONE',  ( 143.0625000000000284, -4.242640687119298093, 4.242640687119298093 ) ) ;
#20030 = CARTESIAN_POINT ( 'NONE',  ( 3.464101615137757051, -5.999999999999979572, -121.8363248654051745 ) ) ;
#20031 = EDGE_LOOP ( 'NONE', ( #3186, #29463, #20725, #12621, #27570, #20681, #10520, #20269, #21395, #6383, #11960, #22412, #4118, #2121, #5163, #12582, #24209, #12895, #24275, #16676, #5396, #5020, #13411, #15550, #10684, #23231, #10733, #16896, #4841, #8895, #925, #12221, #3164, #24392, #14225 ) ) ;
#20032 = EDGE_CURVE ( 'NONE', #19810, #3216, #3534, .T. ) ;
#20033 = EDGE_CURVE ( 'NONE', #6908, #23930, #8208, .T. ) ;
#20034 = CARTESIAN_POINT ( 'NONE',  ( -3.175426480542816510, 5.499999999999865885, -145.3750000000000000 ) ) ;
#20035 = CARTESIAN_POINT ( 'NONE',  ( 5.412658773652712085, -3.125000000000086153, -49.56698729810782567 ) ) ;
#20036 = CARTESIAN_POINT ( 'NONE',  ( 18.62500000000003197, -1.414213562373034527, -1.414213562373090038 ) ) ;
#20037 = VERTEX_POINT ( 'NONE', #6071 ) ;
#20038 = CARTESIAN_POINT ( 'NONE',  ( 3.608439182435180470, 6.249999999999982236, -145.1919872981078470 ) ) ;
#20039 = CARTESIAN_POINT ( 'NONE',  ( 3.175426480543072749, -5.500000000000105693, -77.12500000000001421 ) ) ;
#20040 = CARTESIAN_POINT ( 'NONE',  ( 13.00000000000017764, -1.873492889144789952, -1.873492889145011997 ) ) ;
#20041 = CARTESIAN_POINT ( 'NONE',  ( 7.216878364870455975, -6.409875621278545621E-14, -96.80801270189220986 ) ) ;
#20042 = CARTESIAN_POINT ( 'NONE',  ( -6.350852961085760029, -1.281975124255709124E-13, -152.6250000000000568 ) ) ;
#20043 = CARTESIAN_POINT ( 'NONE',  ( -5.382374809129815141, -9.594851770513439959, -27.68068691953151372 ) ) ;
#20044 = CYLINDRICAL_SURFACE ( 'NONE', #23564, 6.000000000000000888 ) ;
#20045 = CARTESIAN_POINT ( 'NONE',  ( -10.00000000000000178, -19.99999999999998934, -3.000000000000002665 ) ) ;
#20046 = CARTESIAN_POINT ( 'NONE',  ( 0.000000000000000000, 5.999999999999977796, -98.71132486540523132 ) ) ;
#20047 = CARTESIAN_POINT ( 'NONE',  ( 6.000000000000000888, -1.859271017917181981E-14, -114.0863248654052029 ) ) ;
#20048 = CARTESIAN_POINT ( 'NONE',  ( -2.775557561562891351E-14, -5.500000000000115463, -152.2500000000000000 ) ) ;
#20049 = DIRECTION ( 'NONE',  ( -7.147005652999508048E-36, 5.642372883946980038E-36, 1.000000000000000000 ) ) ;
#20050 = CARTESIAN_POINT ( 'NONE',  ( 3.175426480543072749, 5.499999999999865885, -147.1250000000000284 ) ) ;
#20051 = CARTESIAN_POINT ( 'NONE',  ( -4.501142602633604994, 3.771550028943533306, -180.0000000000000568 ) ) ;
#20052 = CARTESIAN_POINT ( 'NONE',  ( 3.175426480543072749, -5.500000000000105693, -90.62500000000001421 ) ) ;
#20053 = CARTESIAN_POINT ( 'NONE',  ( 24.99999999999999289, 5.587541955019290839E-14, -2.000000000000220268 ) ) ;
#20054 = DIRECTION ( 'NONE',  ( 0.000000000000000000, 0.000000000000000000, -1.000000000000000000 ) ) ;
#20055 = CARTESIAN_POINT ( 'NONE',  ( 4.763139720814407951, -2.749999999999988454, -83.00000000000001421 ) ) ;
#20056 = CARTESIAN_POINT ( 'NONE',  ( -5.999999999999963585, 1.780251999655701777E-13, -86.33632486540524553 ) ) ;
#20057 = CARTESIAN_POINT ( 'NONE',  ( 150.8586002691896510, 2.071067811865468400, 4.999999999999989342 ) ) ;
#20058 = DIRECTION ( 'NONE',  ( -1.000000000000000000, -0.000000000000000000, -0.000000000000000000 ) ) ;
#20059 = CYLINDRICAL_SURFACE ( 'NONE', #14976, 1.000000000000000000 ) ;
#20060 = DIRECTION ( 'NONE',  ( -7.147005652999508048E-36, 5.642372883946980038E-36, 1.000000000000000000 ) ) ;
#20061 = CARTESIAN_POINT ( 'NONE',  ( 10.52382486540521711, 1.035533905932929599, -2.499999999999904521 ) ) ;
#20062 = CARTESIAN_POINT ( 'NONE',  ( 6.000000000000000888, -1.859271017917181981E-14, -135.0863248654052029 ) ) ;
#20063 = CARTESIAN_POINT ( 'NONE',  ( 5.196152422706629359, 3.000000000000002665, -75.53867513459483973 ) ) ;
#20064 =( BOUNDED_CURVE ( )  B_SPLINE_CURVE ( 2, ( #15078, #8767, #24420, #19820, #29165, #15237, #1994, #18760, #18456 ),
 .UNSPECIFIED., .F., .T. ) 
 B_SPLINE_CURVE_WITH_KNOTS ( ( 3, 2, 2, 2, 3 ),
 ( 0.4194444444444445086, 0.4203703703703703942, 0.4222222222222222765, 0.4240740740740740478, 0.4249999999999999334 ),
 .UNSPECIFIED. ) 
 CURVE ( )  GEOMETRIC_REPRESENTATION_ITEM ( )  RATIONAL_B_SPLINE_CURVE ( ( 0.9330127018922194093, 0.9330127018922234061, 1.000000000000000000, 0.8660254037844388186, 1.000000000000000000, 0.8660254037844388186, 1.000000000000000000, 0.9330127018922234061, 0.9330127018922194093 ) ) 
 REPRESENTATION_ITEM ( '' )  );
#20065 = ORIENTED_EDGE ( 'NONE', *, *, #23211, .T. ) ;
#20066 = CARTESIAN_POINT ( 'NONE',  ( 3.464101615137852974, 5.999999999999884537, -91.33632486540520290 ) ) ;
#20067 = CARTESIAN_POINT ( 'NONE',  ( 2.775557561562895769E-14, 11.00000000000000000, -14.99152654425661702 ) ) ;
#20068 = CARTESIAN_POINT ( 'NONE',  ( 109.9761751345946124, -0.8284271247461153509, -1.999999999999731104 ) ) ;
#20069 = EDGE_CURVE ( 'NONE', #8862, #20381, #14519, .T. ) ;
#20070 = CARTESIAN_POINT ( 'NONE',  ( 24.93195072464294171, 1.624501552917132496, -1.286961059548207498 ) ) ;
#20071 = ORIENTED_EDGE ( 'NONE', *, *, #16711, .F. ) ;
#20072 = EDGE_CURVE ( 'NONE', #20142, #28820, #16165, .T. ) ;
#20073 =( BOUNDED_CURVE ( )  B_SPLINE_CURVE ( 2, ( #5719, #9910, #677, #19721, #10515, #21586, #10364, #19578, #5420 ),
 .UNSPECIFIED., .F., .F. ) 
 B_SPLINE_CURVE_WITH_KNOTS ( ( 3, 2, 2, 2, 3 ),
 ( 0.9138888888888888618, 0.9148148148148148584, 0.9166666666666666297, 0.9185185185185185119, 0.9194444444444445086 ),
 .UNSPECIFIED. ) 
 CURVE ( )  GEOMETRIC_REPRESENTATION_ITEM ( )  RATIONAL_B_SPLINE_CURVE ( ( 0.9330127018922194093, 0.9330127018922154125, 1.000000000000000000, 0.8660254037844388186, 1.000000000000000000, 0.8660254037844388186, 1.000000000000000000, 0.9330127018922154125, 0.9330127018922194093 ) ) 
 REPRESENTATION_ITEM ( '' )  );
#20074 = UNCERTAINTY_MEASURE_WITH_UNIT (LENGTH_MEASURE( 1.000000000000000082E-05 ), #1701, 'distance_accuracy_value', 'NONE');
#20075 = EDGE_LOOP ( 'NONE', ( #1536, #25257, #29813, #17640 ) ) ;
#20076 = CARTESIAN_POINT ( 'NONE',  ( -6.350852961085760029, -1.281975124255709124E-13, -100.1250000000000568 ) ) ;
#20077 = DIRECTION ( 'NONE',  ( -1.000000000000000000, -1.665334536937736783E-16, -2.220446049250315546E-16 ) ) ;
#20078 = CARTESIAN_POINT ( 'NONE',  ( 7.216878364870455975, -6.409875621278545621E-14, -111.8080127018922241 ) ) ;
#20079 = EDGE_LOOP ( 'NONE', ( #6772, #13211, #10141, #11910 ) ) ;
#20080 = CARTESIAN_POINT ( 'NONE',  ( 147.0863248654052313, 0.000000000000000000, 5.500000000000005329 ) ) ;
#20081 = CARTESIAN_POINT ( 'NONE',  ( 104.4999999999998863, -2.499999999999919176, 0.000000000000000000 ) ) ;
#20082 = CARTESIAN_POINT ( 'NONE',  ( 21.22617513459490368, 2.500000000000144773, -1.035533905932929599 ) ) ;
#20083 = CARTESIAN_POINT ( 'NONE',  ( -7.216878364870328078, 0.000000000000000000, -54.05801270189220276 ) ) ;
#20084 = PRESENTATION_LAYER_ASSIGNMENT (  '', '', ( #11281 ) ) ;
#20085 = ORIENTED_EDGE ( 'NONE', *, *, #21297, .F. ) ;
#20086 = AXIS2_PLACEMENT_3D ( 'NONE', #18014, #27331, #25028 ) ;
#20087 = CARTESIAN_POINT ( 'NONE',  ( 146.5386751345948539, -5.500000000000005329, 0.000000000000000000 ) ) ;
#20088 = CARTESIAN_POINT ( 'NONE',  ( -4.999999999999886313, -70.00000000000001421, 7.500000000000007105 ) ) ;
#20089 = CARTESIAN_POINT ( 'NONE',  ( 0.000000000000000000, 5.499999999999991118, -169.4999999999999716 ) ) ;
#20090 = CARTESIAN_POINT ( 'NONE',  ( 117.5624999999997584, -2.499999999999904521, -1.035533905932508825 ) ) ;
#20091 = CARTESIAN_POINT ( 'NONE',  ( 2.775557561562891351E-14, 6.250000000000033751, -171.4330127018922667 ) ) ;
#20092 = CARTESIAN_POINT ( 'NONE',  ( -1.000000000000000888, 10.00000000000000888, -3.000000000000002665 ) ) ;
#20093 = CARTESIAN_POINT ( 'NONE',  ( -3.175426480542816066, 5.499999999999865885, -106.3750000000000284 ) ) ;
#20094 = CARTESIAN_POINT ( 'NONE',  ( 160.0386751345948539, -5.500000000000005329, 0.000000000000000000 ) ) ;
#20095 = CARTESIAN_POINT ( 'NONE',  ( 0.000000000000000000, 5.499999999999991118, -107.9999999999999858 ) ) ;
#20096 =( NAMED_UNIT ( * ) PLANE_ANGLE_UNIT ( ) SI_UNIT ( $, .RADIAN. ) );
#20097 = CARTESIAN_POINT ( 'NONE',  ( 141.0074251345948255, 2.278174593051965235, -5.500000000000058620 ) ) ;
#20098 = CARTESIAN_POINT ( 'NONE',  ( 6.000000000000000888, -1.607695154586752384, -84.15331216351299304 ) ) ;
#20099 = ORIENTED_EDGE ( 'NONE', *, *, #3850, .F. ) ;
#20100 = CARTESIAN_POINT ( 'NONE',  ( 14.43750000000014033, 1.097466725451739622, -2.649519052838358757 ) ) ;
#20101 = EDGE_CURVE ( 'NONE', #26392, #3053, #16485, .T. ) ;
#20102 = CARTESIAN_POINT ( 'NONE',  ( 120.9374999999996874, 2.500000000000114575, -1.035533905932629173 ) ) ;
#20103 = CARTESIAN_POINT ( 'NONE',  ( 111.1877832217622029, 0.7662911109078588412, -1.849990392679411677 ) ) ;
#20104 = CARTESIAN_POINT ( 'NONE',  ( 6.000000000000000888, 1.743066579297358182E-13, -62.16367513459481131 ) ) ;
#20105 = ORIENTED_EDGE ( 'NONE', *, *, #18882, .T. ) ;
#20106 = CARTESIAN_POINT ( 'NONE',  ( -5.999999999999963585, 1.780251999655701777E-13, -65.33632486540521711 ) ) ;
#20107 = CARTESIAN_POINT ( 'NONE',  ( 5.412658773652739619, 3.124999999999988898, -83.81698729810781856 ) ) ;
#20108 = AXIS2_PLACEMENT_3D ( 'NONE', #15397, #5511, #10612 ) ;
#20109 = CARTESIAN_POINT ( 'NONE',  ( 149.8988248654052313, 3.889087296526011706, 3.889087296526011706 ) ) ;
#20110 = ORIENTED_EDGE ( 'NONE', *, *, #8658, .F. ) ;
#20111 = CARTESIAN_POINT ( 'NONE',  ( 116.2113248654050750, -2.000000000000029310, 0.000000000000000000 ) ) ;
#20112 = EDGE_CURVE ( 'NONE', #28771, #16741, #13466, .T. ) ;
#20113 = AXIS2_PLACEMENT_3D ( 'NONE', #24904, #25052, #1868 ) ;
#20114 = ORIENTED_EDGE ( 'NONE', *, *, #22820, .T. ) ;
#20115 = EDGE_LOOP ( 'NONE', ( #12774, #1061, #2106, #14771 ) ) ;
#20116 = CARTESIAN_POINT ( 'NONE',  ( 157.5937500000000284, 6.000000000000005329, 2.485281374238585972 ) ) ;
#20117 =( BOUNDED_CURVE ( )  B_SPLINE_CURVE ( 2, ( #7396, #3070, #321, #9710, #19093, #28416, #22436, #20130, #12786 ),
 .UNSPECIFIED., .F., .F. ) 
 B_SPLINE_CURVE_WITH_KNOTS ( ( 3, 2, 2, 2, 3 ),
 ( 0.3416666666666666741, 0.3425925925925925597, 0.3444444444444444420, 0.3462962962962963243, 0.3472222222222222099 ),
 .UNSPECIFIED. ) 
 CURVE ( )  GEOMETRIC_REPRESENTATION_ITEM ( )  RATIONAL_B_SPLINE_CURVE ( ( 0.9330127018922194093, 0.9330127018922194093, 1.000000000000000000, 0.8660254037844388186, 1.000000000000000000, 0.8660254037844388186, 1.000000000000000000, 0.9330127018922194093, 0.9330127018922194093 ) ) 
 REPRESENTATION_ITEM ( '' )  );
#20118 = CARTESIAN_POINT ( 'NONE',  ( -3.175426480542816510, 5.499999999999865885, -122.8749999999999858 ) ) ;
#20119 = CARTESIAN_POINT ( 'NONE',  ( 7.216878364870455975, -6.409875621278545621E-14, -135.8080127018922667 ) ) ;
#20120 = EDGE_LOOP ( 'NONE', ( #9158, #22577, #20157, #6588 ) ) ;
#20121 = DIRECTION ( 'NONE',  ( 0.000000000000000000, 0.000000000000000000, 1.000000000000000000 ) ) ;
#20122 = CARTESIAN_POINT ( 'NONE',  ( -3.608439182435052128, -6.250000000000110134, -121.9419872981078043 ) ) ;
#20123 = CARTESIAN_POINT ( 'NONE',  ( -5.196152422706573404, -3.000000000000002665, -135.7113248654052029 ) ) ;
#20124 = CARTESIAN_POINT ( 'NONE',  ( 0.000000000000000000, 5.499999999999991118, -171.0000000000000284 ) ) ;
#20125 = CARTESIAN_POINT ( 'NONE',  ( 159.0865522212051815, -11.33333333501752982, 3.999999995034633216 ) ) ;
#20126 = CARTESIAN_POINT ( 'NONE',  ( 107.6011751345946550, -0.8284271247461753029, 2.000000000000271783 ) ) ;
#20127 = ORIENTED_EDGE ( 'NONE', *, *, #21290, .F. ) ;
#20128 = CARTESIAN_POINT ( 'NONE',  ( 15.75000000000006928, 2.775557561562891351E-13, -2.000000000000057288 ) ) ;
#20129 = CARTESIAN_POINT ( 'NONE',  ( -5.999999999999956479, -1.607695154586745057, -117.7693375672974696 ) ) ;
#20130 = CARTESIAN_POINT ( 'NONE',  ( 6.000000000000000888, 1.607695154586715303, -93.01933756729744118 ) ) ;
#20131 = CARTESIAN_POINT ( 'NONE',  ( 6.000000000000000888, -3.330669073875464691E-16, -7.560779664488942560E-35 ) ) ;
#20132 = CARTESIAN_POINT ( 'NONE',  ( 114.4377832217621318, 1.849990392679562001, 0.7662911109079489913 ) ) ;
#20133 = CARTESIAN_POINT ( 'NONE',  ( 7.216878364870455975, -6.409875621278545621E-14, -68.94198729810780435 ) ) ;
#20134 = CARTESIAN_POINT ( 'NONE',  ( 2.775557561562891351E-14, -6.250000000000061284, -57.31698729810786119 ) ) ;
#20135 = CARTESIAN_POINT ( 'NONE',  ( 3.464101615137757051, -5.999999999999979572, -120.9136751345947971 ) ) ;
#20136 = CARTESIAN_POINT ( 'NONE',  ( 3.464101615137757051, -5.999999999999979572, -63.91367513459485394 ) ) ;
#20137 = CARTESIAN_POINT ( 'NONE',  ( 148.3199251345948255, -2.278174593052012309, -5.500000000000012434 ) ) ;
#20138 = CARTESIAN_POINT ( 'NONE',  ( 107.2113248654050608, -1.999999999999946265, 0.000000000000000000 ) ) ;
#20139 = AXIS2_PLACEMENT_3D ( 'NONE', #24293, #14126, #4549 ) ;
#20140 = CARTESIAN_POINT ( 'NONE',  ( 3.175426480543072749, -5.500000000000105693, -126.6250000000000000 ) ) ;
#20141 = ADVANCED_FACE ( 'NONE', ( #26945 ), #28946, .T. ) ;
#20142 = VERTEX_POINT ( 'NONE', #7910 ) ;
#20143 = CARTESIAN_POINT ( 'NONE',  ( 23.75000000000013145, 1.873492889145067508, 1.873492889144734441 ) ) ;
#20144 = EDGE_CURVE ( 'NONE', #23494, #15499, #5362, .T. ) ;
#20145 = CARTESIAN_POINT ( 'NONE',  ( 5.196152422706629359, 3.000000000000002665, -119.9613248654052313 ) ) ;
#20146 = FACE_OUTER_BOUND ( 'NONE', #24176, .T. ) ;
#20147 = CARTESIAN_POINT ( 'NONE',  ( 5.999999999999999112, 2.951592740943527306E-14, -161.1636751345949108 ) ) ;
#20148 = CARTESIAN_POINT ( 'NONE',  ( 139.2336002691896510, -4.999999999999989342, 2.071067811865468400 ) ) ;
#20149 = ORIENTED_EDGE ( 'NONE', *, *, #16510, .T. ) ;
#20150 = CARTESIAN_POINT ( 'NONE',  ( 114.6247167782376124, 1.849990392679523588, 0.000000000000000000 ) ) ;
#20151 = DIRECTION ( 'NONE',  ( -7.147005652999508048E-36, 5.642372883946980038E-36, 1.000000000000000000 ) ) ;
#20152 = LINE ( 'NONE', #28057, #866 ) ;
#20153 = CARTESIAN_POINT ( 'NONE',  ( -3.608439182435115633, 6.249999999999965361, -116.4419872981078470 ) ) ;
#20154 = FACE_OUTER_BOUND ( 'NONE', #20843, .T. ) ;
#20155 = ADVANCED_FACE ( 'NONE', ( #10715 ), #20059, .F. ) ;
#20156 = CARTESIAN_POINT ( 'NONE',  ( 115.0624999999998153, 2.499999999999994671, 1.035533905932929599 ) ) ;
#20157 = ORIENTED_EDGE ( 'NONE', *, *, #15348, .T. ) ;
#20158 = CARTESIAN_POINT ( 'NONE',  ( 21.58632486540529172, 1.767766952966598470, -1.767766952966487448 ) ) ;
#20159 = CARTESIAN_POINT ( 'NONE',  ( 142.7812500000000568, 2.485281374238585972, 6.000000000000005329 ) ) ;
#20160 = AXIS2_PLACEMENT_3D ( 'NONE', #9850, #12333, #18945 ) ;
#20161 = ORIENTED_EDGE ( 'NONE', *, *, #11869, .T. ) ;
#20162 = ORIENTED_EDGE ( 'NONE', *, *, #8515, .F. ) ;
#20163 = CARTESIAN_POINT ( 'NONE',  ( 135.9300748654051745, 2.278174593051671692, -5.500000000000352607 ) ) ;
#20164 = CARTESIAN_POINT ( 'NONE',  ( -4.763139720814407951, -2.750000000000016431, -52.00000000000004263 ) ) ;
#20165 = CARTESIAN_POINT ( 'NONE',  ( 6.000000000000000888, 1.743066579297358182E-13, -96.08632486540521711 ) ) ;
#20166 = CARTESIAN_POINT ( 'NONE',  ( 135.8511751345948255, -3.889087296526011706, 3.889087296526011706 ) ) ;
#20167 = CARTESIAN_POINT ( 'NONE',  ( 2.775557561562891351E-14, -6.250000000000061284, -74.68301270189226670 ) ) ;
#20168 =( BOUNDED_CURVE ( )  B_SPLINE_CURVE ( 2, ( #5118, #12690, #17292, #22023, #959, #7878, #21881, #26612, #9909 ),
 .UNSPECIFIED., .F., .T. ) 
 B_SPLINE_CURVE_WITH_KNOTS ( ( 3, 2, 2, 2, 3 ),
 ( 0.6194444444444444642, 0.6203703703703703498, 0.6222222222222222321, 0.6240740740740741144, 0.6250000000000000000 ),
 .UNSPECIFIED. ) 
 CURVE ( )  GEOMETRIC_REPRESENTATION_ITEM ( )  RATIONAL_B_SPLINE_CURVE ( ( 0.9330127018922194093, 0.9330127018922234061, 1.000000000000000000, 0.8660254037844388186, 1.000000000000000000, 0.8660254037844388186, 1.000000000000000000, 0.9330127018922194093, 0.9330127018922194093 ) ) 
 REPRESENTATION_ITEM ( '' )  );
#20169 = CARTESIAN_POINT ( 'NONE',  ( -5.196152422706573404, -3.000000000000002665, -173.2113248654052597 ) ) ;
#20170 = AXIS2_PLACEMENT_3D ( 'NONE', #10199, #14816, #17125 ) ;
#20171 = CARTESIAN_POINT ( 'NONE',  ( 150.9226497308104058, 5.000000000000004441, 0.000000000000000000 ) ) ;
#20172 = CARTESIAN_POINT ( 'NONE',  ( 6.000000000000000888, 5.577813053751546416E-15, -177.6636751345948255 ) ) ;
#20173 = SURFACE_STYLE_USAGE ( .BOTH. , #27054 ) ;
#20174 = CARTESIAN_POINT ( 'NONE',  ( -5.999999999999919176, 1.607695154586804565, -104.4033121635129930 ) ) ;
#20175 = CARTESIAN_POINT ( 'NONE',  ( -4.763139720814407951, -2.750000000000016431, -131.5000000000000000 ) ) ;
#20176 = DIRECTION ( 'NONE',  ( 0.000000000000000000, 0.000000000000000000, 1.000000000000000000 ) ) ;
#20177 = CARTESIAN_POINT ( 'NONE',  ( -3.608439182435052128, -6.250000000000110134, -146.8080127018922667 ) ) ;
#20178 = VERTEX_POINT ( 'NONE', #18230 ) ;
#20179 = EDGE_CURVE ( 'NONE', #6130, #6918, #20361, .T. ) ;
#20180 = AXIS2_PLACEMENT_3D ( 'NONE', #12823, #3100, #26150 ) ;
#20181 = CARTESIAN_POINT ( 'NONE',  ( -2.775557561562891351E-14, -5.500000000000115463, -65.25000000000002842 ) ) ;
#20182 = DIRECTION ( 'NONE',  ( 1.000000000000000000, -5.551115123125773458E-17, -1.260129944081490338E-35 ) ) ;
#20183 = CARTESIAN_POINT ( 'NONE',  ( -5.196152422706573404, -3.000000000000002665, -174.7113248654052029 ) ) ;
#20184 = ORIENTED_EDGE ( 'NONE', *, *, #13663, .T. ) ;
#20185 = VECTOR ( 'NONE', #21482, 1000.000000000000000 ) ;
#20186 = CARTESIAN_POINT ( 'NONE',  ( 108.8749999999999574, 1.767766952966265404, -1.767766952966320915 ) ) ;
#20187 = CARTESIAN_POINT ( 'NONE',  ( 146.0625000000000284, -4.242640687119298093, 4.242640687119298093 ) ) ;
#20188 = CARTESIAN_POINT ( 'NONE',  ( 14.43750000000014033, -1.999999999999851674, 0.8284271247462955401 ) ) ;
#20189 = AXIS2_PLACEMENT_3D ( 'NONE', #28528, #26235, #7497 ) ;
#20190 = CARTESIAN_POINT ( 'NONE',  ( 0.000000000000000000, -5.999999999999991118, -49.03867513459481131 ) ) ;
#20191 = EDGE_CURVE ( 'NONE', #20568, #13841, #13635, .T. ) ;
#20192 = ADVANCED_FACE ( 'NONE', ( #6683 ), #20674, .F. ) ;
#20193 = EDGE_LOOP ( 'NONE', ( #13294, #19952, #18207, #12552 ) ) ;
#20194 = CARTESIAN_POINT ( 'NONE',  ( 136.5937500000000853, 6.000000000000005329, 2.485281374238585972 ) ) ;
#20195 = CARTESIAN_POINT ( 'NONE',  ( 161.2468146748790332, -4.679509648744853756, 3.350853646919034201 ) ) ;
#20196 = ORIENTED_EDGE ( 'NONE', *, *, #25800, .T. ) ;
#20197 = CARTESIAN_POINT ( 'NONE',  ( -2.775557561562891351E-14, -5.500000000000115463, -143.2500000000000000 ) ) ;
#20198 = VERTEX_POINT ( 'NONE', #23139 ) ;
#20199 = CARTESIAN_POINT ( 'NONE',  ( 3.608439182435180470, -6.249999999999997335, -48.19198729810783277 ) ) ;
#20200 = CARTESIAN_POINT ( 'NONE',  ( 18.43749999999999645, -1.999999999999971800, 0.8284271247462354770 ) ) ;
#20201 = ORIENTED_EDGE ( 'NONE', *, *, #15752, .F. ) ;
#20202 = CARTESIAN_POINT ( 'NONE',  ( -3.175426480542816510, -5.500000000000057732, -77.37500000000001421 ) ) ;
#20203 = TOROIDAL_SURFACE ( 'NONE', #557, 14.49999999999999289, 0.5000000000000000000 ) ;
#20204 = CARTESIAN_POINT ( 'NONE',  ( -5.412658773652739619, 3.124999999999975131, -93.18301270189222407 ) ) ;
#20205 = ORIENTED_EDGE ( 'NONE', *, *, #26102, .F. ) ;
#20206 = CARTESIAN_POINT ( 'NONE',  ( -0.8029667472979058473, -10.97248951867538302, -19.05056182979571133 ) ) ;
#20207 = CARTESIAN_POINT ( 'NONE',  ( 125.0000000000000568, -55.00000000000000711, -7.500000000000007105 ) ) ;
#20208 = CARTESIAN_POINT ( 'NONE',  ( 106.7113248654050324, 2.000000000000001776, 1.110223024625156540E-13 ) ) ;
#20209 = CARTESIAN_POINT ( 'NONE',  ( 140.0769230769231228, -11.53846153846155254, -4.615384615384604317 ) ) ;
#20210 = DIRECTION ( 'NONE',  ( 0.000000000000000000, 0.000000000000000000, -1.000000000000000000 ) ) ;
#20211 = PRODUCT_CONTEXT ( 'NONE', #8906, 'mechanical' ) ;
#20212 = CARTESIAN_POINT ( 'NONE',  ( 6.350852961086080661, -9.614813431917819062E-14, -153.3749999999999716 ) ) ;
#20213 = DIRECTION ( 'NONE',  ( -7.147005652999508048E-36, 5.642372883946980038E-36, 1.000000000000000000 ) ) ;
#20214 = AXIS2_PLACEMENT_3D ( 'NONE', #12538, #674, #28912 ) ;
#20215 = CARTESIAN_POINT ( 'NONE',  ( -2.027308962371316525, 5.280605156496299024, -179.9999999999999716 ) ) ;
#20216 = AXIS2_PLACEMENT_3D ( 'NONE', #11317, #9284, #16390 ) ;
#20217 =( BOUNDED_CURVE ( )  B_SPLINE_CURVE ( 2, ( #9741, #13779, #26006, #30318, #28149, #25706, #16536, #25551, #23120 ),
 .UNSPECIFIED., .F., .F. ) 
 B_SPLINE_CURVE_WITH_KNOTS ( ( 3, 2, 2, 2, 3 ),
 ( 0.7375000000000002665, 0.7437500000000000222, 0.7499999999999997780, 0.7562499999999995337, 0.7624999999999992895 ),
 .UNSPECIFIED. ) 
 CURVE ( )  GEOMETRIC_REPRESENTATION_ITEM ( )  RATIONAL_B_SPLINE_CURVE ( ( 0.9999999999999973355, 0.9238795325112894030, 1.000000000000000000, 0.9238795325112867385, 1.000000000000000000, 0.9238795325112867385, 1.000000000000000000, 0.9238795325112948431, 0.9999999999999918954 ) ) 
 REPRESENTATION_ITEM ( '' )  );
#20218 = EDGE_CURVE ( 'NONE', #4196, #18433, #18689, .T. ) ;
#20219 = CARTESIAN_POINT ( 'NONE',  ( 0.000000000000000000, 0.000000000000000000, -183.0000000000000000 ) ) ;
#20220 = CARTESIAN_POINT ( 'NONE',  ( 3.175426480543072749, -5.500000000000105693, -75.62500000000000000 ) ) ;
#20221 = AXIS2_PLACEMENT_3D ( 'NONE', #4670, #11790, #23586 ) ;
#20222 = CARTESIAN_POINT ( 'NONE',  ( 154.5148502691896510, -3.535533905932725318, -3.535533905932725318 ) ) ;
#20223 = CARTESIAN_POINT ( 'NONE',  ( -3.464101615137725076, 5.999999999999979572, -106.0863248654052313 ) ) ;
#20224 = DIRECTION ( 'NONE',  ( 0.000000000000000000, 0.000000000000000000, -1.000000000000000000 ) ) ;
#20225 = CARTESIAN_POINT ( 'NONE',  ( 114.5238248654049755, 0.8284271247463257382, -1.999999999999791278 ) ) ;
#20226 = CARTESIAN_POINT ( 'NONE',  ( 22.56250000000011724, -1.999999999999851674, -0.8284271247462354770 ) ) ;
#20227 = CARTESIAN_POINT ( 'NONE',  ( 111.8988248654051034, 0.8284271247462654530, 2.000000000000151879 ) ) ;
#20228 = AXIS2_PLACEMENT_3D ( 'NONE', #15906, #4166, #15437 ) ;
#20229 = DIRECTION ( 'NONE',  ( -8.326672684688675286E-17, -2.081668171172168821E-17, 1.000000000000000000 ) ) ;
#20230 = EDGE_CURVE ( 'NONE', #13576, #7302, #26713, .T. ) ;
#20231 = CARTESIAN_POINT ( 'NONE',  ( -5.999999999999964473, 9.063946212346262433E-15, -173.9136751345948255 ) ) ;
#20232 = ORIENTED_EDGE ( 'NONE', *, *, #22403, .F. ) ;
#20233 = SURFACE_STYLE_FILL_AREA ( #24353 ) ;
#20234 = CARTESIAN_POINT ( 'NONE',  ( -5.999999999999919176, 1.607695154586804565, -72.90331216351302146 ) ) ;
#20235 = CARTESIAN_POINT ( 'NONE',  ( 116.6877832217621460, -0.7662911109077388261, 1.849990392679712103 ) ) ;
#20236 = VECTOR ( 'NONE', #12246, 1000.000000000000000 ) ;
#20237 = ORIENTED_EDGE ( 'NONE', *, *, #7025, .T. ) ;
#20238 = CARTESIAN_POINT ( 'NONE',  ( -4.763139720814407951, -2.750000000000016431, -94.00000000000002842 ) ) ;
#20239 = CARTESIAN_POINT ( 'NONE',  ( 0.000000000000000000, 0.000000000000000000, 0.000000000000000000 ) ) ;
#20240 = CARTESIAN_POINT ( 'NONE',  ( -5.412658773652739619, 3.124999999999975131, -115.6830127018922383 ) ) ;
#20241 = EDGE_LOOP ( 'NONE', ( #7190, #3455, #8381, #9995 ) ) ;
#20242 = CARTESIAN_POINT ( 'NONE',  ( 6.000000000000000888, 7.762456499804235646E-14, -132.6636751345948539 ) ) ;
#20243 = FACE_OUTER_BOUND ( 'NONE', #9305, .T. ) ;
#20244 = CARTESIAN_POINT ( 'NONE',  ( 7.216878364870455975, -6.409875621278545621E-14, -48.80801270189224539 ) ) ;
#20245 = VERTEX_POINT ( 'NONE', #13954 ) ;
#20246 = CARTESIAN_POINT ( 'NONE',  ( -5.999999999999962697, 3.323446944526963260E-14, -159.8363248654052597 ) ) ;
#20247 = CARTESIAN_POINT ( 'NONE',  ( 146.9136751345948539, 0.000000000000000000, -5.500000000000005329 ) ) ;
#20248 = CARTESIAN_POINT ( 'NONE',  ( 0.000000000000000000, 0.000000000000000000, 0.000000000000000000 ) ) ;
#20249 = CARTESIAN_POINT ( 'NONE',  ( 4.763139720814407951, 2.750000000000002665, -163.7500000000000000 ) ) ;
#20250 = CARTESIAN_POINT ( 'NONE',  ( 117.1249999999999432, 1.767766952966320915, 1.767766952966431937 ) ) ;
#20251 = CARTESIAN_POINT ( 'NONE',  ( 6.000000000000000888, 1.743066579297358182E-13, -108.0863248654051745 ) ) ;
#20252 = ADVANCED_FACE ( 'NONE', ( #15947 ), #25571, .T. ) ;
#20253 = CARTESIAN_POINT ( 'NONE',  ( -4.763139720814407951, 2.749999999999946709, -109.2500000000000142 ) ) ;
#20254 = CARTESIAN_POINT ( 'NONE',  ( 23.52382486540536277, 1.035533905932869425, -2.499999999999904521 ) ) ;
#20255 =( BOUNDED_CURVE ( )  B_SPLINE_CURVE ( 2, ( #21140, #15953, #18696, #6991, #30032, #2388, #28170, #11800, #28018 ),
 .UNSPECIFIED., .F., .T. ) 
 B_SPLINE_CURVE_WITH_KNOTS ( ( 3, 2, 2, 2, 3 ),
 ( 0.3805555555555555358, 0.3814814814814815325, 0.3833333333333333037, 0.3851851851851851860, 0.3861111111111111827 ),
 .UNSPECIFIED. ) 
 CURVE ( )  GEOMETRIC_REPRESENTATION_ITEM ( )  RATIONAL_B_SPLINE_CURVE ( ( 0.9330127018922194093, 0.9330127018922154125, 1.000000000000000000, 0.8660254037844388186, 1.000000000000000000, 0.8660254037844388186, 1.000000000000000000, 0.9330127018922154125, 0.9330127018922194093 ) ) 
 REPRESENTATION_ITEM ( '' )  );
#20256 = EDGE_CURVE ( 'NONE', #17671, #15465, #12072, .T. ) ;
#20257 = CARTESIAN_POINT ( 'NONE',  ( 4.763139720814407951, -2.749999999999988454, -107.0000000000000426 ) ) ;
#20258 = CARTESIAN_POINT ( 'NONE',  ( 11.47617513459495342, 1.035533905932869425, 2.499999999999844569 ) ) ;
#20259 = CARTESIAN_POINT ( 'NONE',  ( 0.000000000000000000, 5.999999999999977796, -118.2113248654052029 ) ) ;
#20260 = VERTEX_POINT ( 'NONE', #27548 ) ;
#20261 = CARTESIAN_POINT ( 'NONE',  ( 16.56250000000004974, 2.649519052838358757, -1.097466725451559322 ) ) ;
#20262 = CARTESIAN_POINT ( 'NONE',  ( 115.5624999999999005, -2.499999999999934719, -1.035533905932568777 ) ) ;
#20263 = CARTESIAN_POINT ( 'NONE',  ( 109.0627832217621176, -0.7662911109076785410, -1.849990392679171425 ) ) ;
#20264 =( BOUNDED_CURVE ( )  B_SPLINE_CURVE ( 2, ( #19944, #20514, #29293, #17663, #5952, #29867, #16699, #4530, #12092, #26021, #21434, #366, #28318, #21280, #4969, #9298, #7296, #2240, #25575, #14251, #18840, #18995, #14404, #11642, #13955, #23296, #18690, #11794, #28465, #23738, #2668, #2384, #20988, #23589, #28166, #30335, #16105, #9755, #28012, #19131, #6985, #21135, #25408, #4369, #13797, #72, #16404, #219, #23141, #2086, #11490, #20831, #30179, #9457, #9145, #7136, #18537, #23445, #9605, #25728, #27864, #16554, #25874, #6830, #16256, #4673, #14109, #4826, #2526, #11953, #29064, #7433, #7576, #16989, #10214, #9908, #26748, #3258, #21583, #12689, #5117, #26313, #515, #12836, #17435, #19718, #8029, #22178, #3411, #17136, #10360, #19865, #26611, #26168, #22022, #17291, #2822, #26461, #2966, #818, #5417, #23877, #21880, #14829, #5715, #10511, #15126, #24172, #5566, #28606, #24457, #19284, #958, #1111, #12389, #16844, #14537, #12245, #5269, #24022, #14969, #3115, #14677, #21734, #673, #24309, #10059, #19435, #28760, #7728, #12537, #19576, #28911, #7877, #10834, #15288, #25221, #15609, #4189, #11130, #22642, #15452, #22492, #22331, #12994, #29839, #17744, #13604, #8817, #22948, #1887, #20478, #4028, #18202, #1425, #27520, #24778, #8334, #18056, #11292, #13153, #6497, #13300, #15920, #6193, #13447, #20187, #1265, #29210, #29539, #1581, #10987, #27068, #1735, #20332, #3563, #8172, #29683, #17589, #8496, #8655, #27371, #10676, #26905, #25071, #20023, #22795, #5869, #24613, #29370, #17902, #6334, #6033, #24922, #3724, #27219, #3872, #15764, #2204, #25534, #13760, #4792, #33, #16074, #9265, #16222, #14075, #18658, #4937, #9421, #14368, #28134, #4338, #25692, #16523, #6951, #25845, #11919, #23556, #18809, #4642, #6655, #23107, #30149, #7103, #27977, #16369, #14218, #23411, #2494, #9572, #23706, #21248, #16669, #2640, #28283, #20647, #18966, #25376, #189, #2055, #11458, #7261, #25992, #20802, #9112, #18358, #29993, #6798, #13920, #18507, #27830, #8969, #4497, #27675, #23263, #11609, #20950, #30301, #2356, #11759, #21104, #19105, #5533, #12506, #14646, #26285, #14939, #927, #28579, #9875, #481, #23993, #7696, #24431, #3224, #24277, #28725, #16957, #17257, #29034, #8000, #5681, #10326, #7408 ),
 .UNSPECIFIED., .F., .T. ) 
 B_SPLINE_CURVE_WITH_KNOTS ( ( 3, 2, 2, 2, 2, 2, 2, 2, 2, 2, 2, 2, 2, 2, 2, 2, 2, 2, 2, 2, 2, 2, 2, 2, 2, 2, 2, 2, 2, 2, 2, 2, 2, 2, 2, 2, 2, 2, 2, 2, 2, 2, 2, 2, 2, 2, 2, 2, 2, 2, 2, 2, 2, 2, 2, 2, 2, 2, 2, 2, 2, 2, 2, 2, 2, 2, 2, 2, 2, 2, 2, 2, 2, 2, 2, 2, 2, 2, 2, 2, 2, 2, 2, 2, 2, 2, 2, 2, 2, 2, 2, 2, 2, 2, 2, 2, 2, 2, 2, 2, 2, 2, 2, 2, 2, 2, 2, 2, 2, 2, 2, 2, 2, 2, 2, 2, 2, 2, 2, 2, 2, 2, 2, 2, 2, 2, 2, 2, 2, 2, 2, 2, 2, 2, 2, 2, 2, 2, 2, 2, 2, 2, 3 ),
 ( 0.01663113027555142287, 0.01874999999999999931, 0.02500000000000000139, 0.03125000000000000000, 0.03749999999999999861, 0.04374999999999999722, 0.05000000000000000278, 0.05625000000000000139, 0.06249999999999999306, 0.06875000000000000555, 0.07499999999999998335, 0.08125000000000000278, 0.08749999999999998057, 0.09375000000000000000, 0.09999999999999999167, 0.1062499999999999833, 0.1125000000000000028, 0.1187499999999999806, 0.1249999999999999861, 0.1312499999999999778, 0.1375000000000000111, 0.1437499999999999889, 0.1499999999999999667, 0.1562500000000000000, 0.1624999999999999778, 0.1687500000000000111, 0.1749999999999999889, 0.1812499999999999667, 0.1875000000000000000, 0.1937499999999999778, 0.2000000000000000111, 0.2062499999999999889, 0.2124999999999999667, 0.2187500000000000000, 0.2249999999999999778, 0.2312500000000000111, 0.2374999999999999889, 0.2437499999999999667, 0.2500000000000000000, 0.2562499999999999778, 0.2625000000000000111, 0.2687499999999999334, 0.2749999999999999667, 0.2812500000000000000, 0.2874999999999999223, 0.2937499999999999556, 0.2999999999999999889, 0.3062499999999999667, 0.3124999999999999445, 0.3187499999999999778, 0.3249999999999999556, 0.3312499999999999334, 0.3375000000000000222, 0.3437499999999999445, 0.3499999999999999223, 0.3562500000000000111, 0.3624999999999999334, 0.3687499999999999667, 0.3750000000000000000, 0.3812499999999999223, 0.3874999999999999556, 0.3937499999999999334, 0.3999999999999999667, 0.4062499999999999445, 0.4124999999999999223, 0.4187499999999999556, 0.4249999999999999334, 0.4312499999999999667, 0.4374999999999999445, 0.4437499999999999223, 0.4499999999999999556, 0.4562499999999999334, 0.4624999999999999667, 0.4687499999999999445, 0.4749999999999999223, 0.4812499999999999556, 0.4874999999999999334, 0.4937499999999999667, 0.4999999999999999445, 0.5062499999999999778, 0.5124999999999998446, 0.5187500000000000444, 0.5250000000000000222, 0.5312499999999998890, 0.5374999999999998668, 0.5437499999999999556, 0.5499999999999999334, 0.5562499999999999112, 0.5625000000000000000, 0.5687499999999998668, 0.5749999999999998446, 0.5812499999999999334, 0.5874999999999999112, 0.5937499999999998890, 0.5999999999999999778, 0.6062499999999998446, 0.6124999999999999334, 0.6187500000000000222, 0.6249999999999998890, 0.6312499999999998668, 0.6374999999999999556, 0.6437499999999999334, 0.6499999999999999112, 0.6562500000000000000, 0.6624999999999998668, 0.6687499999999998446, 0.6750000000000000444, 0.6812499999999999112, 0.6874999999999998890, 0.6937499999999998668, 0.6999999999999998446, 0.7062499999999999334, 0.7125000000000000222, 0.7187499999999998890, 0.7249999999999998668, 0.7312499999999998446, 0.7374999999999999334, 0.7437499999999999112, 0.7499999999999998890, 0.7562499999999998668, 0.7624999999999998446, 0.7687500000000000444, 0.7749999999999999112, 0.7812499999999998890, 0.7874999999999998668, 0.7937499999999998446, 0.7999999999999999334, 0.8062499999999999112, 0.8124999999999998890, 0.8187499999999998668, 0.8249999999999998446, 0.8312499999999999334, 0.8374999999999999112, 0.8437499999999998890, 0.8499999999999998668, 0.8562499999999998446, 0.8624999999999999334, 0.8687499999999999112, 0.8749999999999998890, 0.8812499999999998668, 0.8874999999999998446, 0.8937499999999999334, 0.8999999999999999112 ),
 .UNSPECIFIED. ) 
 CURVE ( )  GEOMETRIC_REPRESENTATION_ITEM ( )  RATIONAL_B_SPLINE_CURVE ( ( 0.9658850645339760455, 0.9741937033643669475, 1.000000000000000000, 0.9238795325112867385, 1.000000000000000000, 0.9238795325112867385, 1.000000000000000000, 0.9238795325112867385, 1.000000000000000000, 0.9238795325112867385, 1.000000000000000000, 0.9238795325112867385, 1.000000000000000000, 0.9238795325112867385, 1.000000000000000000, 0.9238795325112867385, 1.000000000000000000, 0.9238795325112867385, 1.000000000000000000, 0.9238795325112867385, 1.000000000000000000, 0.9238795325112867385, 1.000000000000000000, 0.9238795325112867385, 1.000000000000000000, 0.9238795325112867385, 1.000000000000000000, 0.9238795325112867385, 1.000000000000000000, 0.9238795325112867385, 1.000000000000000000, 0.9238795325112867385, 1.000000000000000000, 0.9238795325112867385, 1.000000000000000000, 0.9238795325112867385, 1.000000000000000000, 0.9238795325112867385, 1.000000000000000000, 0.9238795325112867385, 1.000000000000000000, 0.9238795325112867385, 1.000000000000000000, 0.9238795325112867385, 1.000000000000000000, 0.9238795325112867385, 1.000000000000000000, 0.9238795325112867385, 1.000000000000000000, 0.9238795325112867385, 1.000000000000000000, 0.9238795325112867385, 1.000000000000000000, 0.9238795325112867385, 1.000000000000000000, 0.9238795325112867385, 1.000000000000000000, 0.9238795325112867385, 1.000000000000000000, 0.9238795325112867385, 1.000000000000000000, 0.9238795325112867385, 1.000000000000000000, 0.9238795325112867385, 1.000000000000000000, 0.9238795325112867385, 1.000000000000000000, 0.9238795325112867385, 1.000000000000000000, 0.9238795325112867385, 1.000000000000000000, 0.9238795325112867385, 1.000000000000000000, 0.9238795325112867385, 1.000000000000000000, 0.9238795325112867385, 1.000000000000000000, 0.9238795325112867385, 1.000000000000000000, 0.9238795325112867385, 1.000000000000000000, 0.9238795325112867385, 1.000000000000000000, 0.9238795325112867385, 1.000000000000000000, 0.9238795325112867385, 1.000000000000000000, 0.9238795325112867385, 1.000000000000000000, 0.9238795325112867385, 1.000000000000000000, 0.9238795325112867385, 1.000000000000000000, 0.9238795325112867385, 1.000000000000000000, 0.9238795325112867385, 1.000000000000000000, 0.9238795325112867385, 1.000000000000000000, 0.9238795325112867385, 1.000000000000000000, 0.9238795325112867385, 1.000000000000000000, 0.9238795325112867385, 1.000000000000000000, 0.9238795325112867385, 1.000000000000000000, 0.9238795325112867385, 1.000000000000000000, 0.9238795325112867385, 1.000000000000000000, 0.9238795325112867385, 1.000000000000000000, 0.9238795325112867385, 1.000000000000000000, 0.9238795325112867385, 1.000000000000000000, 0.9238795325112867385, 1.000000000000000000, 0.9238795325112867385, 1.000000000000000000, 0.9238795325112867385, 1.000000000000000000, 0.9238795325112867385, 1.000000000000000000, 0.9238795325112867385, 1.000000000000000000, 0.9238795325112867385, 1.000000000000000000, 0.9238795325112867385, 1.000000000000000000, 0.9238795325112867385, 1.000000000000000000, 0.9238795325112867385, 1.000000000000000000, 0.9238795325112867385, 1.000000000000000000, 0.9238795325112867385, 1.000000000000000000, 0.9238795325112867385, 1.000000000000000000, 0.9238795325112867385, 1.000000000000000000, 0.9238795325112867385, 1.000000000000000000, 0.9238795325112867385, 1.000000000000000000, 0.9238795325112867385, 1.000000000000000000, 0.9238795325112867385, 1.000000000000000000, 0.9238795325112867385, 1.000000000000000000, 0.9238795325112867385, 1.000000000000000000, 0.9238795325112867385, 1.000000000000000000, 0.9238795325112867385, 1.000000000000000000, 0.9238795325112867385, 1.000000000000000000, 0.9238795325112867385, 1.000000000000000000, 0.9238795325112867385, 1.000000000000000000, 0.9238795325112867385, 1.000000000000000000, 0.9238795325112867385, 1.000000000000000000, 0.9238795325112867385, 1.000000000000000000, 0.9238795325112867385, 1.000000000000000000, 0.9238795325112867385, 1.000000000000000000, 0.9238795325112867385, 1.000000000000000000, 0.9238795325112867385, 1.000000000000000000, 0.9238795325112867385, 1.000000000000000000, 0.9238795325112867385, 1.000000000000000000, 0.9238795325112867385, 1.000000000000000000, 0.9238795325112867385, 1.000000000000000000, 0.9238795325112867385, 1.000000000000000000, 0.9238795325112867385, 1.000000000000000000, 0.9238795325112867385, 1.000000000000000000, 0.9238795325112867385, 1.000000000000000000, 0.9238795325112867385, 1.000000000000000000, 0.9238795325112867385, 1.000000000000000000, 0.9238795325112867385, 1.000000000000000000, 0.9238795325112867385, 1.000000000000000000, 0.9238795325112867385, 1.000000000000000000, 0.9238795325112867385, 1.000000000000000000, 0.9238795325112867385, 1.000000000000000000, 0.9238795325112867385, 1.000000000000000000, 0.9238795325112867385, 1.000000000000000000, 0.9238795325112867385, 1.000000000000000000, 0.9238795325112867385, 1.000000000000000000, 0.9238795325112867385, 1.000000000000000000, 0.9238795325112867385, 1.000000000000000000, 0.9238795325112867385, 1.000000000000000000, 0.9238795325112867385, 1.000000000000000000, 0.9238795325112867385, 1.000000000000000000, 0.9238795325112867385, 1.000000000000000000, 0.9238795325112867385, 1.000000000000000000, 0.9238795325112867385, 1.000000000000000000, 0.9238795325112867385, 1.000000000000000000, 0.9238795325112867385, 1.000000000000000000, 0.9238795325112867385, 1.000000000000000000, 0.9238795325112867385, 1.000000000000000000, 0.9238795325112867385, 1.000000000000000000, 0.9238795325112867385, 1.000000000000000000, 0.9238795325112867385, 1.000000000000000000, 0.9238795325112867385, 1.000000000000000000, 0.9238795325112867385, 1.000000000000000000, 0.9238795325112867385, 1.000000000000000000, 0.9238795325112867385, 1.000000000000000000, 0.9238795325112867385, 1.000000000000000000, 0.9238795325112867385, 1.000000000000000000, 0.9238795325112867385, 1.000000000000000000, 0.9238795325112867385, 1.000000000000000000, 0.9238795325112867385, 1.000000000000000000, 0.9238795325112867385, 1.000000000000000000, 0.9238795325112867385, 1.000000000000000000, 0.9238795325112867385, 1.000000000000000000, 0.9238795325112867385, 1.000000000000000000, 0.9238795325112867385, 1.000000000000000000, 0.9238795325112867385, 1.000000000000000000, 0.9238795325112867385, 1.000000000000000000, 0.9238795325112867385, 1.000000000000000000, 0.9238795325112867385, 1.000000000000000000, 0.9238795325112880708, 0.9999999999999986677 ) ) 
 REPRESENTATION_ITEM ( '' )  );
#20265 = ORIENTED_EDGE ( 'NONE', *, *, #1620, .F. ) ;
#20266 = CARTESIAN_POINT ( 'NONE',  ( -2.775557561562891351E-14, -5.500000000000115463, -161.2500000000000000 ) ) ;
#20267 = CARTESIAN_POINT ( 'NONE',  ( -5.412658773652739619, 3.124999999999975131, -89.31698729810783277 ) ) ;
#20268 = CARTESIAN_POINT ( 'NONE',  ( 20.96132486540536277, 5.551115123125782702E-14, 2.500000000000002220 ) ) ;
#20269 = ORIENTED_EDGE ( 'NONE', *, *, #1937, .T. ) ;
#20270 = CARTESIAN_POINT ( 'NONE',  ( -5.999999999999963585, 1.780251999655701777E-13, -65.91367513459482552 ) ) ;
#20271 = VERTEX_POINT ( 'NONE', #18536 ) ;
#20272 = CARTESIAN_POINT ( 'NONE',  ( 153.9375000000000284, -4.242640687119298093, -4.242640687119298093 ) ) ;
#20273 = CARTESIAN_POINT ( 'NONE',  ( 4.763139720814407951, 2.750000000000002665, -123.2500000000000284 ) ) ;
#20274 = FACE_OUTER_BOUND ( 'NONE', #19151, .T. ) ;
#20275 = CARTESIAN_POINT ( 'NONE',  ( -5.412658773652739619, 3.124999999999975131, -125.3169872981078043 ) ) ;
#20276 = CARTESIAN_POINT ( 'NONE',  ( 5.412658773652739619, 3.124999999999988898, -178.3169872981078470 ) ) ;
#20277 = CARTESIAN_POINT ( 'NONE',  ( -2.775557561562891351E-14, -5.500000000000115463, -174.7500000000000284 ) ) ;
#20278 = CYLINDRICAL_SURFACE ( 'NONE', #28289, 15.00000000000000000 ) ;
#20279 = CARTESIAN_POINT ( 'NONE',  ( -5.999999999999919176, 1.607695154586804565, -47.40331216351300725 ) ) ;
#20280 = ORIENTED_EDGE ( 'NONE', *, *, #4605, .F. ) ;
#20281 = CARTESIAN_POINT ( 'NONE',  ( 13.43750000000012612, -1.999999999999971800, 0.8284271247462354770 ) ) ;
#20282 = DIRECTION ( 'NONE',  ( -7.147005652999508048E-36, 5.642372883946980038E-36, 1.000000000000000000 ) ) ;
#20283 = CARTESIAN_POINT ( 'NONE',  ( 159.3438746676124254, -11.34859173182233860, -3.955658370643484911 ) ) ;
#20284 = CARTESIAN_POINT ( 'NONE',  ( -5.196152422706601826, 2.999999999999975131, -171.0386751345947971 ) ) ;
#20285 = CARTESIAN_POINT ( 'NONE',  ( 0.000000000000000000, -5.999999999999991118, -46.96132486540521711 ) ) ;
#20286 = CARTESIAN_POINT ( 'NONE',  ( 3.608439182435180470, 6.249999999999982236, -71.69198729810781856 ) ) ;
#20287 = CARTESIAN_POINT ( 'NONE',  ( -5.412658773652739619, 3.124999999999975131, -51.81698729810779724 ) ) ;
#20288 = CARTESIAN_POINT ( 'NONE',  ( 4.763139720814407951, -2.749999999999988454, -50.00000000000004263 ) ) ;
#20289 = CARTESIAN_POINT ( 'NONE',  ( 119.9999999999998153, -0.3289648646987480274, -2.003997983315188858 ) ) ;
#20290 = CARTESIAN_POINT ( 'NONE',  ( 24.52451905283846401, 1.480436431285038258E-13, 2.475480947161601275 ) ) ;
#20291 = EDGE_CURVE ( 'NONE', #22378, #25453, #27862, .T. ) ;
#20292 = CARTESIAN_POINT ( 'NONE',  ( -3.175426480542816510, 5.499999999999865885, -131.8750000000000000 ) ) ;
#20293 = CIRCLE ( 'NONE', #13452, 1.000000000000001554 ) ;
#20294 = FACE_OUTER_BOUND ( 'NONE', #28062, .T. ) ;
#20295 = AXIS2_PLACEMENT_3D ( 'NONE', #13220, #29900, #10900 ) ;
#20296 = VERTEX_POINT ( 'NONE', #27702 ) ;
#20297 = CARTESIAN_POINT ( 'NONE',  ( 24.31250000000006395, -1.097466725451379244, -2.649519052838419153 ) ) ;
#20298 = CARTESIAN_POINT ( 'NONE',  ( 160.3988248654052313, 3.889087296526011706, 3.889087296526011706 ) ) ;
#20299 = LINE ( 'NONE', #11250, #12865 ) ;
#20300 = CARTESIAN_POINT ( 'NONE',  ( 142.4211002691896226, -4.999999999999989342, -2.071067811865468400 ) ) ;
#20301 = EDGE_LOOP ( 'NONE', ( #23676, #2835, #20689, #1493 ) ) ;
#20302 = CARTESIAN_POINT ( 'NONE',  ( 115.5622167782373850, 1.849990392679532247, -0.7662911109075883909 ) ) ;
#20303 = CARTESIAN_POINT ( 'NONE',  ( 5.196152422706629359, 3.000000000000002665, -71.96132486540524553 ) ) ;
#20304 = CARTESIAN_POINT ( 'NONE',  ( 9.500000000000008882, -1.999999999999835243, 0.000000000000000000 ) ) ;
#20305 = CARTESIAN_POINT ( 'NONE',  ( -5.412658773652684552, -3.125000000000099920, -116.0669872981078328 ) ) ;
#20306 = CARTESIAN_POINT ( 'NONE',  ( 140.1363996827915059, -11.13639968279144910, -4.472640761300569423 ) ) ;
#20307 = CARTESIAN_POINT ( 'NONE',  ( 104.7401757384974417, 1.839718259470002781, 0.2240791434755549649 ) ) ;
#20308 = EDGE_LOOP ( 'NONE', ( #27599, #29490, #8171, #19215 ) ) ;
#20309 = CARTESIAN_POINT ( 'NONE',  ( 138.0074251345948539, 2.278174593051927044, -5.500000000000096811 ) ) ;
#20310 = CARTESIAN_POINT ( 'NONE',  ( 140.0625000000000284, -4.242640687119298093, 4.242640687119298093 ) ) ;
#20311 = ORIENTED_EDGE ( 'NONE', *, *, #30077, .F. ) ;
#20312 = SURFACE_SIDE_STYLE ('',( #13278 ) ) ;
#20313 = EDGE_CURVE ( 'NONE', #30043, #17687, #20878, .T. ) ;
#20314 = CARTESIAN_POINT ( 'NONE',  ( 4.763139720814407951, 2.750000000000002665, -52.75000000000002132 ) ) ;
#20315 = CARTESIAN_POINT ( 'NONE',  ( 24.06250000000009592, 2.000000000000091926, 0.8284271247461152399 ) ) ;
#20316 = DIRECTION ( 'NONE',  ( 1.000000000000000000, -5.551115123125773458E-17, -1.260129944081490338E-35 ) ) ;
#20317 = CARTESIAN_POINT ( 'NONE',  ( 3.608439182435180470, -6.249999999999997335, -71.55801270189220986 ) ) ;
#20318 = CARTESIAN_POINT ( 'NONE',  ( 134.5000410784369649, -6.964617708402288443, -8.000000000000007105 ) ) ;
#20319 = CARTESIAN_POINT ( 'NONE',  ( 150.3601497308104058, -3.535533905932725318, -3.535533905932725318 ) ) ;
#20320 = CARTESIAN_POINT ( 'NONE',  ( -5.999999999999968026, 1.607695154586720854, -176.9806624327026157 ) ) ;
#20321 = LINE ( 'NONE', #22317, #29961 ) ;
#20322 = DIRECTION ( 'NONE',  ( -1.000000000000000000, 0.000000000000000000, -0.000000000000000000 ) ) ;
#20323 = FACE_OUTER_BOUND ( 'NONE', #19805, .T. ) ;
#20324 = EDGE_CURVE ( 'NONE', #8182, #27945, #14038, .T. ) ;
#20325 = CARTESIAN_POINT ( 'NONE',  ( 6.350852961086080661, -9.614813431917819062E-14, -135.3750000000000284 ) ) ;
#20326 = DIRECTION ( 'NONE',  ( -7.147005652999508048E-36, 5.642372883946980038E-36, 1.000000000000000000 ) ) ;
#20327 = ORIENTED_EDGE ( 'NONE', *, *, #835, .T. ) ;
#20328 = CARTESIAN_POINT ( 'NONE',  ( -4.763139720814407951, -2.750000000000016431, -61.00000000000000000 ) ) ;
#20329 = CYLINDRICAL_SURFACE ( 'NONE', #8610, 6.000000000000000888 ) ;
#20330 = ORIENTED_EDGE ( 'NONE', *, *, #22507, .T. ) ;
#20331 = CARTESIAN_POINT ( 'NONE',  ( 107.4999999999999716, -2.499999999999891198, 3.330669073875469621E-13 ) ) ;
#20332 = CARTESIAN_POINT ( 'NONE',  ( 145.3125000000000284, 4.242640687119298093, -4.242640687119298093 ) ) ;
#20333 = CARTESIAN_POINT ( 'NONE',  ( 142.4136751345948539, 0.000000000000000000, -5.500000000000005329 ) ) ;
#20334 = CARTESIAN_POINT ( 'NONE',  ( 0.000000000000000000, 0.000000000000000000, 0.000000000000000000 ) ) ;
#20335 = ORIENTED_EDGE ( 'NONE', *, *, #24803, .F. ) ;
#20336 = CARTESIAN_POINT ( 'NONE',  ( 21.78867513459492500, -2.499999999999835687, -1.110223024625156540E-13 ) ) ;
#20337 = EDGE_LOOP ( 'NONE', ( #2, #13528, #3647, #21003 ) ) ;
#20338 = CARTESIAN_POINT ( 'NONE',  ( -3.175426480542816510, -5.500000000000057732, -146.3750000000000284 ) ) ;
#20339 =( BOUNDED_CURVE ( )  B_SPLINE_CURVE ( 2, ( #28277, #16664, #26280, #25987, #4932, #14363, #7404, #16812, #26132 ),
 .UNSPECIFIED., .F., .T. ) 
 B_SPLINE_CURVE_WITH_KNOTS ( ( 3, 2, 2, 2, 3 ),
 ( 0.9527777777777778345, 0.9537037037037037202, 0.9555555555555556024, 0.9574074074074073737, 0.9583333333333332593 ),
 .UNSPECIFIED. ) 
 CURVE ( )  GEOMETRIC_REPRESENTATION_ITEM ( )  RATIONAL_B_SPLINE_CURVE ( ( 0.9330127018922194093, 0.9330127018922234061, 1.000000000000000000, 0.8660254037844388186, 1.000000000000000000, 0.8660254037844388186, 1.000000000000000000, 0.9330127018922234061, 0.9330127018922194093 ) ) 
 REPRESENTATION_ITEM ( '' )  );
#20340 = VERTEX_POINT ( 'NONE', #28010 ) ;
#20341 = CARTESIAN_POINT ( 'NONE',  ( 13.56250000000003197, -1.999999999999971800, -0.8284271247462354770 ) ) ;
#20342 = VERTEX_POINT ( 'NONE', #18085 ) ;
#20343 = EDGE_CURVE ( 'NONE', #4636, #27213, #7491, .T. ) ;
#20344 = CARTESIAN_POINT ( 'NONE',  ( 4.763139720814407951, 2.750000000000002665, -75.25000000000004263 ) ) ;
#20345 = CARTESIAN_POINT ( 'NONE',  ( 13.56250000000003375, 1.097466725451679892, 2.649519052838419153 ) ) ;
#20346 = ORIENTED_EDGE ( 'NONE', *, *, #25660, .F. ) ;
#20347 = CARTESIAN_POINT ( 'NONE',  ( 105.1636751345947260, 1.414213562373145550, -1.414213562373034527 ) ) ;
#20348 =( NAMED_UNIT ( * ) SI_UNIT ( $, .STERADIAN. ) SOLID_ANGLE_UNIT ( ) );
#20349 = DIRECTION ( 'NONE',  ( 1.000000000000000000, 0.000000000000000000, 0.000000000000000000 ) ) ;
#20350 = CARTESIAN_POINT ( 'NONE',  ( 0.8631338372297875372, -14.50000000000001243, 7.874007874011823560 ) ) ;
#20351 = CARTESIAN_POINT ( 'NONE',  ( 121.3127832217621034, 1.849990392679682127, -0.7662911109075883909 ) ) ;
#20352 = EDGE_CURVE ( 'NONE', #15916, #10146, #7919, .T. ) ;
#20353 = APPLICATION_PROTOCOL_DEFINITION ( 'draft international standard', 'automotive_design', 1998, #4179 ) ;
#20354 = CARTESIAN_POINT ( 'NONE',  ( 4.763139720814407951, -2.749999999999988454, -155.0000000000000284 ) ) ;
#20355 = CARTESIAN_POINT ( 'NONE',  ( 17.71132486540530238, 2.500000000000057732, -1.665334536937734811E-13 ) ) ;
#20356 = CARTESIAN_POINT ( 'NONE',  ( 19.52382486540523843, 1.035533905932869425, -2.499999999999964473 ) ) ;
#20357 = CARTESIAN_POINT ( 'NONE',  ( 4.763139720814407951, 2.750000000000002665, -87.25000000000005684 ) ) ;
#20358 = CARTESIAN_POINT ( 'NONE',  ( -3.175426480542816510, 5.499999999999865885, -71.87500000000000000 ) ) ;
#20359 = AXIS2_PLACEMENT_3D ( 'NONE', #27697, #20668, #15793 ) ;
#20360 = CARTESIAN_POINT ( 'NONE',  ( -5.999999999999963585, 8.134310703387671600E-14, -141.8363248654052029 ) ) ;
#20361 = LINE ( 'NONE', #9297, #7111 ) ;
#20362 = CARTESIAN_POINT ( 'NONE',  ( 0.000000000000000000, 0.000000000000000000, 0.000000000000000000 ) ) ;
#20363 = CARTESIAN_POINT ( 'NONE',  ( 20.62500000000014211, -1.414213562372979016, -1.414213562373145550 ) ) ;
#20364 = AXIS2_PLACEMENT_3D ( 'NONE', #1307, #13193, #22066 ) ;
#20365 = CARTESIAN_POINT ( 'NONE',  ( 5.196152422706629359, 3.000000000000002665, -119.0386751345948682 ) ) ;
#20366 = CARTESIAN_POINT ( 'NONE',  ( 150.2738248654052597, -3.889087296526011706, 3.889087296526011706 ) ) ;
#20367 = DIRECTION ( 'NONE',  ( -7.147005652999508048E-36, 5.642372883946980038E-36, 1.000000000000000000 ) ) ;
#20368 = ORIENTED_EDGE ( 'NONE', *, *, #20736, .F. ) ;
#20369 = CARTESIAN_POINT ( 'NONE',  ( 158.9062500000000284, 6.000000000000005329, -2.485281374238555774 ) ) ;
#20370 = DIRECTION ( 'NONE',  ( -1.000000000000000000, -1.665334536937736783E-16, -2.220446049250315546E-16 ) ) ;
#20371 = CARTESIAN_POINT ( 'NONE',  ( 117.3127832217621318, 1.849990392679532247, -0.7662911109076485650 ) ) ;
#20372 = ORIENTED_EDGE ( 'NONE', *, *, #1117, .T. ) ;
#20373 = ADVANCED_FACE ( 'NONE', ( #11793 ), #28464, .T. ) ;
#20374 = CARTESIAN_POINT ( 'NONE',  ( 6.350852961086080661, -9.614813431917819062E-14, -99.37499999999998579 ) ) ;
#20375 = CARTESIAN_POINT ( 'NONE',  ( 5.196152422706629359, -2.999999999999988898, -89.28867513459482552 ) ) ;
#20376 = CARTESIAN_POINT ( 'NONE',  ( 5.412658773652739619, 3.124999999999988898, -113.1830127018922383 ) ) ;
#20377 = ORIENTED_EDGE ( 'NONE', *, *, #23713, .F. ) ;
#20378 = PLANE ( 'NONE',  #1472 ) ;
#20379 = CARTESIAN_POINT ( 'NONE',  ( 5.196152422706629359, 3.000000000000002665, -52.46132486540522422 ) ) ;
#20380 = CARTESIAN_POINT ( 'NONE',  ( -7.216878364870328078, 0.000000000000000000, -49.55801270189223828 ) ) ;
#20381 = VERTEX_POINT ( 'NONE', #365 ) ;
#20382 = CARTESIAN_POINT ( 'NONE',  ( 0.000000000000000000, 5.999999999999977796, -160.2113248654052313 ) ) ;
#20383 = EDGE_CURVE ( 'NONE', #13173, #14042, #5678, .T. ) ;
#20384 = CARTESIAN_POINT ( 'NONE',  ( 0.000000000000000000, 0.000000000000000000, 0.000000000000000000 ) ) ;
#20385 = DIRECTION ( 'NONE',  ( 0.000000000000000000, 0.000000000000000000, -1.000000000000000000 ) ) ;
#20386 = CARTESIAN_POINT ( 'NONE',  ( 3.175426480543072749, 5.499999999999865885, -163.6249999999999716 ) ) ;
#20387 = CARTESIAN_POINT ( 'NONE',  ( 116.4999999999999574, -2.499999999999891198, 0.000000000000000000 ) ) ;
#20388 = CARTESIAN_POINT ( 'NONE',  ( -0.07553485551683718213, -14.85597034017936124, 8.150736628208766987 ) ) ;
#20389 = CARTESIAN_POINT ( 'NONE',  ( 0.000000000000000000, 5.499999999999991118, -112.5000000000000426 ) ) ;
#20390 = CARTESIAN_POINT ( 'NONE',  ( 146.1488248654052029, -3.889087296526011706, -3.889087296526011706 ) ) ;
#20391 = CARTESIAN_POINT ( 'NONE',  ( -2.775557561562891351E-14, -5.500000000000115463, -95.25000000000000000 ) ) ;
#20392 = VECTOR ( 'NONE', #20543, 1000.000000000000000 ) ;
#20393 = CARTESIAN_POINT ( 'NONE',  ( -6.000000000000007105, -1.607695154586655129, -112.3466878364870638 ) ) ;
#20394 = CARTESIAN_POINT ( 'NONE',  ( 0.000000000000000000, -5.999999999999991118, -82.03867513459483973 ) ) ;
#20395 = CARTESIAN_POINT ( 'NONE',  ( 13.81249999999996980, 1.097466725451619718, 2.649519052838358757 ) ) ;
#20396 = CARTESIAN_POINT ( 'NONE',  ( 118.8124999999998579, 1.035533905932749299, -2.499999999999784173 ) ) ;
#20397 = B_SPLINE_CURVE_WITH_KNOTS ( 'NONE', 3,
 ( #23602, #4837, #26725, #9614 ),
 .UNSPECIFIED., .F., .F.,
 ( 4, 4 ),
 ( 0.000000000000000000, 0.0004007166227139687315 ),
 .UNSPECIFIED. ) ;
#20398 = CARTESIAN_POINT ( 'NONE',  ( 110.3127832217620323, 1.849990392679501827, -0.7662911109075883909 ) ) ;
#20399 = EDGE_LOOP ( 'NONE', ( #17864, #24367, #17102, #5844 ) ) ;
#20400 = CARTESIAN_POINT ( 'NONE',  ( 3.464101615137852974, 5.999999999999884537, -112.3363248654051887 ) ) ;
#20401 = CARTESIAN_POINT ( 'NONE',  ( 108.6247167782375271, 1.849990392679551343, 0.000000000000000000 ) ) ;
#20402 = CARTESIAN_POINT ( 'NONE',  ( 7.216878364870455975, -6.409875621278545621E-14, -89.94198729810783277 ) ) ;
#20403 = CARTESIAN_POINT ( 'NONE',  ( -5.999999999999963585, -1.487416814333745711E-14, -67.41367513459481131 ) ) ;
#20404 = VERTEX_POINT ( 'NONE', #23588 ) ;
#20405 = CARTESIAN_POINT ( 'NONE',  ( -4.513192036455980549, 10.03241344175770600, -28.95831720094624728 ) ) ;
#20406 = VERTEX_POINT ( 'NONE', #29178 ) ;
#20407 = ORIENTED_EDGE ( 'NONE', *, *, #8586, .T. ) ;
#20408 = CARTESIAN_POINT ( 'NONE',  ( 156.9375000000000284, -4.242640687119298093, -4.242640687119298093 ) ) ;
#20409 = EDGE_CURVE ( 'NONE', #4583, #30412, #8672, .T. ) ;
#20410 = CARTESIAN_POINT ( 'NONE',  ( -3.175426480542816510, 5.499999999999865885, -119.8750000000000284 ) ) ;
#20411 = EDGE_CURVE ( 'NONE', #13602, #15294, #20803, .T. ) ;
#20412 = CARTESIAN_POINT ( 'NONE',  ( 3.608439182435180470, -6.249999999999997335, -140.5580127018922383 ) ) ;
#20413 = ORIENTED_EDGE ( 'NONE', *, *, #19855, .F. ) ;
#20414 = CARTESIAN_POINT ( 'NONE',  ( 161.0000000000000284, 0.000000000000000000, -11.00000000000000355 ) ) ;
#20415 = CARTESIAN_POINT ( 'NONE',  ( 5.412658773652739619, 3.124999999999988898, -119.8169872981078612 ) ) ;
#20416 = CARTESIAN_POINT ( 'NONE',  ( -5.412658773652739619, 3.124999999999975131, -176.3169872981078470 ) ) ;
#20417 = CARTESIAN_POINT ( 'NONE',  ( -6.350852961085760029, -1.281975124255709124E-13, -170.6250000000000284 ) ) ;
#20418 = CYLINDRICAL_SURFACE ( 'NONE', #3771, 5.500000000000000000 ) ;
#20419 = CARTESIAN_POINT ( 'NONE',  ( -6.000000000000000888, 1.067854986875958443E-15, 7.560779664488942560E-35 ) ) ;
#20420 = ORIENTED_EDGE ( 'NONE', *, *, #28192, .F. ) ;
#20421 = CARTESIAN_POINT ( 'NONE',  ( 11.12500000000010658, 1.414213562373201061, 1.414213562373034527 ) ) ;
#20422 = CARTESIAN_POINT ( 'NONE',  ( 124.9999999999999432, -71.00000000000001421, -5.000000000000004441 ) ) ;
#20423 =( BOUNDED_CURVE ( )  B_SPLINE_CURVE ( 2, ( #19278, #26743, #2962 ),
 .UNSPECIFIED., .F., .T. ) 
 B_SPLINE_CURVE_WITH_KNOTS ( ( 3, 3 ),
 ( 0.01315883293251204553, 0.01562500000000000000 ),
 .UNSPECIFIED. ) 
 CURVE ( )  GEOMETRIC_REPRESENTATION_ITEM ( )  RATIONAL_B_SPLINE_CURVE ( ( 0.9671125746057327444, 0.9759710988694461076, 1.000000000000000000 ) ) 
 REPRESENTATION_ITEM ( '' )  );
#20424 = AXIS2_PLACEMENT_3D ( 'NONE', #24638, #6056, #982 ) ;
#20425 = CARTESIAN_POINT ( 'NONE',  ( 159.9008402799206863, -11.15565105496981779, -4.421997596351708637 ) ) ;
#20426 = CARTESIAN_POINT ( 'NONE',  ( -3.464101615137757051, -5.999999999999979572, -55.16367513459481131 ) ) ;
#20427 = CARTESIAN_POINT ( 'NONE',  ( 3.608439182435180470, 6.249999999999982236, -76.19198729810784698 ) ) ;
#20428 = VECTOR ( 'NONE', #21621, 1000.000000000000000 ) ;
#20429 = CARTESIAN_POINT ( 'NONE',  ( 2.775557561562891351E-14, 6.250000000000033751, -61.06698729810783277 ) ) ;
#20430 = CARTESIAN_POINT ( 'NONE',  ( -3.464101615137725076, 5.999999999999979572, -110.5863248654051603 ) ) ;
#20431 = CARTESIAN_POINT ( 'NONE',  ( -4.763139720814407951, 2.749999999999946709, -50.75000000000001421 ) ) ;
#20432 = DIRECTION ( 'NONE',  ( -1.000000000000000000, 0.000000000000000000, 0.000000000000000000 ) ) ;
#20433 = CARTESIAN_POINT ( 'NONE',  ( -6.000000000000007105, -1.607695154586655129, -47.84668783648706381 ) ) ;
#20434 = CARTESIAN_POINT ( 'NONE',  ( 6.350852961086080661, -9.614813431917819062E-14, -121.8750000000000426 ) ) ;
#20435 = DIRECTION ( 'NONE',  ( 1.000000000000000000, -0.000000000000000000, -0.000000000000000000 ) ) ;
#20436 = AXIS2_PLACEMENT_3D ( 'NONE', #28900, #8018, #3246 ) ;
#20437 = VERTEX_POINT ( 'NONE', #2821 ) ;
#20438 = CARTESIAN_POINT ( 'NONE',  ( 143.8199251345948255, -2.278174593052027408, -5.499999999999996447 ) ) ;
#20439 = DIRECTION ( 'NONE',  ( -7.147005652999508048E-36, 5.642372883946980038E-36, 1.000000000000000000 ) ) ;
#20440 = CARTESIAN_POINT ( 'NONE',  ( 141.5773502691896510, 5.000000000000004441, 0.000000000000000000 ) ) ;
#20441 = VERTEX_POINT ( 'NONE', #26872 ) ;
#20442 = VECTOR ( 'NONE', #18248, 1000.000000000000000 ) ;
#20443 = CARTESIAN_POINT ( 'NONE',  ( 110.8747167782375556, 0.000000000000000000, 1.849990392679523588 ) ) ;
#20444 = CARTESIAN_POINT ( 'NONE',  ( 10.53867513459491612, 5.551115123125782702E-14, 2.499999999999724665 ) ) ;
#20445 = DIRECTION ( 'NONE',  ( 1.000000000000000000, -1.387778780781444413E-14, 0.000000000000000000 ) ) ;
#20446 = CARTESIAN_POINT ( 'NONE',  ( 3.608439182435180470, -6.249999999999997335, -114.1919872981078328 ) ) ;
#20447 = CARTESIAN_POINT ( 'NONE',  ( 6.000000000000000888, -1.859271017917181981E-14, -54.08632486540521001 ) ) ;
#20448 = DIRECTION ( 'NONE',  ( -1.000000000000000000, -1.665334536937731113E-16, 1.526556658859586792E-16 ) ) ;
#20449 = EDGE_LOOP ( 'NONE', ( #15601, #8252, #8429, #26103 ) ) ;
#20450 = ORIENTED_EDGE ( 'NONE', *, *, #3456, .F. ) ;
#20451 = CARTESIAN_POINT ( 'NONE',  ( 105.7886751345946550, -1.999999999999946265, 0.000000000000000000 ) ) ;
#20452 = CARTESIAN_POINT ( 'NONE',  ( 140.5312500000000284, -2.485281374238555774, -6.000000000000005329 ) ) ;
#20453 = EDGE_CURVE ( 'NONE', #14299, #1664, #18436, .T. ) ;
#20454 = ORIENTED_EDGE ( 'NONE', *, *, #6391, .T. ) ;
#20455 = AXIS2_PLACEMENT_3D ( 'NONE', #14234, #12365, #17119 ) ;
#20456 = CARTESIAN_POINT ( 'NONE',  ( 3.175426480543072749, 5.499999999999865885, -52.62500000000002842 ) ) ;
#20457 = CARTESIAN_POINT ( 'NONE',  ( 22.56250000000011724, -1.999999999999851674, -0.8284271247462354770 ) ) ;
#20458 = CARTESIAN_POINT ( 'NONE',  ( -0.5000000000000004441, -24.99999999999999289, 8.500000000000007105 ) ) ;
#20459 = VECTOR ( 'NONE', #5043, 1000.000000000000000 ) ;
#20460 = CARTESIAN_POINT ( 'NONE',  ( 130.0000000000000284, -60.00000000000001421, 3.000000000000002665 ) ) ;
#20461 = CARTESIAN_POINT ( 'NONE',  ( -5.412658773652739619, 3.124999999999975131, -66.18301270189225249 ) ) ;
#20462 = CARTESIAN_POINT ( 'NONE',  ( 135.2945438920399681, -8.600858288645461869, -8.000000000000007105 ) ) ;
#20463 = CARTESIAN_POINT ( 'NONE',  ( 151.3913997308104058, -2.071067811865468400, 4.999999999999989342 ) ) ;
#20464 = CARTESIAN_POINT ( 'NONE',  ( -5.999999999999960032, -1.607695154586736397, -178.3466878364870638 ) ) ;
#20465 = DIRECTION ( 'NONE',  ( -8.326672684688675286E-17, -2.081668171172168821E-17, 1.000000000000000000 ) ) ;
#20466 = AXIS2_PLACEMENT_3D ( 'NONE', #1233, #5841, #8144 ) ;
#20467 = DIRECTION ( 'NONE',  ( -1.000000000000000000, -0.000000000000000000, -0.000000000000000000 ) ) ;
#20468 = CARTESIAN_POINT ( 'NONE',  ( 0.000000000000000000, -5.999999999999991118, -67.03867513459482552 ) ) ;
#20469 = CARTESIAN_POINT ( 'NONE',  ( 4.763139720814407951, 2.750000000000002665, -127.7500000000000284 ) ) ;
#20470 = CARTESIAN_POINT ( 'NONE',  ( 137.8199251345948539, -2.278174593052098018, -5.499999999999928058 ) ) ;
#20471 = CARTESIAN_POINT ( 'NONE',  ( 135.0000000000000284, 6.000000000000005329, 0.000000000000000000 ) ) ;
#20472 = ORIENTED_EDGE ( 'NONE', *, *, #3502, .T. ) ;
#20473 = CARTESIAN_POINT ( 'NONE',  ( -2.775557561562891351E-14, -5.500000000000115463, -62.25000000000002842 ) ) ;
#20474 = CARTESIAN_POINT ( 'NONE',  ( -3.464101615137757051, -5.999999999999979572, -154.1636751345947971 ) ) ;
#20475 = CARTESIAN_POINT ( 'NONE',  ( 3.464101615137757051, -5.999999999999979572, -76.83632486540520290 ) ) ;
#20476 = ORIENTED_EDGE ( 'NONE', *, *, #19463, .F. ) ;
#20477 = CARTESIAN_POINT ( 'NONE',  ( 105.8749999999999574, 1.767766952966320915, -1.767766952966320915 ) ) ;
#20478 = CARTESIAN_POINT ( 'NONE',  ( 147.4687500000000853, -2.485281374238585972, 6.000000000000005329 ) ) ;
#20479 = CARTESIAN_POINT ( 'NONE',  ( -5.999999999999963585, 1.780251999655701777E-13, -90.83632486540521711 ) ) ;
#20480 = CARTESIAN_POINT ( 'NONE',  ( 12.81250000000004441, 0.8284271247461753029, -2.000000000000091926 ) ) ;
#20481 = EDGE_CURVE ( 'NONE', #8567, #23700, #25756, .T. ) ;
#20482 = LINE ( 'NONE', #16075, #15080 ) ;
#20483 = STYLED_ITEM ( 'NONE', ( #5650 ), #5179 ) ;
#20484 = CARTESIAN_POINT ( 'NONE',  ( 140.7187500000000284, 2.485281374238555774, -6.000000000000005329 ) ) ;
#20485 = DIRECTION ( 'NONE',  ( -1.000000000000000000, -1.665334536937736783E-16, -2.220446049250315546E-16 ) ) ;
#20486 = ORIENTED_EDGE ( 'NONE', *, *, #20813, .T. ) ;
#20487 = CARTESIAN_POINT ( 'NONE',  ( 6.350852961086080661, -9.614813431917819062E-14, -142.8750000000000568 ) ) ;
#20488 = EDGE_CURVE ( 'NONE', #15144, #9511, #28647, .T. ) ;
#20489 = ORIENTED_EDGE ( 'NONE', *, *, #28029, .F. ) ;
#20490 = CARTESIAN_POINT ( 'NONE',  ( 14.06250000000011546, 2.000000000000151879, 0.8284271247461753029 ) ) ;
#20491 = ORIENTED_EDGE ( 'NONE', *, *, #8586, .F. ) ;
#20492 = CARTESIAN_POINT ( 'NONE',  ( 4.763139720814407951, -2.749999999999988454, -75.50000000000001421 ) ) ;
#20493 = CARTESIAN_POINT ( 'NONE',  ( 10.00000000000012079, -0.6095397824213422133, -2.424553825687569830 ) ) ;
#20494 = CARTESIAN_POINT ( 'NONE',  ( 3.608439182435180470, 6.249999999999982236, -87.55801270189222407 ) ) ;
#20495 = CARTESIAN_POINT ( 'NONE',  ( 10.43750000000004796, -1.999999999999851674, 0.8284271247461753029 ) ) ;
#20496 = CARTESIAN_POINT ( 'NONE',  ( -0.4021627495782659767, -10.99447802115039075, -19.01010557178162941 ) ) ;
#20497 = CARTESIAN_POINT ( 'NONE',  ( -3.464101615137725076, 5.999999999999979572, -150.1636751345947971 ) ) ;
#20498 = DIRECTION ( 'NONE',  ( 0.000000000000000000, 0.000000000000000000, -1.000000000000000000 ) ) ;
#20499 = CYLINDRICAL_SURFACE ( 'NONE', #4455, 6.000000000000000888 ) ;
#20500 = DIRECTION ( 'NONE',  ( -1.000000000000000000, -1.067522139062651904E-16, 0.000000000000000000 ) ) ;
#20501 = STYLED_ITEM ( 'NONE', ( #26451 ), #23889 ) ;
#20502 = VECTOR ( 'NONE', #26994, 1000.000000000000000 ) ;
#20503 = SHAPE_DEFINITION_REPRESENTATION ( #28061, #7189 ) ;
#20504 = CARTESIAN_POINT ( 'NONE',  ( -3.175426480542816066, 5.499999999999865885, -152.8749999999999716 ) ) ;
#20505 = CARTESIAN_POINT ( 'NONE',  ( 139.8316809845309763, -9.383857069608923851, -7.879428590029234236 ) ) ;
#20506 = CARTESIAN_POINT ( 'NONE',  ( -5.630955349224697315, 2.071796769723730058, -179.9999999999999432 ) ) ;
#20507 = CARTESIAN_POINT ( 'NONE',  ( -3.175426480542816066, 5.499999999999865885, -85.37500000000004263 ) ) ;
#20508 = LINE ( 'NONE', #11636, #29170 ) ;
#20509 = CARTESIAN_POINT ( 'NONE',  ( 3.175426480543072749, -5.500000000000105693, -74.12500000000007105 ) ) ;
#20510 = CARTESIAN_POINT ( 'NONE',  ( 150.2961002691897079, 2.071067811865468400, -4.999999999999989342 ) ) ;
#20511 = CARTESIAN_POINT ( 'NONE',  ( 150.1949251345948539, 5.500000000000012434, -2.278174593052012309 ) ) ;
#20512 = CARTESIAN_POINT ( 'NONE',  ( 104.8677751940535785, -1.887434372084343837, -0.4305587433837875788 ) ) ;
#20513 = AXIS2_PLACEMENT_3D ( 'NONE', #30330, #7291, #11788 ) ;
#20514 = CARTESIAN_POINT ( 'NONE',  ( 161.4676415472669930, -3.677632379980754873, -4.807648994257829322 ) ) ;
#20515 = CARTESIAN_POINT ( 'NONE',  ( -5.999999999999919176, 1.607695154586804565, -103.4806624327025872 ) ) ;
#20516 = CARTESIAN_POINT ( 'NONE',  ( 18.68750000000005329, -0.8284271247461753029, -1.999999999999971800 ) ) ;
#20517 = EDGE_CURVE ( 'NONE', #16280, #3063, #11859, .T. ) ;
#20518 = CARTESIAN_POINT ( 'NONE',  ( 139.4136751345948539, 0.000000000000000000, -5.500000000000005329 ) ) ;
#20519 = B_SPLINE_CURVE_WITH_KNOTS ( 'NONE', 2,
 ( #561, #5011, #23635 ),
 .UNSPECIFIED., .F., .F.,
 ( 3, 3 ),
 ( 0.000000000000000000, 1.000000000000000000 ),
 .UNSPECIFIED. ) ;
#20520 = DIRECTION ( 'NONE',  ( 0.000000000000000000, -1.000000000000000000, 0.000000000000000000 ) ) ;
#20521 = CARTESIAN_POINT ( 'NONE',  ( 5.196152422706629359, 3.000000000000002665, -139.4613248654052029 ) ) ;
#20522 =( BOUNDED_CURVE ( )  B_SPLINE_CURVE ( 2, ( #26237, #19644, #14602, #23954, #2892, #3040, #26534, #12312, #28831 ),
 .UNSPECIFIED., .F., .T. ) 
 B_SPLINE_CURVE_WITH_KNOTS ( ( 3, 2, 2, 2, 3 ),
 ( 0.7194444444444444420, 0.7203703703703703276, 0.7222222222222222099, 0.7240740740740740922, 0.7249999999999999778 ),
 .UNSPECIFIED. ) 
 CURVE ( )  GEOMETRIC_REPRESENTATION_ITEM ( )  RATIONAL_B_SPLINE_CURVE ( ( 0.9330127018922194093, 0.9330127018922194093, 1.000000000000000000, 0.8660254037844388186, 1.000000000000000000, 0.8660254037844388186, 1.000000000000000000, 0.9330127018922234061, 0.9330127018922194093 ) ) 
 REPRESENTATION_ITEM ( '' )  );
#20523 = ORIENTED_EDGE ( 'NONE', *, *, #13379, .F. ) ;
#20524 = CARTESIAN_POINT ( 'NONE',  ( 154.5937500000000284, 6.000000000000005329, 2.485281374238585972 ) ) ;
#20525 = CARTESIAN_POINT ( 'NONE',  ( 117.8127832217621744, -1.849990392679501827, 0.7662911109078287542 ) ) ;
#20526 = CARTESIAN_POINT ( 'NONE',  ( 11.71132486540527040, 2.500000000000113243, -5.551115123125782702E-14 ) ) ;
#20527 = ORIENTED_EDGE ( 'NONE', *, *, #3467, .T. ) ;
#20528 = ORIENTED_EDGE ( 'NONE', *, *, #28632, .F. ) ;
#20529 = EDGE_CURVE ( 'NONE', #5997, #23417, #8777, .T. ) ;
#20530 = ADVANCED_FACE ( 'NONE', ( #8297 ), #15415, .T. ) ;
#20531 = ADVANCED_FACE ( 'NONE', ( #14034, #11879 ), #2746, .F. ) ;
#20532 = ORIENTED_EDGE ( 'NONE', *, *, #21919, .T. ) ;
#20533 = CARTESIAN_POINT ( 'NONE',  ( 4.763139720814407951, -2.749999999999988454, -98.00000000000002842 ) ) ;
#20534 = CARTESIAN_POINT ( 'NONE',  ( 3.464101615137852974, 5.999999999999884537, -70.91367513459481131 ) ) ;
#20535 = CARTESIAN_POINT ( 'NONE',  ( -5.412658773652684552, -3.125000000000099920, -107.9330127018922667 ) ) ;
#20536 = EDGE_LOOP ( 'NONE', ( #18957, #25778, #18393, #14162 ) ) ;
#20537 = CARTESIAN_POINT ( 'NONE',  ( 0.4021627495783208772, 10.99447802115039075, -19.01010557178162941 ) ) ;
#20538 = LINE ( 'NONE', #4237, #17002 ) ;
#20539 = CARTESIAN_POINT ( 'NONE',  ( -3.175426480542816510, -5.500000000000057732, -165.8750000000000568 ) ) ;
#20540 = CARTESIAN_POINT ( 'NONE',  ( 6.000000000000000888, 1.743066579297358182E-13, -57.08632486540521001 ) ) ;
#20541 = VERTEX_POINT ( 'NONE', #20104 ) ;
#20542 = DIRECTION ( 'NONE',  ( 1.000000000000000000, -5.551115123125773458E-17, -1.260129944081490338E-35 ) ) ;
#20543 = DIRECTION ( 'NONE',  ( -7.147005652999508048E-36, 5.642372883946980038E-36, 1.000000000000000000 ) ) ;
#20544 = CARTESIAN_POINT ( 'NONE',  ( 3.175426480543072749, 5.499999999999865885, -159.1250000000000000 ) ) ;
#20545 = CARTESIAN_POINT ( 'NONE',  ( 115.3749999999999574, -1.767766952966320915, 1.767766952966431937 ) ) ;
#20546 = CARTESIAN_POINT ( 'NONE',  ( -6.350852961085760029, -1.281975124255709124E-13, -109.1250000000000426 ) ) ;
#20547 = LINE ( 'NONE', #22558, #2164 ) ;
#20548 = CARTESIAN_POINT ( 'NONE',  ( -6.000000000000000888, 1.067854986875958443E-15, 7.560779664488942560E-35 ) ) ;
#20549 = CARTESIAN_POINT ( 'NONE',  ( 3.175426480543072749, 5.499999999999865885, -100.6250000000000000 ) ) ;
#20550 = CARTESIAN_POINT ( 'NONE',  ( 159.3898502691896510, 3.535533905932725318, -3.535533905932725318 ) ) ;
#20551 = PRESENTATION_STYLE_ASSIGNMENT (( #24985 ) ) ;
#20552 = CARTESIAN_POINT ( 'NONE',  ( 0.2148296108471211552, -15.54268077391681047, 8.042193295382688234 ) ) ;
#20553 = EDGE_LOOP ( 'NONE', ( #28651, #6407, #5459, #15371 ) ) ;
#20554 = CARTESIAN_POINT ( 'NONE',  ( 12.87500000000010836, 5.551115123125782702E-14, 2.649519052838333888 ) ) ;
#20555 = CARTESIAN_POINT ( 'NONE',  ( 118.3749999999999147, -1.767766952966293159, 1.767766952966431937 ) ) ;
#20556 = EDGE_CURVE ( 'NONE', #2147, #22177, #19274, .T. ) ;
#20557 = CARTESIAN_POINT ( 'NONE',  ( 110.1252832217622029, -1.665334536937734811E-13, -1.849990392679412565 ) ) ;
#20558 = CYLINDRICAL_SURFACE ( 'NONE', #10569, 6.000000000000000888 ) ;
#20559 = ORIENTED_EDGE ( 'NONE', *, *, #28784, .F. ) ;
#20560 = DIRECTION ( 'NONE',  ( 1.000000000000000000, -0.000000000000000000, -0.000000000000000000 ) ) ;
#20561 = CARTESIAN_POINT ( 'NONE',  ( 108.4372167782374419, 0.7662911109078588412, -1.849990392679231599 ) ) ;
#20562 = CARTESIAN_POINT ( 'NONE',  ( 5.412658773652712085, -3.125000000000086153, -91.56698729810786119 ) ) ;
#20563 = ORIENTED_EDGE ( 'NONE', *, *, #30402, .T. ) ;
#20564 = ADVANCED_FACE ( 'NONE', ( #6114 ), #20558, .T. ) ;
#20565 = CARTESIAN_POINT ( 'NONE',  ( -5.196152422706573404, -3.000000000000002665, -65.78867513459485394 ) ) ;
#20566 = EDGE_CURVE ( 'NONE', #12588, #25384, #25140, .T. ) ;
#20567 = EDGE_LOOP ( 'NONE', ( #24673, #13675, #20162 ) ) ;
#20568 = VERTEX_POINT ( 'NONE', #24697 ) ;
#20569 = CARTESIAN_POINT ( 'NONE',  ( 155.4375000000000284, -4.242640687119298093, -4.242640687119298093 ) ) ;
#20570 = ORIENTED_EDGE ( 'NONE', *, *, #17249, .T. ) ;
#20571 =( BOUNDED_CURVE ( )  B_SPLINE_CURVE ( 2, ( #6384, #23276, #8394, #17801, #22383, #6091, #29590, #16382, #25117 ),
 .UNSPECIFIED., .F., .F. ) 
 B_SPLINE_CURVE_WITH_KNOTS ( ( 3, 2, 2, 2, 3 ),
 ( 0.3527777777777778567, 0.3537037037037037424, 0.3555555555555555136, 0.3574074074074073959, 0.3583333333333332815 ),
 .UNSPECIFIED. ) 
 CURVE ( )  GEOMETRIC_REPRESENTATION_ITEM ( )  RATIONAL_B_SPLINE_CURVE ( ( 0.9330127018922194093, 0.9330127018922234061, 1.000000000000000000, 0.8660254037844388186, 1.000000000000000000, 0.8660254037844388186, 1.000000000000000000, 0.9330127018922234061, 0.9330127018922194093 ) ) 
 REPRESENTATION_ITEM ( '' )  );
#20572 = CARTESIAN_POINT ( 'NONE',  ( 4.763139720814407951, 2.750000000000002665, -120.2500000000000284 ) ) ;
#20573 = CARTESIAN_POINT ( 'NONE',  ( 5.412658773652712085, -3.125000000000086153, -131.4330127018922383 ) ) ;
#20574 = VERTEX_POINT ( 'NONE', #22410 ) ;
#20575 = CARTESIAN_POINT ( 'NONE',  ( -3.464101615137725076, 5.999999999999979572, -160.6636751345948824 ) ) ;
#20576 = CARTESIAN_POINT ( 'NONE',  ( 3.608439182435180470, 6.249999999999982236, -119.6919872981077901 ) ) ;
#20577 = CARTESIAN_POINT ( 'NONE',  ( -7.216878364870328078, 0.000000000000000000, -179.1919872981078754 ) ) ;
#20578 = CARTESIAN_POINT ( 'NONE',  ( 160.6082150250991276, -11.35260501843221448, 3.892452095878841778 ) ) ;
#20579 = PRESENTATION_STYLE_ASSIGNMENT (( #4433 ) ) ;
#20580 = VERTEX_POINT ( 'NONE', #13371 ) ;
#20581 = CARTESIAN_POINT ( 'NONE',  ( 12.87500000000008171, 1.414213562373312083, -1.414213562373034527 ) ) ;
#20582 = CYLINDRICAL_SURFACE ( 'NONE', #489, 5.500000000000000000 ) ;
#20583 = CARTESIAN_POINT ( 'NONE',  ( 159.0000000000000284, -11.33333333333333215, -4.000000000000004441 ) ) ;
#20584 = CARTESIAN_POINT ( 'NONE',  ( 159.0000000000000284, -12.00000000000001066, -5.000000000000004441 ) ) ;
#20585 = DIRECTION ( 'NONE',  ( -0.000000000000000000, -0.000000000000000000, 1.000000000000000000 ) ) ;
#20586 = CARTESIAN_POINT ( 'NONE',  ( 111.5002832217621602, 1.308140751793723799, 1.308140751793640533 ) ) ;
#20587 = CARTESIAN_POINT ( 'NONE',  ( 2.775557561562891351E-14, -6.250000000000061284, -72.31698729810781856 ) ) ;
#20588 = CARTESIAN_POINT ( 'NONE',  ( -5.412658773652739619, 3.124999999999975131, -60.81698729810780435 ) ) ;
#20589 = CARTESIAN_POINT ( 'NONE',  ( 3.175426480543072749, 5.499999999999865885, -46.62500000000006395 ) ) ;
#20590 = CARTESIAN_POINT ( 'NONE',  ( -9.999999999999772626, -90.00000000000001421, 3.000000000000002665 ) ) ;
#20591 = CARTESIAN_POINT ( 'NONE',  ( -5.196152422706573404, -3.000000000000002665, -47.78867513459483973 ) ) ;
#20592 = CARTESIAN_POINT ( 'NONE',  ( 3.175426480543072749, -5.500000000000105693, -123.6250000000000426 ) ) ;
#20593 = CARTESIAN_POINT ( 'NONE',  ( -5.999999999999963585, -1.487416814333745711E-14, -50.33632486540523843 ) ) ;
#20594 = CARTESIAN_POINT ( 'NONE',  ( 114.5386751345947403, -2.775557561562891351E-14, 2.000000000000112799 ) ) ;
#20595 = ORIENTED_EDGE ( 'NONE', *, *, #2118, .F. ) ;
#20596 = CARTESIAN_POINT ( 'NONE',  ( 23.00000000000007461, -1.873492889144789952, 1.873492889144734441 ) ) ;
#20597 = EDGE_CURVE ( 'NONE', #2765, #16117, #25530, .T. ) ;
#20598 = VECTOR ( 'NONE', #25670, 1000.000000000000000 ) ;
#20599 = DIRECTION ( 'NONE',  ( 0.000000000000000000, -1.000000000000000000, 0.000000000000000000 ) ) ;
#20600 = CARTESIAN_POINT ( 'NONE',  ( -0.5000000000000004441, 0.000000000000000000, -8.500000000000007105 ) ) ;
#20601 = CARTESIAN_POINT ( 'NONE',  ( 140.0773502691896510, 5.000000000000004441, 0.000000000000000000 ) ) ;
#20602 = VECTOR ( 'NONE', #23443, 1000.000000000000000 ) ;
#20603 = ORIENTED_EDGE ( 'NONE', *, *, #15927, .F. ) ;
#20604 = CARTESIAN_POINT ( 'NONE',  ( 109.8122167782375840, 0.7662911109078588412, 1.849990392679772278 ) ) ;
#20605 = DIRECTION ( 'NONE',  ( -7.147005652999508048E-36, 5.642372883946980038E-36, 1.000000000000000000 ) ) ;
#20606 = CARTESIAN_POINT ( 'NONE',  ( 111.8747167782376408, 0.000000000000000000, 1.849990392679523588 ) ) ;
#20607 = MECHANICAL_DESIGN_GEOMETRIC_PRESENTATION_REPRESENTATION (  '', ( #18668 ), #28424 ) ;
#20608 = CARTESIAN_POINT ( 'NONE',  ( -7.216878364870328078, 0.000000000000000000, -119.1919872981078470 ) ) ;
#20609 = EDGE_CURVE ( 'NONE', #1806, #7693, #14959, .T. ) ;
#20610 = CARTESIAN_POINT ( 'NONE',  ( 9.999999999999841904, 2.000000000000057288, -4.274358644806852681E-12 ) ) ;
#20611 = VERTEX_POINT ( 'NONE', #28055 ) ;
#20612 = ORIENTED_EDGE ( 'NONE', *, *, #10810, .F. ) ;
#20613 = DIRECTION ( 'NONE',  ( 1.000000000000000000, -5.551115123125773458E-17, -1.260129944081490338E-35 ) ) ;
#20614 = CARTESIAN_POINT ( 'NONE',  ( 141.8437500000000284, -6.000000000000005329, -2.485281374238555774 ) ) ;
#20615 =( BOUNDED_CURVE ( )  B_SPLINE_CURVE ( 2, ( #26926, #17456, #5888, #3584, #10698, #1131, #26770, #19594, #28777 ),
 .UNSPECIFIED., .F., .T. ) 
 B_SPLINE_CURVE_WITH_KNOTS ( ( 3, 2, 2, 2, 3 ),
 ( 0.3694444444444443532, 0.3703703703703703498, 0.3722222222222222321, 0.3740740740740741144, 0.3750000000000000000 ),
 .UNSPECIFIED. ) 
 CURVE ( )  GEOMETRIC_REPRESENTATION_ITEM ( )  RATIONAL_B_SPLINE_CURVE ( ( 0.9330127018922194093, 0.9330127018922154125, 1.000000000000000000, 0.8660254037844388186, 1.000000000000000000, 0.8660254037844388186, 1.000000000000000000, 0.9330127018922194093, 0.9330127018922194093 ) ) 
 REPRESENTATION_ITEM ( '' )  );
#20616 = EDGE_LOOP ( 'NONE', ( #16891, #13770, #132, #1814 ) ) ;
#20617 = CARTESIAN_POINT ( 'NONE',  ( -7.216878364870328078, 0.000000000000000000, -149.1919872981077901 ) ) ;
#20618 = CARTESIAN_POINT ( 'NONE',  ( -0.5000000000000004441, -15.50000000000001421, 0.000000000000000000 ) ) ;
#20619 = LINE ( 'NONE', #18483, #1005 ) ;
#20620 = STYLED_ITEM ( 'NONE', ( #7522 ), #27262 ) ;
#20621 = CARTESIAN_POINT ( 'NONE',  ( 24.68750000000014566, -0.8284271247460552878, -2.000000000000151879 ) ) ;
#20622 = FACE_OUTER_BOUND ( 'NONE', #23829, .T. ) ;
#20623 = CARTESIAN_POINT ( 'NONE',  ( 6.000000000000000888, 7.762456499804235646E-14, -144.0863248654052313 ) ) ;
#20624 = CARTESIAN_POINT ( 'NONE',  ( 5.412658773652712085, -3.125000000000086153, -63.93301270189222407 ) ) ;
#20625 = CARTESIAN_POINT ( 'NONE',  ( 134.5875105163358683, -7.951309655782822006, -8.000000000000007105 ) ) ;
#20626 =( BOUNDED_CURVE ( )  B_SPLINE_CURVE ( 2, ( #1133, #18072, #3743, #29232, #20046, #24939, #26928, #22661, #3586 ),
 .UNSPECIFIED., .F., .T. ) 
 B_SPLINE_CURVE_WITH_KNOTS ( ( 3, 2, 2, 2, 3 ),
 ( 0.3861111111111111827, 0.3870370370370370683, 0.3888888888888888395, 0.3907407407407407218, 0.3916666666666666075 ),
 .UNSPECIFIED. ) 
 CURVE ( )  GEOMETRIC_REPRESENTATION_ITEM ( )  RATIONAL_B_SPLINE_CURVE ( ( 0.9330127018922194093, 0.9330127018922234061, 1.000000000000000000, 0.8660254037844388186, 1.000000000000000000, 0.8660254037844388186, 1.000000000000000000, 0.9330127018922234061, 0.9330127018922194093 ) ) 
 REPRESENTATION_ITEM ( '' )  );
#20627 = CARTESIAN_POINT ( 'NONE',  ( 142.2976497308104058, 0.000000000000000000, 5.000000000000004441 ) ) ;
#20628 = CARTESIAN_POINT ( 'NONE',  ( 112.0386751345946834, 5.551115123125782702E-14, -1.999999999999890754 ) ) ;
#20629 = CARTESIAN_POINT ( 'NONE',  ( 161.0000000000000284, -5.424442335930618420, -0.9085292203135086897 ) ) ;
#20630 = CARTESIAN_POINT ( 'NONE',  ( 6.000000000000014211, -1.607695154586730180, -155.2306624327026441 ) ) ;
#20631 = DIRECTION ( 'NONE',  ( 0.000000000000000000, 0.000000000000000000, -1.000000000000000000 ) ) ;
#20632 = CARTESIAN_POINT ( 'NONE',  ( 2.081668171172167281E-16, 3.582034040661430693E-16, -2.499999999999999112 ) ) ;
#20633 = CARTESIAN_POINT ( 'NONE',  ( 109.9374999999996874, 2.500000000000115019, -1.035533905932448873 ) ) ;
#20634 = DIRECTION ( 'NONE',  ( -0.000000000000000000, -1.000000000000000000, 0.000000000000000000 ) ) ;
#20635 = CARTESIAN_POINT ( 'NONE',  ( 3.175426480543072749, 5.499999999999865885, -124.6250000000000426 ) ) ;
#20636 =( LENGTH_UNIT ( ) NAMED_UNIT ( * ) SI_UNIT ( .MILLI., .METRE. ) );
#20637 = DIRECTION ( 'NONE',  ( -8.326672684688675286E-17, -2.081668171172168821E-17, 1.000000000000000000 ) ) ;
#20638 = ORIENTED_EDGE ( 'NONE', *, *, #1817, .F. ) ;
#20639 = EDGE_CURVE ( 'NONE', #12335, #28056, #4412, .T. ) ;
#20640 = CARTESIAN_POINT ( 'NONE',  ( -3.175426480542816066, 5.499999999999865885, -55.37500000000003553 ) ) ;
#20641 = DIRECTION ( 'NONE',  ( 1.000000000000000000, -5.551115123125773458E-17, -1.260129944081490338E-35 ) ) ;
#20642 = LINE ( 'NONE', #6189, #27228 ) ;
#20643 = ADVANCED_FACE ( 'NONE', ( #6567 ), #16143, .T. ) ;
#20644 = CARTESIAN_POINT ( 'NONE',  ( 13.96132486540527218, 1.110223024625156540E-13, 2.499999999999946709 ) ) ;
#20645 = ORIENTED_EDGE ( 'NONE', *, *, #4170, .F. ) ;
#20646 = CARTESIAN_POINT ( 'NONE',  ( 105.3749999999999005, -1.767766952966320915, 1.767766952966431937 ) ) ;
#20647 = CARTESIAN_POINT ( 'NONE',  ( 139.5000000000000284, 6.000000000000005329, 0.000000000000000000 ) ) ;
#20648 = CYLINDRICAL_SURFACE ( 'NONE', #29763, 5.500000000000000000 ) ;
#20649 = CARTESIAN_POINT ( 'NONE',  ( 136.4062500000000568, 6.000000000000005329, -2.485281374238555774 ) ) ;
#20650 = LINE ( 'NONE', #16374, #7694 ) ;
#20651 = CARTESIAN_POINT ( 'NONE',  ( -3.175426480542816510, 5.499999999999865885, -136.3750000000000568 ) ) ;
#20652 = VERTEX_POINT ( 'NONE', #9036 ) ;
#20653 = CARTESIAN_POINT ( 'NONE',  ( 13.06249999999998046, 2.000000000000151879, 0.8284271247461153509 ) ) ;
#20654 = ORIENTED_EDGE ( 'NONE', *, *, #17345, .F. ) ;
#20655 = CARTESIAN_POINT ( 'NONE',  ( 6.350852961086080661, -9.614813431917819062E-14, -63.37500000000001421 ) ) ;
#20656 = DIRECTION ( 'NONE',  ( -0.000000000000000000, -0.000000000000000000, -1.000000000000000000 ) ) ;
#20657 = CARTESIAN_POINT ( 'NONE',  ( -3.608439182435052128, -6.250000000000110134, -89.80801270189225249 ) ) ;
#20658 = VERTEX_POINT ( 'NONE', #14293 ) ;
#20659 = CARTESIAN_POINT ( 'NONE',  ( -6.000643140593883373, -9.219125907743269011, -25.38858793365676192 ) ) ;
#20660 = FACE_OUTER_BOUND ( 'NONE', #18237, .T. ) ;
#20661 = CARTESIAN_POINT ( 'NONE',  ( 140.1656963055991412, -11.58284815279925262, -4.440052304730661703 ) ) ;
#20662 = CARTESIAN_POINT ( 'NONE',  ( 121.1252832217622597, -5.551115123125782702E-14, -1.849990392679523588 ) ) ;
#20663 = MECHANICAL_DESIGN_GEOMETRIC_PRESENTATION_REPRESENTATION (  '', ( #17238 ), #24563 ) ;
#20664 = CARTESIAN_POINT ( 'NONE',  ( -4.763139720814407951, 2.749999999999946709, -148.2500000000000000 ) ) ;
#20665 = LINE ( 'NONE', #2076, #24124 ) ;
#20666 = CARTESIAN_POINT ( 'NONE',  ( 2.775557561562891351E-14, -6.250000000000061284, -161.6830127018922383 ) ) ;
#20667 = CARTESIAN_POINT ( 'NONE',  ( 156.8363248654052313, 0.000000000000000000, -5.500000000000005329 ) ) ;
#20668 = DIRECTION ( 'NONE',  ( -7.147005652999508048E-36, 5.642372883946980038E-36, 1.000000000000000000 ) ) ;
#20669 = CARTESIAN_POINT ( 'NONE',  ( -4.763139720814407951, -2.750000000000016431, -73.00000000000001421 ) ) ;
#20670 = EDGE_CURVE ( 'NONE', #23700, #28026, #3169, .T. ) ;
#20671 = CARTESIAN_POINT ( 'NONE',  ( -6.000000000000007105, -1.607695154586655129, -74.84668783648703538 ) ) ;
#20672 = CARTESIAN_POINT ( 'NONE',  ( 147.8586002691896510, 2.071067811865468400, 4.999999999999989342 ) ) ;
#20673 = CARTESIAN_POINT ( 'NONE',  ( 0.8631338372297875372, -15.37878787878788067, 8.351220472436777342 ) ) ;
#20674 = CYLINDRICAL_SURFACE ( 'NONE', #15506, 2.000000000000012879 ) ;
#20675 = PRESENTATION_LAYER_ASSIGNMENT (  '', '', ( #15297 ) ) ;
#20676 = CARTESIAN_POINT ( 'NONE',  ( -5.999999999999963585, -1.487416814333745711E-14, -71.91367513459482552 ) ) ;
#20677 = CYLINDRICAL_SURFACE ( 'NONE', #18765, 2.000000000000012879 ) ;
#20678 = LINE ( 'NONE', #23144, #13928 ) ;
#20679 = CARTESIAN_POINT ( 'NONE',  ( 116.2497167782374845, -1.308140751793585022, -1.308140751793640533 ) ) ;
#20680 = LINE ( 'NONE', #9003, #29690 ) ;
#20681 = ORIENTED_EDGE ( 'NONE', *, *, #19965, .T. ) ;
#20682 = CARTESIAN_POINT ( 'NONE',  ( 153.2812500000000568, 2.485281374238585972, 6.000000000000005329 ) ) ;
#20683 = FACE_BOUND ( 'NONE', #21886, .T. ) ;
#20684 = CARTESIAN_POINT ( 'NONE',  ( 117.8752832217622881, -1.849990392679551343, 0.000000000000000000 ) ) ;
#20685 = AXIS2_PLACEMENT_3D ( 'NONE', #28865, #19384, #7978 ) ;
#20686 = CARTESIAN_POINT ( 'NONE',  ( 135.0000000000000284, -8.798545334315205579, -8.160000000000000142 ) ) ;
#20687 = VERTEX_POINT ( 'NONE', #25448 ) ;
#20688 = ORIENTED_EDGE ( 'NONE', *, *, #21805, .T. ) ;
#20689 = ORIENTED_EDGE ( 'NONE', *, *, #20815, .F. ) ;
#20690 = CARTESIAN_POINT ( 'NONE',  ( 0.000000000000000000, 5.499999999999991118, -99.00000000000002842 ) ) ;
#20691 = CARTESIAN_POINT ( 'NONE',  ( -5.412658773652739619, 3.124999999999975131, -103.6830127018922241 ) ) ;
#20692 = ORIENTED_EDGE ( 'NONE', *, *, #20001, .F. ) ;
#20693 = SURFACE_STYLE_USAGE ( .BOTH. , #1783 ) ;
#20694 = CARTESIAN_POINT ( 'NONE',  ( -10.00000000000000178, -19.99999999999998934, 3.000000000000002665 ) ) ;
#20695 = ADVANCED_FACE ( 'NONE', ( #4716 ), #18581, .F. ) ;
#20696 = CARTESIAN_POINT ( 'NONE',  ( 4.763139720814407951, 2.750000000000002665, -163.7500000000000000 ) ) ;
#20697 = CARTESIAN_POINT ( 'NONE',  ( 1.966823652257182253, -10.82907957849942981, -30.68208441639942308 ) ) ;
#20698 = ORIENTED_EDGE ( 'NONE', *, *, #28989, .F. ) ;
#20699 = DIRECTION ( 'NONE',  ( 1.000000000000000000, -5.551115123125773458E-17, -1.260129944081490338E-35 ) ) ;
#20700 = CARTESIAN_POINT ( 'NONE',  ( 0.000000000000000000, 0.000000000000000000, 0.000000000000000000 ) ) ;
#20701 = CARTESIAN_POINT ( 'NONE',  ( -6.350852961085760029, -1.281975124255709124E-13, -170.6249999999999716 ) ) ;
#20702 = CARTESIAN_POINT ( 'NONE',  ( -5.999999999999962697, 3.323446944526963891E-14, -155.9136751345948255 ) ) ;
#20703 = MECHANICAL_DESIGN_GEOMETRIC_PRESENTATION_REPRESENTATION (  '', ( #14358 ), #9916 ) ;
#20704 = CARTESIAN_POINT ( 'NONE',  ( 3.175426480543072749, -5.500000000000105693, -165.6250000000000000 ) ) ;
#20705 = CARTESIAN_POINT ( 'NONE',  ( 114.2499999999999147, -1.110223024625156540E-13, 2.500000000000057732 ) ) ;
#20706 = CARTESIAN_POINT ( 'NONE',  ( -3.175426480542816066, -5.500000000000057732, -111.8750000000000426 ) ) ;
#20707 = CARTESIAN_POINT ( 'NONE',  ( 21.46132486540527751, 5.551115123125782702E-14, -2.500000000000002220 ) ) ;
#20708 = DIRECTION ( 'NONE',  ( 0.000000000000000000, 1.000000000000000000, -0.000000000000000000 ) ) ;
#20709 = CARTESIAN_POINT ( 'NONE',  ( -3.175426480542816510, 5.499999999999865885, -94.37500000000002842 ) ) ;
#20710 =( BOUNDED_CURVE ( )  B_SPLINE_CURVE ( 2, ( #15393, #22121, #21681, #616, #28700, #17082, #5360, #14768, #5808 ),
 .UNSPECIFIED., .F., .T. ) 
 B_SPLINE_CURVE_WITH_KNOTS ( ( 3, 2, 2, 2, 3 ),
 ( 0.3750000000000000000, 0.3759259259259259411, 0.3777777777777777679, 0.3796296296296296502, 0.3805555555555555358 ),
 .UNSPECIFIED. ) 
 CURVE ( )  GEOMETRIC_REPRESENTATION_ITEM ( )  RATIONAL_B_SPLINE_CURVE ( ( 0.9330127018922194093, 0.9330127018922194093, 1.000000000000000000, 0.8660254037844388186, 1.000000000000000000, 0.8660254037844388186, 1.000000000000000000, 0.9330127018922214077, 0.9330127018922194093 ) ) 
 REPRESENTATION_ITEM ( '' )  );
#20711 = EDGE_CURVE ( 'NONE', #4711, #3683, #1394, .T. ) ;
#20712 = FILL_AREA_STYLE_COLOUR ( '', #10077 ) ;
#20713 = CARTESIAN_POINT ( 'NONE',  ( -0.08172161153639843911, -15.06323960844747312, 7.964335018497379792 ) ) ;
#20714 = ORIENTED_EDGE ( 'NONE', *, *, #23713, .T. ) ;
#20715 = CARTESIAN_POINT ( 'NONE',  ( 117.8124999999998579, 1.035533905932869425, -2.499999999999784173 ) ) ;
#20716 = CARTESIAN_POINT ( 'NONE',  ( 10.00000000000014211, 1.983679448820493629, -0.6834733846401986890 ) ) ;
#20717 = FACE_OUTER_BOUND ( 'NONE', #21484, .T. ) ;
#20718 = ORIENTED_EDGE ( 'NONE', *, *, #6195, .T. ) ;
#20719 = CARTESIAN_POINT ( 'NONE',  ( 109.7738248654049471, 2.000000000000031530, 0.8284271247464157772 ) ) ;
#20720 = CARTESIAN_POINT ( 'NONE',  ( 107.8747167782375840, 0.000000000000000000, 1.849990392679523588 ) ) ;
#20721 = VECTOR ( 'NONE', #18449, 1000.000000000000000 ) ;
#20722 = CARTESIAN_POINT ( 'NONE',  ( -5.412658773652684552, -3.125000000000099920, -89.06698729810780435 ) ) ;
#20723 = ORIENTED_EDGE ( 'NONE', *, *, #17249, .F. ) ;
#20724 = CARTESIAN_POINT ( 'NONE',  ( 6.000000000000000888, 1.743066579297358182E-13, -108.6636751345948255 ) ) ;
#20725 = ORIENTED_EDGE ( 'NONE', *, *, #9746, .T. ) ;
#20726 = CARTESIAN_POINT ( 'NONE',  ( 148.5937500000000284, 6.000000000000005329, 2.485281374238585972 ) ) ;
#20727 = CARTESIAN_POINT ( 'NONE',  ( -4.763139720814407951, 2.749999999999946709, -124.2500000000000284 ) ) ;
#20728 = CARTESIAN_POINT ( 'NONE',  ( 22.68750000000008882, -1.097466725451439196, 2.649519052838358757 ) ) ;
#20729 = CARTESIAN_POINT ( 'NONE',  ( -5.412658773652739619, 3.124999999999975131, -127.6830127018922525 ) ) ;
#20730 = ORIENTED_EDGE ( 'NONE', *, *, #20343, .T. ) ;
#20731 = DIRECTION ( 'NONE',  ( -0.000000000000000000, -0.000000000000000000, -1.000000000000000000 ) ) ;
#20732 = CARTESIAN_POINT ( 'NONE',  ( -5.412658773652684552, -3.125000000000099920, -165.5669872981078186 ) ) ;
#20733 = CARTESIAN_POINT ( 'NONE',  ( 2.775557561562891351E-14, 6.250000000000033751, -173.5669872981078186 ) ) ;
#20734 = DIRECTION ( 'NONE',  ( 0.000000000000000000, 0.000000000000000000, -1.000000000000000000 ) ) ;
#20735 = CARTESIAN_POINT ( 'NONE',  ( 24.46132486540536632, 1.665334536937734811E-13, -2.500000000000002220 ) ) ;
#20736 = EDGE_CURVE ( 'NONE', #7007, #6912, #10664, .T. ) ;
#20737 = ORIENTED_EDGE ( 'NONE', *, *, #28582, .T. ) ;
#20738 = CARTESIAN_POINT ( 'NONE',  ( 11.56250000000009059, -1.999999999999851674, -0.8284271247462354770 ) ) ;
#20739 = CARTESIAN_POINT ( 'NONE',  ( 0.2015195925780142172, -15.64213524437055192, -7.848188837846724830 ) ) ;
#20740 = CARTESIAN_POINT ( 'NONE',  ( 0.000000000000000000, 0.000000000000000000, 0.000000000000000000 ) ) ;
#20741 = CARTESIAN_POINT ( 'NONE',  ( 109.4136751345946976, 1.414213562373090038, 1.414213562373034527 ) ) ;
#20742 = FACE_OUTER_BOUND ( 'NONE', #27740, .T. ) ;
#20743 = CARTESIAN_POINT ( 'NONE',  ( 158.0550748654052313, -5.500000000000012434, -2.278174593052012309 ) ) ;
#20744 = CARTESIAN_POINT ( 'NONE',  ( 112.0002832217622739, -1.308140751793557266, -1.308140751793640533 ) ) ;
#20745 = CARTESIAN_POINT ( 'NONE',  ( 3.608439182435180470, 6.249999999999982236, -74.69198729810781856 ) ) ;
#20746 = CARTESIAN_POINT ( 'NONE',  ( 2.775557561562891351E-14, -6.250000000000061284, -63.31698729810780435 ) ) ;
#20747 = CARTESIAN_POINT ( 'NONE',  ( 3.175426480543072749, -5.500000000000105693, -48.62500000000000711 ) ) ;
#20748 = CARTESIAN_POINT ( 'NONE',  ( -0.2114713642193687404, -9.788528635780680887, -4.341247053692759650 ) ) ;
#20749 = CARTESIAN_POINT ( 'NONE',  ( -6.000000000000007105, -1.607695154586655129, -153.7693375672974128 ) ) ;
#20750 = CARTESIAN_POINT ( 'NONE',  ( 5.196152422706629359, 3.000000000000002665, -159.5386751345948539 ) ) ;
#20751 = EDGE_CURVE ( 'NONE', #17680, #2251, #18885, .T. ) ;
#20752 = CARTESIAN_POINT ( 'NONE',  ( 3.175426480543072749, -5.500000000000105693, -119.1250000000000142 ) ) ;
#20753 = ADVANCED_FACE ( 'NONE', ( #20717 ), #21177, .F. ) ;
#20754 = CARTESIAN_POINT ( 'NONE',  ( 4.763139720814407951, 2.750000000000002665, -154.7500000000000568 ) ) ;
#20755 =( NAMED_UNIT ( * ) SI_UNIT ( $, .STERADIAN. ) SOLID_ANGLE_UNIT ( ) );
#20756 = CARTESIAN_POINT ( 'NONE',  ( 154.4925748654052882, 2.278174593051942587, 5.500000000000080824 ) ) ;
#20757 = ORIENTED_EDGE ( 'NONE', *, *, #9438, .F. ) ;
#20758 = CARTESIAN_POINT ( 'NONE',  ( 22.18750000000012434, -2.649519052838178457, -1.097466725451559322 ) ) ;
#20759 = CARTESIAN_POINT ( 'NONE',  ( 6.000000000000000888, 1.743066579297358182E-13, -55.58632486540519579 ) ) ;
#20760 = CARTESIAN_POINT ( 'NONE',  ( 116.2886751345946124, 2.000000000000168310, 3.330669073875469621E-13 ) ) ;
#20761 = AXIS2_PLACEMENT_3D ( 'NONE', #14290, #23631, #11989 ) ;
#20762 = ORIENTED_EDGE ( 'NONE', *, *, #20313, .T. ) ;
#20763 = CARTESIAN_POINT ( 'NONE',  ( 111.4997167782375413, 1.308140751793696044, -1.308140751793640533 ) ) ;
#20764 = CARTESIAN_POINT ( 'NONE',  ( 5.999999999999974243, 1.607695154586759934, -122.0966878364870496 ) ) ;
#20765 = CARTESIAN_POINT ( 'NONE',  ( 113.8747167782375556, 0.000000000000000000, 1.849990392679523588 ) ) ;
#20766 = CARTESIAN_POINT ( 'NONE',  ( 2.775557561562891351E-14, -6.250000000000061284, -111.3169872981077901 ) ) ;
#20767 = CARTESIAN_POINT ( 'NONE',  ( 6.000000000000004441, -1.607695154586747055, -176.2306624327026157 ) ) ;
#20768 = LINE ( 'NONE', #29653, #14775 ) ;
#20769 = VERTEX_POINT ( 'NONE', #25619 ) ;
#20770 = EDGE_LOOP ( 'NONE', ( #1160, #25853, #29589, #19476 ) ) ;
#20771 = CARTESIAN_POINT ( 'NONE',  ( 159.0000000000000284, -12.00000000000001066, 4.000000000000003553 ) ) ;
#20772 = CARTESIAN_POINT ( 'NONE',  ( 136.8750000000000284, 0.000000000000000000, 6.000000000000005329 ) ) ;
#20773 = CARTESIAN_POINT ( 'NONE',  ( 2.775557561562891351E-14, 6.250000000000033751, -50.56698729810782567 ) ) ;
#20774 = CARTESIAN_POINT ( 'NONE',  ( -5.412658773652739619, 3.124999999999975131, -137.3169872981078186 ) ) ;
#20775 = CARTESIAN_POINT ( 'NONE',  ( 18.91367513459496408, -1.767766952966265404, -1.767766952966376426 ) ) ;
#20776 = CARTESIAN_POINT ( 'NONE',  ( 6.000000000000000888, 1.607695154586715303, -151.5193375672974128 ) ) ;
#20777 = EDGE_CURVE ( 'NONE', #25006, #27165, #16420, .T. ) ;
#20778 = CARTESIAN_POINT ( 'NONE',  ( 22.00000000000010303, 2.000000000000168310, 0.000000000000000000 ) ) ;
#20779 = FACE_OUTER_BOUND ( 'NONE', #2638, .T. ) ;
#20780 = CARTESIAN_POINT ( 'NONE',  ( -3.464101615137757051, -5.999999999999979572, -137.6636751345947971 ) ) ;
#20781 = CARTESIAN_POINT ( 'NONE',  ( 5.412658773652712085, -3.125000000000086153, -68.43301270189222407 ) ) ;
#20782 = AXIS2_PLACEMENT_3D ( 'NONE', #3762, #21917, #17626 ) ;
#20783 = CARTESIAN_POINT ( 'NONE',  ( 141.4538997308104058, -2.071067811865468400, -4.999999999999989342 ) ) ;
#20784 = CARTESIAN_POINT ( 'NONE',  ( 0.000000000000000000, 0.000000000000000000, 0.000000000000000000 ) ) ;
#20785 = DIRECTION ( 'NONE',  ( 1.000000000000000000, -0.000000000000000000, -0.000000000000000000 ) ) ;
#20786 = LINE ( 'NONE', #13905, #16377 ) ;
#20787 = CARTESIAN_POINT ( 'NONE',  ( 24.52451905283846401, 1.480436431285038258E-13, 2.475480947161601275 ) ) ;
#20788 = CARTESIAN_POINT ( 'NONE',  ( 108.9999999999998579, 2.500000000000030198, 1.110223024625156540E-13 ) ) ;
#20789 = CARTESIAN_POINT ( 'NONE',  ( 13.46132486540532724, 1.665334536937734811E-13, -2.500000000000057732 ) ) ;
#20790 = EDGE_CURVE ( 'NONE', #22257, #28223, #13828, .T. ) ;
#20791 = CARTESIAN_POINT ( 'NONE',  ( 3.175426480543072749, -5.500000000000105693, -125.1250000000000426 ) ) ;
#20792 = CARTESIAN_POINT ( 'NONE',  ( 137.1636751345948255, 0.000000000000000000, 5.500000000000005329 ) ) ;
#20793 = CARTESIAN_POINT ( 'NONE',  ( -5.412658773652739619, 3.124999999999975131, -142.6830127018922099 ) ) ;
#20794 = CARTESIAN_POINT ( 'NONE',  ( 116.0000000000000142, 0.000000000000000000, 0.000000000000000000 ) ) ;
#20795 = EDGE_LOOP ( 'NONE', ( #15250, #29752, #3368, #23115 ) ) ;
#20796 = CARTESIAN_POINT ( 'NONE',  ( 4.763139720814407951, 2.750000000000002665, -54.25000000000002132 ) ) ;
#20797 = CARTESIAN_POINT ( 'NONE',  ( 5.999999999999949374, -1.607695154586841868, -154.6533121635130215 ) ) ;
#20798 = CARTESIAN_POINT ( 'NONE',  ( 5.196152422706629359, -2.999999999999988898, -76.71132486540521711 ) ) ;
#20799 = CARTESIAN_POINT ( 'NONE',  ( 5.999999999999999112, 2.951592740943527306E-14, -151.5863248654052029 ) ) ;
#20800 = EDGE_LOOP ( 'NONE', ( #16180, #24397, #3198 ) ) ;
#20801 = CARTESIAN_POINT ( 'NONE',  ( 120.4997167782374703, 1.308140751793723799, -1.308140751793640533 ) ) ;
#20802 = CARTESIAN_POINT ( 'NONE',  ( 138.7500000000000284, -6.000000000000005329, 0.000000000000000000 ) ) ;
#20803 = B_SPLINE_CURVE_WITH_KNOTS ( 'NONE', 3,
 ( #23876, #11952, #17554, #7996, #21278, #17401 ),
 .UNSPECIFIED., .F., .F.,
 ( 4, 2, 4 ),
 ( 0.000000000000000000, 0.001072522389057926949, 0.002145044778115853899 ),
 .UNSPECIFIED. ) ;
#20804 = DIRECTION ( 'NONE',  ( -7.147005652999508048E-36, 5.642372883946980038E-36, 1.000000000000000000 ) ) ;
#20805 =( BOUNDED_SURFACE ( )  B_SPLINE_SURFACE ( 1, 2, ( 
 ( #24883, #19981, #13112, #24576, #15244, #20297, #1537, #22292, #1221, #8290, #10632, #25030, #6299, #3835, #20143, #29333, #13262, #17703, #24737, #8609, #22450, #22603, #10945, #29643, #14181, #11715, #20596, #20909, #23218, #18920, #25803, #18767, #23518, #11411, #29945, #30255, #22902, #21058, #16331, #20758, #13563, #4753, #18462, #2459, #4452, #16628, #23370, #2314, #21211, #18613, #25948, #27783, #11875, #30407, #153, #9376, #1846, #6760, #28088, #16181, #9222, #16476, #11248, #2003, #27933, #30105, #8925, #6909, #25327, #7216, #9069, #9532, #7063, #18316, #25650, #28242, #27628, #13721, #23061, #4602, #16029, #6607, #25485, #13877, #14032, #2601, #14895, #887, #14606, #7655, #19648, #21661, #23807, #19072, #26538, #17063, #24236, #23958, #14751, #2741, #12020, #21357, #9828, #12463, #26242, #9982, #28681, #14327, #7797, #17210, #3045, #28987, #24096, #295, #28535, #10137, #7504, #5342, #9683, #28388, #12168, #751, #21514, #16775, #19506, #26098, #14472, #16917, #2896, #20261, #8730, #22407, #17973, #26679, #5788, #15204, #29443, #29136, #15680, #22564, #19789, #1494, #3336, #27286, #24988, #5950, #8418, #22712, #13074, #24537, #17512, #6259, #17823, #3938, #15372, #15524, #3486, #12763, #22105, #1182, #3794, #17661, #1344, #20100, #5642, #29607, #24694, #13368, #29753, #1654, #3637, #24845, #12916, #20395, #22253, #10906, #15045, #10591, #1042, #19942, #29291, #26984, #27143, #27897, #18117, #25444, #15984, #30062, #20554, #15838, #16294, #6871, #27585, #4712, #4256, #25137, #11679, #23332, #20866, #16139, #21022, #13833, #29905, #4102, #4567, #13676, #9032, #8885, #1802, #18728, #25614, #13524, #4408, #23178, #23484, #30370, #9338, #28051, #25283, #22864, #2122, #27435, #13993, #30217, #23017, #6563, #7023, #1963, #16441, #11525, #21172, #25766, #14145, #2422, #9181, #114, #18577, #11836, #24057, #12423, #5003, #7758, #3146, #17169, #3002, #26060, #19320, #9496, #16883 ),
 ( #28796, #4860, #710, #21317, #9790, #23769, #11987, #19169, #7469, #19467, #2857, #26202, #18879, #5448, #9642, #23916, #26492, #28352, #2563, #5153, #21622, #28201, #28642, #14568, #554, #9944, #260, #14857, #24201, #7613, #17023, #7176, #19035, #26351, #7327, #5301, #14714, #5906, #28947, #20226, #13191, #10719, #5750, #15486, #24953, #17325, #5601, #15005, #24345, #24811, #10398, #3761, #19751, #8211, #8056, #12876, #17471, #26786, #24496, #29249, #22983, #4674, #28014, #8999, #18233, #22674, #25410, #1617, #13638, #23143, #20363, #18539, #6686, #4532, #27865, #30337, #9147, #13798, #1767, #4062, #6986, #2242, #13957, #23298, #16406, #1924, #18691, #13486, #16107, #11330, #6527, #20989, #25576, #27402, #30029, #27551, #20833, #11644, #6367, #15949, #11169, #20516, #29869, #27704, #8850, #18388, #25248, #4221, #23446, #4971, #14539, #21136, #28608, #28467, #14679, #7578, #21736, #16991, #23879, #23591, #16556, #19437, #2968, #675, #10061, #28762, #23740, #7730, #4828, #16845, #9757, #26023, #9458, #18842, #2528, #11955, #9606, #21282, #220, #29212, #10362, #22494, #22333, #7879, #10513, #1267, #22179, #10678, #27070, #8336, #24615, #19867, #12691, #10216, #3260, #22024, #20025, #24459, #1113, #29372, #12838, #17746, #13155, #29541, #15290, #1427, #17904, #10836, #5419, #20188, #29066, #6035, #8031, #17437, #26750, #15128, #3412, #17591, #15453, #24174, #3117, #12539, #15611, #13449, #11294, #6799, #22797, #13302, #18203, #6656, #24924, #25377, #4190, #11132, #8819, #20480, #27521, #16223, #13605, #22950, #2057, #7548, #9573, #18967, #2641, #12060, #2787, #641, #9876, #482, #12215, #21555, #19251, #5235, #14647, #4643, #14076, #28135, #5682, #17711, #3379, #6000, #12805, #10024, #10327, #5534, #26876, #14940, #24278, #19692, #3225, #29035, #22146, #1089, #10484, #5838, #15253, #25037, #13413, #8465, #9503, #2430, #3992, #22760, #11842, #21179, #18024, #29649, #20304 ) ),
 .UNSPECIFIED., .F., .F., .T. ) 
 B_SPLINE_SURFACE_WITH_KNOTS ( ( 2, 2 ),
 ( 3, 2, 2, 2, 2, 2, 2, 2, 2, 2, 2, 2, 2, 2, 2, 2, 2, 2, 2, 2, 2, 2, 2, 2, 2, 2, 2, 2, 2, 2, 2, 2, 2, 2, 2, 2, 2, 2, 2, 2, 2, 2, 2, 2, 2, 2, 2, 2, 2, 2, 2, 2, 2, 2, 2, 2, 2, 2, 2, 2, 2, 2, 2, 2, 2, 2, 2, 2, 2, 2, 2, 2, 2, 2, 2, 2, 2, 2, 2, 2, 2, 2, 2, 2, 2, 2, 2, 2, 2, 2, 2, 2, 2, 2, 2, 2, 2, 2, 2, 2, 2, 2, 2, 2, 2, 2, 2, 2, 2, 2, 2, 2, 2, 2, 2, 2, 2, 2, 2, 2, 2, 2, 2, 2, 3 ),
 ( 0.000000000000000000, 1.000000000000000000 ),
 ( 0.000000000000000000, 0.007812500000000000000, 0.01562500000000000000, 0.02343750000000000000, 0.03125000000000000000, 0.03906250000000000000, 0.04687500000000000000, 0.05468750000000000000, 0.06250000000000000000, 0.07031250000000000000, 0.07812500000000000000, 0.08593750000000000000, 0.09375000000000000000, 0.1015625000000000000, 0.1093750000000000000, 0.1171875000000000000, 0.1250000000000000000, 0.1328125000000000000, 0.1406250000000000000, 0.1484375000000000000, 0.1562500000000000000, 0.1640625000000000000, 0.1718750000000000000, 0.1796875000000000000, 0.1875000000000000000, 0.1953125000000000000, 0.2031250000000000000, 0.2109375000000000000, 0.2187500000000000000, 0.2265625000000000000, 0.2343750000000000000, 0.2421875000000000000, 0.2500000000000000000, 0.2578125000000000000, 0.2656250000000000000, 0.2734375000000000000, 0.2812500000000000000, 0.2890625000000000000, 0.2968750000000000000, 0.3046875000000000000, 0.3125000000000000000, 0.3203125000000000000, 0.3281250000000000000, 0.3359375000000000000, 0.3437500000000000000, 0.3515625000000000000, 0.3593750000000000000, 0.3671875000000000000, 0.3750000000000000000, 0.3828125000000000000, 0.3906250000000000000, 0.3984375000000000000, 0.4062500000000000000, 0.4140625000000000000, 0.4218750000000000000, 0.4296875000000000000, 0.4375000000000000000, 0.4453125000000000000, 0.4531250000000000000, 0.4609375000000000000, 0.4687500000000000000, 0.4765625000000000000, 0.4843750000000000000, 0.4921875000000000000, 0.5000000000000000000, 0.5078125000000000000, 0.5156250000000000000, 0.5234375000000000000, 0.5312500000000000000, 0.5390625000000000000, 0.5468750000000000000, 0.5546875000000000000, 0.5625000000000000000, 0.5703125000000000000, 0.5781250000000000000, 0.5859375000000000000, 0.5937500000000000000, 0.6015625000000000000, 0.6093750000000000000, 0.6171875000000000000, 0.6250000000000000000, 0.6328125000000000000, 0.6406250000000000000, 0.6484375000000000000, 0.6562500000000000000, 0.6640625000000000000, 0.6718750000000000000, 0.6796875000000000000, 0.6875000000000000000, 0.6953125000000000000, 0.7031250000000000000, 0.7109375000000000000, 0.7187500000000000000, 0.7265625000000000000, 0.7343750000000000000, 0.7421875000000000000, 0.7500000000000000000, 0.7578125000000000000, 0.7656250000000000000, 0.7734375000000000000, 0.7812500000000000000, 0.7890625000000000000, 0.7968750000000000000, 0.8046875000000000000, 0.8125000000000000000, 0.8203125000000000000, 0.8281250000000000000, 0.8359375000000000000, 0.8437500000000000000, 0.8515625000000000000, 0.8593750000000000000, 0.8671875000000000000, 0.8750000000000000000, 0.8828125000000000000, 0.8906250000000000000, 0.8984375000000000000, 0.9062500000000000000, 0.9140625000000000000, 0.9218750000000000000, 0.9296875000000000000, 0.9375000000000000000, 0.9453125000000000000, 0.9531250000000000000, 0.9609375000000000000, 0.9687500000000000000 ),
 .UNSPECIFIED. ) 
 GEOMETRIC_REPRESENTATION_ITEM ( )  RATIONAL_B_SPLINE_SURFACE ( (
 ( 1.000000000000000000, 0.9238795325112867385, 1.000000000000000000, 0.9238795325112867385, 1.000000000000000000, 0.9238795325112867385, 1.000000000000000000, 0.9238795325112867385, 1.000000000000000000, 0.9238795325112867385, 1.000000000000000000, 0.9238795325112867385, 1.000000000000000000, 0.9238795325112867385, 1.000000000000000000, 0.9238795325112867385, 1.000000000000000000, 0.9238795325112867385, 1.000000000000000000, 0.9238795325112867385, 1.000000000000000000, 0.9238795325112867385, 1.000000000000000000, 0.9238795325112867385, 1.000000000000000000, 0.9238795325112867385, 1.000000000000000000, 0.9238795325112867385, 1.000000000000000000, 0.9238795325112867385, 1.000000000000000000, 0.9238795325112867385, 1.000000000000000000, 0.9238795325112867385, 1.000000000000000000, 0.9238795325112867385, 1.000000000000000000, 0.9238795325112867385, 1.000000000000000000, 0.9238795325112867385, 1.000000000000000000, 0.9238795325112867385, 1.000000000000000000, 0.9238795325112867385, 1.000000000000000000, 0.9238795325112867385, 1.000000000000000000, 0.9238795325112867385, 1.000000000000000000, 0.9238795325112867385, 1.000000000000000000, 0.9238795325112867385, 1.000000000000000000, 0.9238795325112867385, 1.000000000000000000, 0.9238795325112867385, 1.000000000000000000, 0.9238795325112867385, 1.000000000000000000, 0.9238795325112867385, 1.000000000000000000, 0.9238795325112867385, 1.000000000000000000, 0.9238795325112867385, 1.000000000000000000, 0.9238795325112867385, 1.000000000000000000, 0.9238795325112867385, 1.000000000000000000, 0.9238795325112867385, 1.000000000000000000, 0.9238795325112867385, 1.000000000000000000, 0.9238795325112867385, 1.000000000000000000, 0.9238795325112867385, 1.000000000000000000, 0.9238795325112867385, 1.000000000000000000, 0.9238795325112867385, 1.000000000000000000, 0.9238795325112867385, 1.000000000000000000, 0.9238795325112867385, 1.000000000000000000, 0.9238795325112867385, 1.000000000000000000, 0.9238795325112867385, 1.000000000000000000, 0.9238795325112867385, 1.000000000000000000, 0.9238795325112867385, 1.000000000000000000, 0.9238795325112867385, 1.000000000000000000, 0.9238795325112867385, 1.000000000000000000, 0.9238795325112867385, 1.000000000000000000, 0.9238795325112867385, 1.000000000000000000, 0.9238795325112867385, 1.000000000000000000, 0.9238795325112867385, 1.000000000000000000, 0.9238795325112867385, 1.000000000000000000, 0.9238795325112867385, 1.000000000000000000, 0.9238795325112867385, 1.000000000000000000, 0.9238795325112867385, 1.000000000000000000, 0.9238795325112867385, 1.000000000000000000, 0.9238795325112867385, 1.000000000000000000, 0.9238795325112867385, 1.000000000000000000, 0.9238795325112867385, 1.000000000000000000, 0.9238795325112867385, 1.000000000000000000, 0.9238795325112867385, 1.000000000000000000, 0.9238795325112867385, 1.000000000000000000, 0.9238795325112867385, 1.000000000000000000, 0.9238795325112867385, 1.000000000000000000, 0.9238795325112867385, 1.000000000000000000, 0.9238795325112867385, 1.000000000000000000, 0.9238795325112867385, 1.000000000000000000, 0.9238795325112867385, 1.000000000000000000, 0.9238795325112867385, 1.000000000000000000, 0.9238795325112867385, 1.000000000000000000, 0.9238795325112867385, 1.000000000000000000, 0.9238795325112867385, 1.000000000000000000, 0.9238795325112867385, 1.000000000000000000, 0.9238795325112867385, 1.000000000000000000, 0.9238795325112867385, 1.000000000000000000, 0.9238795325112867385, 1.000000000000000000, 0.9238795325112867385, 1.000000000000000000, 0.9238795325112867385, 1.000000000000000000, 0.9238795325112867385, 1.000000000000000000, 0.9238795325112867385, 1.000000000000000000, 0.9238795325112867385, 1.000000000000000000, 0.9238795325112867385, 1.000000000000000000, 0.9238795325112867385, 1.000000000000000000, 0.9238795325112867385, 1.000000000000000000, 0.9238795325112867385, 1.000000000000000000, 0.9238795325112867385, 1.000000000000000000, 0.9238795325112867385, 1.000000000000000000, 0.9238795325112867385, 1.000000000000000000, 0.9238795325112867385, 1.000000000000000000, 0.9238795325112867385, 1.000000000000000000, 0.9238795325112867385, 1.000000000000000000, 0.9238795325112867385, 1.000000000000000000, 0.9238795325112867385, 1.000000000000000000, 0.9238795325112867385, 1.000000000000000000, 0.9238795325112867385, 1.000000000000000000, 0.9238795325112867385, 1.000000000000000000, 0.9238795325112867385, 1.000000000000000000, 0.9238795325112867385, 1.000000000000000000, 0.9238795325112867385, 1.000000000000000000, 0.9238795325112867385, 1.000000000000000000, 0.9238795325112867385, 1.000000000000000000, 0.9238795325112867385, 1.000000000000000000, 0.9238795325112867385, 1.000000000000000000, 0.9238795325112867385, 1.000000000000000000, 0.9238795325112867385, 1.000000000000000000, 0.9238795325112867385, 1.000000000000000000, 0.9238795325112867385, 1.000000000000000000, 0.9238795325112867385, 1.000000000000000000, 0.9238795325112867385, 1.000000000000000000, 0.9238795325112867385, 1.000000000000000000, 0.9238795325112867385, 1.000000000000000000, 0.9238795325112867385, 1.000000000000000000, 0.9238795325112867385, 1.000000000000000000, 0.9238795325112867385, 1.000000000000000000, 0.9238795325112867385, 1.000000000000000000, 0.9238795325112867385, 1.000000000000000000, 0.9238795325112867385, 1.000000000000000000, 0.9238795325112867385, 1.000000000000000000, 0.9238795325112867385, 1.000000000000000000, 0.9238795325112867385, 1.000000000000000000, 0.9238795325112867385, 1.000000000000000000, 0.9238795325112867385, 1.000000000000000000, 0.9238795325112867385, 1.000000000000000000),
 ( 1.000000000000000000, 0.9238795325112867385, 1.000000000000000000, 0.9238795325112867385, 1.000000000000000000, 0.9238795325112867385, 1.000000000000000000, 0.9238795325112867385, 1.000000000000000000, 0.9238795325112867385, 1.000000000000000000, 0.9238795325112867385, 1.000000000000000000, 0.9238795325112867385, 1.000000000000000000, 0.9238795325112867385, 1.000000000000000000, 0.9238795325112867385, 1.000000000000000000, 0.9238795325112867385, 1.000000000000000000, 0.9238795325112867385, 1.000000000000000000, 0.9238795325112867385, 1.000000000000000000, 0.9238795325112867385, 1.000000000000000000, 0.9238795325112867385, 1.000000000000000000, 0.9238795325112867385, 1.000000000000000000, 0.9238795325112867385, 1.000000000000000000, 0.9238795325112867385, 1.000000000000000000, 0.9238795325112867385, 1.000000000000000000, 0.9238795325112867385, 1.000000000000000000, 0.9238795325112867385, 1.000000000000000000, 0.9238795325112867385, 1.000000000000000000, 0.9238795325112867385, 1.000000000000000000, 0.9238795325112867385, 1.000000000000000000, 0.9238795325112867385, 1.000000000000000000, 0.9238795325112867385, 1.000000000000000000, 0.9238795325112867385, 1.000000000000000000, 0.9238795325112867385, 1.000000000000000000, 0.9238795325112867385, 1.000000000000000000, 0.9238795325112867385, 1.000000000000000000, 0.9238795325112867385, 1.000000000000000000, 0.9238795325112867385, 1.000000000000000000, 0.9238795325112867385, 1.000000000000000000, 0.9238795325112867385, 1.000000000000000000, 0.9238795325112867385, 1.000000000000000000, 0.9238795325112867385, 1.000000000000000000, 0.9238795325112867385, 1.000000000000000000, 0.9238795325112867385, 1.000000000000000000, 0.9238795325112867385, 1.000000000000000000, 0.9238795325112867385, 1.000000000000000000, 0.9238795325112867385, 1.000000000000000000, 0.9238795325112867385, 1.000000000000000000, 0.9238795325112867385, 1.000000000000000000, 0.9238795325112867385, 1.000000000000000000, 0.9238795325112867385, 1.000000000000000000, 0.9238795325112867385, 1.000000000000000000, 0.9238795325112867385, 1.000000000000000000, 0.9238795325112867385, 1.000000000000000000, 0.9238795325112867385, 1.000000000000000000, 0.9238795325112867385, 1.000000000000000000, 0.9238795325112867385, 1.000000000000000000, 0.9238795325112867385, 1.000000000000000000, 0.9238795325112867385, 1.000000000000000000, 0.9238795325112867385, 1.000000000000000000, 0.9238795325112867385, 1.000000000000000000, 0.9238795325112867385, 1.000000000000000000, 0.9238795325112867385, 1.000000000000000000, 0.9238795325112867385, 1.000000000000000000, 0.9238795325112867385, 1.000000000000000000, 0.9238795325112867385, 1.000000000000000000, 0.9238795325112867385, 1.000000000000000000, 0.9238795325112867385, 1.000000000000000000, 0.9238795325112867385, 1.000000000000000000, 0.9238795325112867385, 1.000000000000000000, 0.9238795325112867385, 1.000000000000000000, 0.9238795325112867385, 1.000000000000000000, 0.9238795325112867385, 1.000000000000000000, 0.9238795325112867385, 1.000000000000000000, 0.9238795325112867385, 1.000000000000000000, 0.9238795325112867385, 1.000000000000000000, 0.9238795325112867385, 1.000000000000000000, 0.9238795325112867385, 1.000000000000000000, 0.9238795325112867385, 1.000000000000000000, 0.9238795325112867385, 1.000000000000000000, 0.9238795325112867385, 1.000000000000000000, 0.9238795325112867385, 1.000000000000000000, 0.9238795325112867385, 1.000000000000000000, 0.9238795325112867385, 1.000000000000000000, 0.9238795325112867385, 1.000000000000000000, 0.9238795325112867385, 1.000000000000000000, 0.9238795325112867385, 1.000000000000000000, 0.9238795325112867385, 1.000000000000000000, 0.9238795325112867385, 1.000000000000000000, 0.9238795325112867385, 1.000000000000000000, 0.9238795325112867385, 1.000000000000000000, 0.9238795325112867385, 1.000000000000000000, 0.9238795325112867385, 1.000000000000000000, 0.9238795325112867385, 1.000000000000000000, 0.9238795325112867385, 1.000000000000000000, 0.9238795325112867385, 1.000000000000000000, 0.9238795325112867385, 1.000000000000000000, 0.9238795325112867385, 1.000000000000000000, 0.9238795325112867385, 1.000000000000000000, 0.9238795325112867385, 1.000000000000000000, 0.9238795325112867385, 1.000000000000000000, 0.9238795325112867385, 1.000000000000000000, 0.9238795325112867385, 1.000000000000000000, 0.9238795325112867385, 1.000000000000000000, 0.9238795325112867385, 1.000000000000000000, 0.9238795325112867385, 1.000000000000000000, 0.9238795325112867385, 1.000000000000000000, 0.9238795325112867385, 1.000000000000000000, 0.9238795325112867385, 1.000000000000000000, 0.9238795325112867385, 1.000000000000000000, 0.9238795325112867385, 1.000000000000000000, 0.9238795325112867385, 1.000000000000000000, 0.9238795325112867385, 1.000000000000000000, 0.9238795325112867385, 1.000000000000000000, 0.9238795325112867385, 1.000000000000000000, 0.9238795325112867385, 1.000000000000000000, 0.9238795325112867385, 1.000000000000000000, 0.9238795325112867385, 1.000000000000000000, 0.9238795325112867385, 1.000000000000000000, 0.9238795325112867385, 1.000000000000000000, 0.9238795325112867385, 1.000000000000000000, 0.9238795325112867385, 1.000000000000000000, 0.9238795325112867385, 1.000000000000000000, 0.9238795325112867385, 1.000000000000000000, 0.9238795325112867385, 1.000000000000000000, 0.9238795325112867385, 1.000000000000000000, 0.9238795325112867385, 1.000000000000000000, 0.9238795325112867385, 1.000000000000000000, 0.9238795325112867385, 1.000000000000000000, 0.9238795325112867385, 1.000000000000000000, 0.9238795325112867385, 1.000000000000000000) ) ) 
 REPRESENTATION_ITEM ( '' )  SURFACE ( )  );
#20806 = CARTESIAN_POINT ( 'NONE',  ( 138.7500000000000284, -6.000000000000005329, 0.000000000000000000 ) ) ;
#20807 = VERTEX_POINT ( 'NONE', #16740 ) ;
#20808 = CARTESIAN_POINT ( 'NONE',  ( 3.175426480543072749, -5.500000000000105693, -135.6250000000000000 ) ) ;
#20809 = VERTEX_POINT ( 'NONE', #15009 ) ;
#20810 = CARTESIAN_POINT ( 'NONE',  ( 13.31250000000012612, -0.8284271247460553989, 1.999999999999911626 ) ) ;
#20811 = VERTEX_POINT ( 'NONE', #19324 ) ;
#20812 = CARTESIAN_POINT ( 'NONE',  ( 6.350852961086080661, -9.614813431917819062E-14, -69.37500000000004263 ) ) ;
#20813 = EDGE_CURVE ( 'NONE', #25966, #25175, #27207, .T. ) ;
#20814 = CARTESIAN_POINT ( 'NONE',  ( -6.000000000000000888, 1.067854986875958443E-15, 7.560779664488942560E-35 ) ) ;
#20815 = EDGE_CURVE ( 'NONE', #12881, #5798, #29671, .T. ) ;
#20816 = PRODUCT_DEFINITION ( 'UNKNOWN', '', #6531, #25523 ) ;
#20817 = CARTESIAN_POINT ( 'NONE',  ( -4.999999999999990230, -24.99999999999999289, -7.500000000000007105 ) ) ;
#20818 = DIRECTION ( 'NONE',  ( 1.000000000000000000, -5.551115123125773458E-17, -1.260129944081490338E-35 ) ) ;
#20819 = CARTESIAN_POINT ( 'NONE',  ( 120.3127832217622171, 1.849990392679591977, -0.7662911109075883909 ) ) ;
#20820 = CARTESIAN_POINT ( 'NONE',  ( 4.763139720814407951, -2.749999999999988454, -144.5000000000000284 ) ) ;
#20821 = CARTESIAN_POINT ( 'NONE',  ( 140.4999999682997895, -9.426604554197883346, -7.431193927736174487 ) ) ;
#20822 = CARTESIAN_POINT ( 'NONE',  ( 4.763139720814407951, 2.750000000000002665, -142.7500000000000568 ) ) ;
#20823 = CARTESIAN_POINT ( 'NONE',  ( 3.608439182435180470, -6.249999999999997335, -163.0580127018922099 ) ) ;
#20824 = CARTESIAN_POINT ( 'NONE',  ( 3.044979857375308677E-14, 10.99999999999998224, -14.99152654425661702 ) ) ;
#20825 = CARTESIAN_POINT ( 'NONE',  ( 3.175426480543072749, -5.500000000000105693, -81.62500000000002842 ) ) ;
#20826 = DIRECTION ( 'NONE',  ( 1.000000000000000000, -5.551115123125773458E-17, -1.260129944081490338E-35 ) ) ;
#20827 = CARTESIAN_POINT ( 'NONE',  ( -4.763139720814407951, -2.750000000000016431, -76.00000000000001421 ) ) ;
#20828 = CARTESIAN_POINT ( 'NONE',  ( 6.000000000000052403, -1.607695154586662678, -156.1533121635129930 ) ) ;
#20829 = CARTESIAN_POINT ( 'NONE',  ( -5.999999999999963585, -1.487416814333745711E-14, -88.41367513459482552 ) ) ;
#20830 = DIRECTION ( 'NONE',  ( 1.000000000000000000, -5.551115123125773458E-17, -1.260129944081490338E-35 ) ) ;
#20831 = CARTESIAN_POINT ( 'NONE',  ( 156.8437500000000284, -6.000000000000005329, -2.485281374238556218 ) ) ;
#20832 = DIRECTION ( 'NONE',  ( 1.000000000000000000, 0.000000000000000000, 0.000000000000000000 ) ) ;
#20833 = CARTESIAN_POINT ( 'NONE',  ( 19.00000000000020961, 2.000000000000223821, -5.551115123125782702E-14 ) ) ;
#20834 = CARTESIAN_POINT ( 'NONE',  ( -3.464101615137725076, 5.999999999999979572, -118.6636751345947829 ) ) ;
#20835 = CARTESIAN_POINT ( 'NONE',  ( 119.1872167782375271, -1.849990392679562001, -0.7662911109077087390 ) ) ;
#20836 = CARTESIAN_POINT ( 'NONE',  ( 0.000000000000000000, 0.000000000000000000, 0.000000000000000000 ) ) ;
#20837 = ORIENTED_EDGE ( 'NONE', *, *, #28246, .F. ) ;
#20838 = CARTESIAN_POINT ( 'NONE',  ( 156.3750000000000284, 0.000000000000000000, 6.000000000000005329 ) ) ;
#20839 =( LENGTH_UNIT ( ) NAMED_UNIT ( * ) SI_UNIT ( .MILLI., .METRE. ) );
#20840 = CARTESIAN_POINT ( 'NONE',  ( 113.8127832217621034, -1.849990392679441875, 0.7662911109079489913 ) ) ;
#20841 = DIRECTION ( 'NONE',  ( -7.147005652999508048E-36, 5.642372883946980038E-36, 1.000000000000000000 ) ) ;
#20842 = ORIENTED_EDGE ( 'NONE', *, *, #27637, .F. ) ;
#20843 = EDGE_LOOP ( 'NONE', ( #18116, #23711, #30038, #14361 ) ) ;
#20844 = EDGE_LOOP ( 'NONE', ( #6575, #9314, #6532 ) ) ;
#20845 = CARTESIAN_POINT ( 'NONE',  ( -3.175426480542816510, 5.499999999999865885, -86.87500000000007105 ) ) ;
#20846 = ADVANCED_FACE ( 'NONE', ( #559 ), #7617, .T. ) ;
#20847 = CARTESIAN_POINT ( 'NONE',  ( -5.412658773652684552, -3.125000000000099920, -104.9330127018922525 ) ) ;
#20848 = CARTESIAN_POINT ( 'NONE',  ( 0.000000000000000000, 5.999999999999977796, -52.21132486540525264 ) ) ;
#20849 = CARTESIAN_POINT ( 'NONE',  ( 3.175426480543072749, 5.499999999999865885, -166.6249999999999716 ) ) ;
#20850 = CARTESIAN_POINT ( 'NONE',  ( 5.801553858104719019, -9.346157964213302805, -26.58091173639827431 ) ) ;
#20851 = ORIENTED_EDGE ( 'NONE', *, *, #10093, .F. ) ;
#20852 = FACE_OUTER_BOUND ( 'NONE', #1508, .T. ) ;
#20853 = FILL_AREA_STYLE ('',( #13212 ) ) ;
#20854 = CARTESIAN_POINT ( 'NONE',  ( -4.763139720814407951, 2.749999999999946709, -173.7500000000000284 ) ) ;
#20855 = DIRECTION ( 'NONE',  ( -7.147005652999508048E-36, 5.642372883946980038E-36, 1.000000000000000000 ) ) ;
#20856 = CARTESIAN_POINT ( 'NONE',  ( 3.175426480543072749, 5.499999999999865885, -165.1249999999999716 ) ) ;
#20857 = CARTESIAN_POINT ( 'NONE',  ( 113.8749999999998721, 1.767766952966431937, -1.767766952966209892 ) ) ;
#20858 = AXIS2_PLACEMENT_3D ( 'NONE', #21760, #703, #17162 ) ;
#20859 = CARTESIAN_POINT ( 'NONE',  ( -4.763139720814407951, 2.749999999999946709, -104.7500000000000142 ) ) ;
#20860 = CARTESIAN_POINT ( 'NONE',  ( -3.464101615137757051, -5.999999999999979572, -159.5863248654051176 ) ) ;
#20861 = CARTESIAN_POINT ( 'NONE',  ( -5.999999999999963585, -1.487416814333745711E-14, -122.9136751345948255 ) ) ;
#20862 = CARTESIAN_POINT ( 'NONE',  ( 4.763139720814407951, 2.750000000000002665, -100.7500000000000000 ) ) ;
#20863 = CARTESIAN_POINT ( 'NONE',  ( 13.64882486540520290, 2.500000000000205169, -1.035533905932809473 ) ) ;
#20864 = CARTESIAN_POINT ( 'NONE',  ( 158.5461002691896510, -2.071067811865468400, 4.999999999999989342 ) ) ;
#20865 = CARTESIAN_POINT ( 'NONE',  ( 0.2014817752041039023, -15.64225424449952229, 7.847953382956076140 ) ) ;
#20866 = CARTESIAN_POINT ( 'NONE',  ( 12.25000000000014921, -1.873492889144845464, -1.873492889145123019 ) ) ;
#20867 = CARTESIAN_POINT ( 'NONE',  ( 116.6249999999999716, -1.767766952966459693, -1.767766952966209892 ) ) ;
#20868 = CARTESIAN_POINT ( 'NONE',  ( 12.71132486540518869, 2.500000000000002220, 0.000000000000000000 ) ) ;
#20869 = CARTESIAN_POINT ( 'NONE',  ( 105.4377832217621176, 1.849990392679562001, 0.7662911109078888172 ) ) ;
#20870 = CARTESIAN_POINT ( 'NONE',  ( 0.000000000000000000, -5.999999999999991118, -85.96132486540520290 ) ) ;
#20871 = VERTEX_POINT ( 'NONE', #2707 ) ;
#20872 = VECTOR ( 'NONE', #26289, 1000.000000000000000 ) ;
#20873 = EDGE_CURVE ( 'NONE', #18702, #29957, #19039, .T. ) ;
#20874 = ORIENTED_EDGE ( 'NONE', *, *, #28855, .T. ) ;
#20875 = CARTESIAN_POINT ( 'NONE',  ( 124.9999999999999432, -65.00000000000000000, 8.000000000000007105 ) ) ;
#20876 = CARTESIAN_POINT ( 'NONE',  ( 152.1562500000000284, -6.000000000000005329, 2.485281374238555774 ) ) ;
#20877 = VERTEX_POINT ( 'NONE', #28505 ) ;
#20878 = CIRCLE ( 'NONE', #19396, 16.18577070100374726 ) ;
#20879 = CARTESIAN_POINT ( 'NONE',  ( -3.175426480542816510, -5.500000000000057732, -113.3750000000000568 ) ) ;
#20880 = CARTESIAN_POINT ( 'NONE',  ( 21.18750000000013500, 1.097466725451679892, -2.649519052838298805 ) ) ;
#20881 =( BOUNDED_CURVE ( )  B_SPLINE_CURVE ( 3, ( #9000, #22675, #30182, #6832 ),
 .UNSPECIFIED., .F., .F. ) 
 B_SPLINE_CURVE_WITH_KNOTS ( ( 4, 4 ),
 ( 1.570796326794896558, 2.746801533890022906 ),
 .UNSPECIFIED. ) 
 CURVE ( )  GEOMETRIC_REPRESENTATION_ITEM ( )  RATIONAL_B_SPLINE_CURVE ( ( 1.000000000000000000, 0.8880335295585641830, 0.8880335295585641830, 1.000000000000000000 ) ) 
 REPRESENTATION_ITEM ( '' )  );
#20882 = EDGE_CURVE ( 'NONE', #4865, #886, #4543, .T. ) ;
#20883 = CARTESIAN_POINT ( 'NONE',  ( 5.412658773652712085, -3.125000000000086153, -134.4330127018922383 ) ) ;
#20884 = ORIENTED_EDGE ( 'NONE', *, *, #17395, .T. ) ;
#20885 =( NAMED_UNIT ( * ) SI_UNIT ( $, .STERADIAN. ) SOLID_ANGLE_UNIT ( ) );
#20886 = CARTESIAN_POINT ( 'NONE',  ( -7.216878364870328078, 0.000000000000000000, -168.6919872981078186 ) ) ;
#20887 = CARTESIAN_POINT ( 'NONE',  ( -5.412658773652739619, 3.124999999999975131, -180.8169872981077901 ) ) ;
#20888 = AXIS2_PLACEMENT_3D ( 'NONE', #15343, #24821, #3768 ) ;
#20889 = CARTESIAN_POINT ( 'NONE',  ( 10.87499999999996803, 1.414213562373312083, -1.414213562373145550 ) ) ;
#20890 = CARTESIAN_POINT ( 'NONE',  ( 0.7528903888467955996, -15.55266350887514903, -8.022782003273663420 ) ) ;
#20891 = CARTESIAN_POINT ( 'NONE',  ( 6.000000000000000888, 7.762456499804235646E-14, -144.6636751345948255 ) ) ;
#20892 =( BOUNDED_SURFACE ( )  B_SPLINE_SURFACE ( 3, 2, ( 
 ( #26727, #5690, #24588 ),
 ( #29345, #21852, #29185 ),
 ( #3537, #15102, #19993 ),
 ( #22154, #797, #24285 ),
 ( #5241, #5392, #932 ),
 ( #17412, #3232, #12968 ),
 ( #12512, #17564, #10490 ),
 ( #12658, #8146, #16963 ) ),
 .UNSPECIFIED., .F., .F., .T. ) 
 B_SPLINE_SURFACE_WITH_KNOTS ( ( 4, 2, 2, 4 ),
 ( 3, 3 ),
 ( 1.570796326794896558, 2.158798930342461730, 2.452800232116244317, 2.746801533890027347 ),
 ( 0.000000000000000000, 1.000000000000000000 ),
 .UNSPECIFIED. ) 
 GEOMETRIC_REPRESENTATION_ITEM ( )  RATIONAL_B_SPLINE_SURFACE ( (
 ( 1.000000000000000000, 1.000000000000000000, 1.000000000000000000),
 ( 1.000000000000000000, 1.000817594376257835, 1.000000000000000000),
 ( 1.000000000000000000, 0.9690373989631937413, 1.000000000000000000),
 ( 1.000000000000000000, 0.8952806170301043087, 1.000000000000000000),
 ( 1.000000000000000000, 0.8665500556586805958, 1.000000000000000000),
 ( 1.000000000000000000, 0.8091552864627657993, 1.000000000000000000),
 ( 1.000000000000000000, 0.7805842023125286744, 1.000000000000000000),
 ( 1.000000000000000000, 0.7576044462920088485, 1.000000000000000000) ) ) 
 REPRESENTATION_ITEM ( '' )  SURFACE ( )  );
#20893 = CIRCLE ( 'NONE', #28697, 1.999999999999998224 ) ;
#20895 = VECTOR ( 'NONE', #12926, 1000.000000000000000 ) ;
#20894 = CARTESIAN_POINT ( 'NONE',  ( 153.2886751345948255, 5.500000000000005329, 0.000000000000000000 ) ) ;
#20896 = CARTESIAN_POINT ( 'NONE',  ( -4.999999999999990230, -55.00000000000002132, -7.500000000000007105 ) ) ;
#20897 = CARTESIAN_POINT ( 'NONE',  ( 157.5863248654052597, 0.000000000000000000, 5.500000000000005329 ) ) ;
#20898 = CARTESIAN_POINT ( 'NONE',  ( 112.5002832217623023, 1.308140751793696044, 1.308140751793640533 ) ) ;
#20899 = CARTESIAN_POINT ( 'NONE',  ( 5.412658773652739619, 3.124999999999988898, -73.31698729810781856 ) ) ;
#20900 = CARTESIAN_POINT ( 'NONE',  ( -5.412658773652739619, 3.124999999999975131, -59.31698729810786119 ) ) ;
#20901 = CARTESIAN_POINT ( 'NONE',  ( 6.000000000000000888, 1.743066579297358182E-13, -112.5863248654052029 ) ) ;
#20902 = CARTESIAN_POINT ( 'NONE',  ( -7.216878364870328078, 0.000000000000000000, -181.5580127018922383 ) ) ;
#20903 = CARTESIAN_POINT ( 'NONE',  ( -1.000000000000001776, -9.000000000000007105, -4.000000000000005329 ) ) ;
#20904 = CARTESIAN_POINT ( 'NONE',  ( -5.999999999999963585, -1.487416814333745711E-14, -71.91367513459482552 ) ) ;
#20905 = CARTESIAN_POINT ( 'NONE',  ( -5.999999999999963585, -1.487416814333745711E-14, -71.33632486540521711 ) ) ;
#20906 = CARTESIAN_POINT ( 'NONE',  ( -3.175426480542816510, 5.499999999999865885, -124.3749999999999858 ) ) ;
#20907 = CARTESIAN_POINT ( 'NONE',  ( 135.0000000000000284, -8.793943684514120562, -7.941504649977358277 ) ) ;
#20908 = ORIENTED_EDGE ( 'NONE', *, *, #15386, .F. ) ;
#20909 = CARTESIAN_POINT ( 'NONE',  ( 22.93749999999999289, -1.097466725451499370, 2.649519052838358757 ) ) ;
#20910 = CARTESIAN_POINT ( 'NONE',  ( 143.7261751345948539, -3.889087296526011706, -3.889087296526011706 ) ) ;
#20911 = LINE ( 'NONE', #9071, #6448 ) ;
#20912 = ORIENTED_EDGE ( 'NONE', *, *, #14952, .F. ) ;
#20913 = CARTESIAN_POINT ( 'NONE',  ( 108.1872167782373850, -1.849990392679472073, -0.7662911109077087390 ) ) ;
#20914 = CARTESIAN_POINT ( 'NONE',  ( 2.081668171172167281E-16, 3.582034040661430693E-16, -2.499999999999999112 ) ) ;
#20915 = ADVANCED_FACE ( 'NONE', ( #10252 ), #23920, .T. ) ;
#20916 = CARTESIAN_POINT ( 'NONE',  ( 3.608439182435180470, 6.249999999999982236, -109.1919872981078043 ) ) ;
#20917 = CARTESIAN_POINT ( 'NONE',  ( 16.96132486540522066, 1.110223024625156540E-13, 2.500000000000002220 ) ) ;
#20918 = ORIENTED_EDGE ( 'NONE', *, *, #12545, .F. ) ;
#20919 = DIRECTION ( 'NONE',  ( 1.000000000000000000, -5.551115123125773458E-17, -1.260129944081490338E-35 ) ) ;
#20920 = ORIENTED_EDGE ( 'NONE', *, *, #27090, .T. ) ;
#20921 = DIRECTION ( 'NONE',  ( 0.000000000000000000, -1.000000000000000000, 0.000000000000000000 ) ) ;
#20922 = CARTESIAN_POINT ( 'NONE',  ( 136.2187500000000284, 2.485281374238555774, -6.000000000000005329 ) ) ;
#20923 = EDGE_CURVE ( 'NONE', #22647, #11887, #12426, .T. ) ;
#20924 = CARTESIAN_POINT ( 'NONE',  ( 2.775557561562891351E-14, 6.250000000000033751, -140.5669872981077901 ) ) ;
#20925 = CARTESIAN_POINT ( 'NONE',  ( 11.56250000000000000, 1.097466725451619718, 2.649519052838478661 ) ) ;
#20926 = PRESENTATION_LAYER_ASSIGNMENT (  '', '', ( #8718 ) ) ;
#20927 = CARTESIAN_POINT ( 'NONE',  ( 14.78867513459480776, -2.500000000000002220, -5.551115123125782702E-14 ) ) ;
#20928 = CARTESIAN_POINT ( 'NONE',  ( 23.12500000000003553, 1.414213562373090038, 1.414213562373034527 ) ) ;
#20929 = PRESENTATION_STYLE_ASSIGNMENT (( #4010 ) ) ;
#20930 = CARTESIAN_POINT ( 'NONE',  ( 2.775557561562891351E-14, 6.250000000000033751, -66.43301270189222407 ) ) ;
#20931 = CARTESIAN_POINT ( 'NONE',  ( 135.7516005668298078, -9.165151352129356610, -8.000000000000007105 ) ) ;
#20932 = CARTESIAN_POINT ( 'NONE',  ( 144.6413997308104342, 2.071067811865468400, -4.999999999999989342 ) ) ;
#20933 = DIRECTION ( 'NONE',  ( -7.147005652999508048E-36, 5.642372883946980038E-36, 1.000000000000000000 ) ) ;
#20934 = CARTESIAN_POINT ( 'NONE',  ( -5.999999999999963585, 1.780251999655701777E-13, -70.41367513459482552 ) ) ;
#20935 = CARTESIAN_POINT ( 'NONE',  ( -5.999999999999963585, 1.607695154586726627, -164.9806624327025588 ) ) ;
#20936 = FACE_OUTER_BOUND ( 'NONE', #6538, .T. ) ;
#20937 = DIRECTION ( 'NONE',  ( 1.000000000000000000, -0.000000000000000000, 0.000000000000000000 ) ) ;
#20938 = CARTESIAN_POINT ( 'NONE',  ( 108.5000000000000000, -2.500000000000002220, 2.220446049250313081E-13 ) ) ;
#20939 = DIRECTION ( 'NONE',  ( -7.147005652999508048E-36, 5.642372883946980038E-36, 1.000000000000000000 ) ) ;
#20940 = CARTESIAN_POINT ( 'NONE',  ( -6.350852961085760029, -1.281975124255709124E-13, -125.6250000000000426 ) ) ;
#20941 = CARTESIAN_POINT ( 'NONE',  ( -5.412658773652684552, -3.125000000000099920, -143.9330127018922383 ) ) ;
#20942 = ORIENTED_EDGE ( 'NONE', *, *, #19889, .T. ) ;
#20943 = VECTOR ( 'NONE', #5517, 1000.000000000000000 ) ;
#20944 = CARTESIAN_POINT ( 'NONE',  ( -4.763139720814407951, -2.750000000000016431, -55.00000000000004974 ) ) ;
#20945 = CARTESIAN_POINT ( 'NONE',  ( -3.464101615137725076, 5.999999999999979572, -124.0863248654052455 ) ) ;
#20946 = CARTESIAN_POINT ( 'NONE',  ( -5.999999999999963585, 8.134310703387671600E-14, -120.8363248654052171 ) ) ;
#20947 = CARTESIAN_POINT ( 'NONE',  ( 5.999999999999949374, -1.607695154586841868, -163.6533121635129646 ) ) ;
#20948 = ORIENTED_EDGE ( 'NONE', *, *, #13140, .F. ) ;
#20949 = CARTESIAN_POINT ( 'NONE',  ( 120.2497167782375271, -1.308140751793529510, -1.308140751793640533 ) ) ;
#20950 = CARTESIAN_POINT ( 'NONE',  ( 137.5312500000000284, -2.485281374238556218, -6.000000000000005329 ) ) ;
#20951 = EDGE_CURVE ( 'NONE', #18704, #21171, #264, .T. ) ;
#20952 = CARTESIAN_POINT ( 'NONE',  ( 3.608439182435180470, -6.249999999999997335, -103.6919872981078470 ) ) ;
#20953 = CARTESIAN_POINT ( 'NONE',  ( 143.0699251345947971, 2.278174593052322283, 5.499999999999701572 ) ) ;
#20954 = CARTESIAN_POINT ( 'NONE',  ( 160.2976497308104342, 0.000000000000000000, 5.000000000000004441 ) ) ;
#20955 = CARTESIAN_POINT ( 'NONE',  ( 14.39882486540531303, -1.035533905932568999, -2.499999999999904521 ) ) ;
#20956 = CIRCLE ( 'NONE', #12659, 0.5000000000000004441 ) ;
#20957 = EDGE_CURVE ( 'NONE', #18615, #8469, #7914, .T. ) ;
#20958 = CARTESIAN_POINT ( 'NONE',  ( 4.763139720814407951, 2.750000000000002665, -139.7500000000000284 ) ) ;
#20959 = ORIENTED_EDGE ( 'NONE', *, *, #25688, .F. ) ;
#20960 = PRESENTATION_LAYER_ASSIGNMENT (  '', '', ( #25839 ) ) ;
#20961 = CARTESIAN_POINT ( 'NONE',  ( 13.68750000000000178, -0.8284271247459350507, -2.000000000000091926 ) ) ;
#20962 = ORIENTED_EDGE ( 'NONE', *, *, #4037, .F. ) ;
#20963 = CARTESIAN_POINT ( 'NONE',  ( 4.763139720814407951, -2.749999999999988454, -62.00000000000000000 ) ) ;
#20964 = CARTESIAN_POINT ( 'NONE',  ( 10.00000000000015099, 0.5728653053451536747, -2.302908512320128942 ) ) ;
#20965 = DIRECTION ( 'NONE',  ( 0.3742395684071963546, 0.4425345409093133231, -0.8149281720130793216 ) ) ;
#20966 = CARTESIAN_POINT ( 'NONE',  ( -3.608439182435115633, 6.249999999999965361, -88.80801270189223828 ) ) ;
#20967 = CIRCLE ( 'NONE', #13144, 15.00000000000000000 ) ;
#20968 = CARTESIAN_POINT ( 'NONE',  ( 152.3511751345948539, -3.889087296526011706, 3.889087296526011706 ) ) ;
#20969 = CARTESIAN_POINT ( 'NONE',  ( 105.6872167782375413, 1.849990392679591977, 0.7662911109080692285 ) ) ;
#20970 = DIRECTION ( 'NONE',  ( -7.147005652999508048E-36, 5.642372883946980038E-36, 1.000000000000000000 ) ) ;
#20971 = DIRECTION ( 'NONE',  ( 1.000000000000000000, 0.000000000000000000, 0.000000000000000000 ) ) ;
#20972 = CARTESIAN_POINT ( 'NONE',  ( 120.5627832217621460, 0.7662911109078287542, 1.849990392679652151 ) ) ;
#20973 = CARTESIAN_POINT ( 'NONE',  ( 0.000000000000000000, 5.499999999999991118, -150.0000000000000284 ) ) ;
#20974 = CARTESIAN_POINT ( 'NONE',  ( 139.5000000000000000, -8.946933499675704837, 8.000000000000007105 ) ) ;
#20975 = AXIS2_PLACEMENT_3D ( 'NONE', #22741, #1684, #13551 ) ;
#20976 = CARTESIAN_POINT ( 'NONE',  ( -4.763139720814407951, -2.750000000000016431, -134.5000000000000000 ) ) ;
#20977 = CARTESIAN_POINT ( 'NONE',  ( 3.608439182435180470, -6.249999999999997335, -157.0580127018922383 ) ) ;
#20978 = CARTESIAN_POINT ( 'NONE',  ( 0.000000000000000000, 0.000000000000000000, 0.000000000000000000 ) ) ;
#20979 = LINE ( 'NONE', #25716, #7570 ) ;
#20980 = PRODUCT_DEFINITION_SHAPE ( 'NONE', 'NONE',  #30419 ) ;
#20981 = CARTESIAN_POINT ( 'NONE',  ( -4.763139720814407951, 2.749999999999946709, -80.74999999999998579 ) ) ;
#20982 = DIRECTION ( 'NONE',  ( 1.000000000000000000, 0.000000000000000000, 0.000000000000000000 ) ) ;
#20983 = CARTESIAN_POINT ( 'NONE',  ( -6.350852961085760029, -1.281975124255709124E-13, -64.12500000000001421 ) ) ;
#20984 =( BOUNDED_CURVE ( )  B_SPLINE_CURVE ( 2, ( #6831, #16257, #4531, #13956, #516, #19577, #5567, #2823, #14538 ),
 .UNSPECIFIED., .F., .F. ) 
 B_SPLINE_CURVE_WITH_KNOTS ( ( 3, 2, 2, 2, 3 ),
 ( 0.3527777777777778012, 0.3537037037037036868, 0.3555555555555555691, 0.3574074074074073959, 0.3583333333333333370 ),
 .UNSPECIFIED. ) 
 CURVE ( )  GEOMETRIC_REPRESENTATION_ITEM ( )  RATIONAL_B_SPLINE_CURVE ( ( 0.9330127018922194093, 0.9330127018922214077, 1.000000000000000000, 0.8660254037844388186, 1.000000000000000000, 0.8660254037844388186, 1.000000000000000000, 0.9330127018922194093, 0.9330127018922194093 ) ) 
 REPRESENTATION_ITEM ( '' )  );
#20985 = CARTESIAN_POINT ( 'NONE',  ( 149.6398502691896510, -3.535533905932752852, 3.535533905932725318 ) ) ;
#20986 = CARTESIAN_POINT ( 'NONE',  ( 0.000000000000000000, -5.999999999999991118, -88.03867513459483973 ) ) ;
#20987 = CARTESIAN_POINT ( 'NONE',  ( -2.081668171172168020E-16, -5.204170427930420051E-17, 2.499999999999999112 ) ) ;
#20988 = CARTESIAN_POINT ( 'NONE',  ( 158.6250000000000568, 0.000000000000000000, -6.000000000000005329 ) ) ;
#20989 = CARTESIAN_POINT ( 'NONE',  ( 19.31250000000010303, -0.8284271247459350507, 2.000000000000091926 ) ) ;
#20990 = CARTESIAN_POINT ( 'NONE',  ( 138.8511751345948255, -3.889087296526011706, 3.889087296526011706 ) ) ;
#20991 = EDGE_CURVE ( 'NONE', #26834, #7517, #16954, .T. ) ;
#20992 = CARTESIAN_POINT ( 'NONE',  ( -6.000000000000007105, -1.607695154586655129, -98.84668783648703538 ) ) ;
#20993 = CARTESIAN_POINT ( 'NONE',  ( 118.7497167782375982, 1.308140751793696044, 1.308140751793640533 ) ) ;
#20994 = PRESENTATION_STYLE_ASSIGNMENT (( #11648 ) ) ;
#20995 = ADVANCED_FACE ( 'NONE', ( #12880 ), #8059, .T. ) ;
#20996 = EDGE_LOOP ( 'NONE', ( #1279, #11261, #14720, #26356 ) ) ;
#20997 = CARTESIAN_POINT ( 'NONE',  ( 150.8437500000000284, -6.000000000000005329, -2.485281374238555774 ) ) ;
#20998 = VECTOR ( 'NONE', #16325, 1000.000000000000114 ) ;
#20999 = CARTESIAN_POINT ( 'NONE',  ( 115.8127832217621460, -1.849990392679472073, 0.7662911109078888172 ) ) ;
#21000 = LINE ( 'NONE', #18095, #28328 ) ;
#21001 = ORIENTED_EDGE ( 'NONE', *, *, #26950, .T. ) ;
#21002 = ORIENTED_EDGE ( 'NONE', *, *, #9259, .F. ) ;
#21003 = ORIENTED_EDGE ( 'NONE', *, *, #15240, .T. ) ;
#21004 = CARTESIAN_POINT ( 'NONE',  ( -4.763139720814407951, 2.749999999999946709, -86.75000000000000000 ) ) ;
#21005 = CARTESIAN_POINT ( 'NONE',  ( 3.608439182435180470, -6.249999999999997335, -110.5580127018922241 ) ) ;
#21006 = EDGE_LOOP ( 'NONE', ( #187, #22720, #27444, #10916 ) ) ;
#21007 = CYLINDRICAL_SURFACE ( 'NONE', #15239, 5.500000000000000000 ) ;
#21008 = CARTESIAN_POINT ( 'NONE',  ( 156.0788997308104058, -4.999999999999989342, 2.071067811865468400 ) ) ;
#21009 = CARTESIAN_POINT ( 'NONE',  ( 6.000000000000000888, -1.859271017917181981E-14, -63.08632486540521711 ) ) ;
#21010 = ORIENTED_EDGE ( 'NONE', *, *, #20991, .F. ) ;
#21011 = CARTESIAN_POINT ( 'NONE',  ( 3.464101615137852974, 5.999999999999884537, -93.41367513459479710 ) ) ;
#21012 = CARTESIAN_POINT ( 'NONE',  ( 4.763139720814407951, -2.749999999999988454, -168.4999999999999716 ) ) ;
#21013 = CARTESIAN_POINT ( 'NONE',  ( 0.000000000000000000, 5.499999999999991118, -156.0000000000000284 ) ) ;
#21014 = CARTESIAN_POINT ( 'NONE',  ( 113.3124999999997300, -1.035533905932598975, 2.500000000000144773 ) ) ;
#21015 = CARTESIAN_POINT ( 'NONE',  ( -4.763139720814407951, 2.749999999999946709, -103.2500000000000142 ) ) ;
#21016 = CARTESIAN_POINT ( 'NONE',  ( 5.999999999999949374, 1.607695154586804565, -87.59668783648704959 ) ) ;
#21017 = CARTESIAN_POINT ( 'NONE',  ( -6.350852961085760029, -1.281975124255709124E-13, -98.62500000000005684 ) ) ;
#21018 = CARTESIAN_POINT ( 'NONE',  ( 160.7023502691896510, 0.000000000000000000, -5.000000000000004441 ) ) ;
#21019 = CARTESIAN_POINT ( 'NONE',  ( 134.9999999999997158, -6.982120021893415185, 8.500000000000007105 ) ) ;
#21020 = AXIS2_PLACEMENT_3D ( 'NONE', #19697, #28475, #7146 ) ;
#21021 = ORIENTED_EDGE ( 'NONE', *, *, #19430, .T. ) ;
#21022 = CARTESIAN_POINT ( 'NONE',  ( 12.12500000000010836, -2.649519052838111843, -5.551115123125782702E-14 ) ) ;
#21023 = CARTESIAN_POINT ( 'NONE',  ( 114.4374999999998010, -2.499999999999964473, 1.035533905932929599 ) ) ;
#21024 = LINE ( 'NONE', #14147, #7036 ) ;
#21025 = EDGE_CURVE ( 'NONE', #16384, #20652, #29718, .T. ) ;
#21026 = CARTESIAN_POINT ( 'NONE',  ( 108.1877832217622881, 0.7662911109077388261, -1.849990392679291551 ) ) ;
#21027 = CARTESIAN_POINT ( 'NONE',  ( 161.0957217774242736, 0.3141511273712443986, 5.595721777424251364 ) ) ;
#21028 = EDGE_CURVE ( 'NONE', #11352, #8549, #22371, .T. ) ;
#21029 = ORIENTED_EDGE ( 'NONE', *, *, #10694, .T. ) ;
#21030 = DIRECTION ( 'NONE',  ( 1.000000000000000000, -5.551115123125774074E-17, -1.260129944081490338E-35 ) ) ;
#21031 = DIRECTION ( 'NONE',  ( -7.147005652999508048E-36, 5.642372883946980038E-36, 1.000000000000000000 ) ) ;
#21032 = CARTESIAN_POINT ( 'NONE',  ( 107.0622167782373708, -1.849990392679381701, 0.7662911109079489913 ) ) ;
#21033 =( BOUNDED_CURVE ( )  B_SPLINE_CURVE ( 2, ( #25507, #11432, #9087, #4159, #4773, #9396, #30124, #20776, #10 ),
 .UNSPECIFIED., .F., .F. ) 
 B_SPLINE_CURVE_WITH_KNOTS ( ( 3, 2, 2, 2, 3 ),
 ( 0.7750000000000000222, 0.7759259259259259078, 0.7777777777777777901, 0.7796296296296296724, 0.7805555555555555580 ),
 .UNSPECIFIED. ) 
 CURVE ( )  GEOMETRIC_REPRESENTATION_ITEM ( )  RATIONAL_B_SPLINE_CURVE ( ( 0.9330127018922194093, 0.9330127018922194093, 1.000000000000000000, 0.8660254037844388186, 1.000000000000000000, 0.8660254037844388186, 1.000000000000000000, 0.9330127018922194093, 0.9330127018922194093 ) ) 
 REPRESENTATION_ITEM ( '' )  );
#21034 = CARTESIAN_POINT ( 'NONE',  ( 111.2113248654051176, -1.999999999999946265, 0.000000000000000000 ) ) ;
#21035 = ORIENTED_EDGE ( 'NONE', *, *, #27893, .T. ) ;
#21036 = CARTESIAN_POINT ( 'NONE',  ( 5.196152422706629359, -2.999999999999988898, -141.2113248654052313 ) ) ;
#21037 = ORIENTED_EDGE ( 'NONE', *, *, #23791, .T. ) ;
#21038 = CARTESIAN_POINT ( 'NONE',  ( 149.1562500000000284, -6.000000000000005329, 2.485281374238555774 ) ) ;
#21039 = CARTESIAN_POINT ( 'NONE',  ( -4.763139720814407951, 2.749999999999946709, -113.7500000000000142 ) ) ;
#21040 = CARTESIAN_POINT ( 'NONE',  ( 20.50000000000012790, 1.873492889145011997, 1.873492889144734441 ) ) ;
#21041 = CARTESIAN_POINT ( 'NONE',  ( -3.608439182435052128, -6.250000000000110134, -128.8080127018922383 ) ) ;
#21042 = ORIENTED_EDGE ( 'NONE', *, *, #88, .F. ) ;
#21043 = CARTESIAN_POINT ( 'NONE',  ( 158.6175748654052313, 5.500000000000012434, -2.278174593052012309 ) ) ;
#21044 = CARTESIAN_POINT ( 'NONE',  ( 3.608439182435180470, 6.249999999999982236, -167.6919872981078186 ) ) ;
#21045 = CARTESIAN_POINT ( 'NONE',  ( 109.3750000000000142, -1.767766952966320915, 1.767766952966431937 ) ) ;
#21046 = ORIENTED_EDGE ( 'NONE', *, *, #17183, .F. ) ;
#21047 = CARTESIAN_POINT ( 'NONE',  ( -5.196152422706601826, 2.999999999999975131, -95.46132486540520290 ) ) ;
#21048 = CARTESIAN_POINT ( 'NONE',  ( 6.000000000000000888, -6.507448562710137091E-15, -175.5863248654052029 ) ) ;
#21049 = CARTESIAN_POINT ( 'NONE',  ( 23.46132486540525264, 1.110223024625156540E-13, -2.500000000000002220 ) ) ;
#21050 = CARTESIAN_POINT ( 'NONE',  ( 108.6252832217621886, 5.551115123125782702E-14, 1.849990392679634610 ) ) ;
#21051 = CARTESIAN_POINT ( 'NONE',  ( 3.608439182435180470, 6.249999999999982236, -174.5580127018922667 ) ) ;
#21052 = CARTESIAN_POINT ( 'NONE',  ( -39.00000000000000000, -20.00000000000021316, -4.000000000000003553 ) ) ;
#21053 = CARTESIAN_POINT ( 'NONE',  ( -5.999999999999956479, -1.607695154586745057, -101.8466878364870354 ) ) ;
#21054 = CARTESIAN_POINT ( 'NONE',  ( -4.999999999999990230, -24.99999999999999289, -8.000000000000007105 ) ) ;
#21055 = CARTESIAN_POINT ( 'NONE',  ( -2.775557561562891351E-14, -5.500000000000115463, -120.7500000000000284 ) ) ;
#21056 = CARTESIAN_POINT ( 'NONE',  ( 135.0000000000000000, -7.896660352823049678, -8.122336518022390095 ) ) ;
#21057 = ORIENTED_EDGE ( 'NONE', *, *, #21744, .F. ) ;
#21058 = CARTESIAN_POINT ( 'NONE',  ( 22.31250000000015277, -1.097466725451439196, -2.649519052838358757 ) ) ;
#21059 = CARTESIAN_POINT ( 'NONE',  ( 6.000000000000000888, -3.330669073875464691E-16, -7.560779664488942560E-35 ) ) ;
#21060 = CARTESIAN_POINT ( 'NONE',  ( -5.196152422706601826, 2.999999999999975131, -122.4613248654052313 ) ) ;
#21061 = CARTESIAN_POINT ( 'NONE',  ( 18.33632486540526330, -1.767766952966265404, -1.767766952966542959 ) ) ;
#21062 = EDGE_CURVE ( 'NONE', #3053, #22801, #9117, .T. ) ;
#21063 = ORIENTED_EDGE ( 'NONE', *, *, #25275, .F. ) ;
#21064 = CARTESIAN_POINT ( 'NONE',  ( 109.6872167782374561, 1.849990392679562001, 0.7662911109080090544 ) ) ;
#21065 = CARTESIAN_POINT ( 'NONE',  ( 151.0238248654052313, 3.889087296526011706, -3.889087296526011706 ) ) ;
#21066 = CARTESIAN_POINT ( 'NONE',  ( 5.412658773652739619, 3.124999999999988898, -107.8169872981078470 ) ) ;
#21067 = SURFACE_STYLE_USAGE ( .BOTH. , #11724 ) ;
#21068 = ORIENTED_EDGE ( 'NONE', *, *, #15426, .F. ) ;
#21069 = CARTESIAN_POINT ( 'NONE',  ( 22.10117513459489302, 1.035533905932869425, -2.500000000000024425 ) ) ;
#21070 =( BOUNDED_CURVE ( )  B_SPLINE_CURVE ( 2, ( #30204, #30355, #30047, #4845, #9322, #7159, #14272, #16572, #8870 ),
 .UNSPECIFIED., .F., .F. ) 
 B_SPLINE_CURVE_WITH_KNOTS ( ( 3, 2, 2, 2, 3 ),
 ( 0.06250000000000052736, 0.06875000000000031086, 0.07500000000000006661, 0.08124999999999985012, 0.08749999999999961975 ),
 .UNSPECIFIED. ) 
 CURVE ( )  GEOMETRIC_REPRESENTATION_ITEM ( )  RATIONAL_B_SPLINE_CURVE ( ( 0.9999999999999935607, 0.9238795325112931778, 1.000000000000000000, 0.9238795325112867385, 1.000000000000000000, 0.9238795325112867385, 1.000000000000000000, 0.9238795325112912904, 0.9999999999999954481 ) ) 
 REPRESENTATION_ITEM ( '' )  );
#21071 = DIRECTION ( 'NONE',  ( 1.000000000000000000, -5.551115123125773458E-17, -1.260129944081490338E-35 ) ) ;
#21072 = VERTEX_POINT ( 'NONE', #10722 ) ;
#21073 = VERTEX_POINT ( 'NONE', #12727 ) ;
#21074 = CARTESIAN_POINT ( 'NONE',  ( 138.7500000000000284, -6.000000000000005329, 0.000000000000000000 ) ) ;
#21075 =( BOUNDED_CURVE ( )  B_SPLINE_CURVE ( 2, ( #16030, #18464, #2316, #29797, #29946, #25488, #27784, #11566, #4453 ),
 .UNSPECIFIED., .F., .T. ) 
 B_SPLINE_CURVE_WITH_KNOTS ( ( 3, 2, 2, 2, 3 ),
 ( 0.5638888888888888840, 0.5648148148148147696, 0.5666666666666666519, 0.5685185185185185341, 0.5694444444444444198 ),
 .UNSPECIFIED. ) 
 CURVE ( )  GEOMETRIC_REPRESENTATION_ITEM ( )  RATIONAL_B_SPLINE_CURVE ( ( 0.9330127018922194093, 0.9330127018922194093, 1.000000000000000000, 0.8660254037844388186, 1.000000000000000000, 0.8660254037844388186, 1.000000000000000000, 0.9330127018922234061, 0.9330127018922194093 ) ) 
 REPRESENTATION_ITEM ( '' )  );
#21076 = CARTESIAN_POINT ( 'NONE',  ( 3.608439182435180470, -6.249999999999997335, -142.6919872981078186 ) ) ;
#21077 = DIRECTION ( 'NONE',  ( 1.000000000000000000, 0.000000000000000000, 0.000000000000000000 ) ) ;
#21078 = CARTESIAN_POINT ( 'NONE',  ( 11.12500000000010658, 1.665334536937734811E-13, -2.649519052838444910 ) ) ;
#21079 = CARTESIAN_POINT ( 'NONE',  ( -5.196152422706573404, -3.000000000000002665, -93.71132486540523132 ) ) ;
#21080 = CARTESIAN_POINT ( 'NONE',  ( 18.50000000000012790, -1.999999999999835243, 0.000000000000000000 ) ) ;
#21081 = CARTESIAN_POINT ( 'NONE',  ( -5.999999999999982236, -1.607695154586700426, -130.3466878364870638 ) ) ;
#21082 = CARTESIAN_POINT ( 'NONE',  ( 117.5238248654049897, 0.8284271247463557142, -1.999999999999791278 ) ) ;
#21083 = CARTESIAN_POINT ( 'NONE',  ( 142.0163997308104626, 4.999999999999989342, 2.071067811865468400 ) ) ;
#21084 = CARTESIAN_POINT ( 'NONE',  ( 11.85117513459488592, -2.499999999999964473, -1.035533905932749299 ) ) ;
#21085 = LINE ( 'NONE', #23691, #3451 ) ;
#21086 = ADVANCED_FACE ( 'NONE', ( #1462 ), #8380, .T. ) ;
#21087 = CARTESIAN_POINT ( 'NONE',  ( 0.000000000000000000, -5.999999999999991118, -146.5386751345948539 ) ) ;
#21088 = ADVANCED_FACE ( 'NONE', ( #27405 ), #15801, .T. ) ;
#21089 = CARTESIAN_POINT ( 'NONE',  ( 6.000000000000000888, -1.859271017917181981E-14, -101.1636751345948397 ) ) ;
#21090 = FACE_OUTER_BOUND ( 'NONE', #28254, .T. ) ;
#21091 = CARTESIAN_POINT ( 'NONE',  ( 109.4999999999998579, -2.499999999999891198, 2.220446049250313081E-13 ) ) ;
#21092 = CARTESIAN_POINT ( 'NONE',  ( 0.000000000000000000, 0.000000000000000000, 0.000000000000000000 ) ) ;
#21093 = AXIS2_PLACEMENT_3D ( 'NONE', #2218, #15818, #27268 ) ;
#21094 = COLOUR_RGB ( '', 0.72549020, 0.75294118, 0.79215686) ;
#21095 = CARTESIAN_POINT ( 'NONE',  ( -5.999999999999963585, -1.487416814333745711E-14, -138.8363248654052597 ) ) ;
#21096 = CARTESIAN_POINT ( 'NONE',  ( -4.999999999999913847, -65.50000000000001421, 7.500000000000007105 ) ) ;
#21097 = ORIENTED_EDGE ( 'NONE', *, *, #12685, .F. ) ;
#21098 = AXIS2_PLACEMENT_3D ( 'NONE', #19671, #7976, #5663 ) ;
#21099 = CARTESIAN_POINT ( 'NONE',  ( -4.763139720814407951, 2.749999999999946709, -56.75000000000002132 ) ) ;
#21100 = EDGE_CURVE ( 'NONE', #27213, #20652, #23228, .T. ) ;
#21101 = EDGE_CURVE ( 'NONE', #8441, #9719, #18113, .T. ) ;
#21102 = ORIENTED_EDGE ( 'NONE', *, *, #16411, .F. ) ;
#21103 = CARTESIAN_POINT ( 'NONE',  ( 105.1249999999999005, 1.767766952966265404, 1.767766952966431937 ) ) ;
#21104 = CARTESIAN_POINT ( 'NONE',  ( 137.1562500000000284, -6.000000000000005329, 2.485281374238556218 ) ) ;
#21105 = CARTESIAN_POINT ( 'NONE',  ( 2.775557561562891351E-14, -6.250000000000061284, -106.8169872981078470 ) ) ;
#21106 = LINE ( 'NONE', #21404, #21457 ) ;
#21107 = CARTESIAN_POINT ( 'NONE',  ( 134.8125000000000284, 4.242640687119298093, -4.242640687119298093 ) ) ;
#21108 = CARTESIAN_POINT ( 'NONE',  ( 119.3749999999998863, -1.767766952966209892, 1.767766952966542959 ) ) ;
#21109 = AXIS2_PLACEMENT_3D ( 'NONE', #27124, #29596, #29740 ) ;
#21110 = CARTESIAN_POINT ( 'NONE',  ( -2.775557561562891351E-14, -5.500000000000115463, -134.2500000000000284 ) ) ;
#21111 = ORIENTED_EDGE ( 'NONE', *, *, #4997, .F. ) ;
#21112 = CARTESIAN_POINT ( 'NONE',  ( -3.175426480542816510, 5.499999999999865885, -68.87500000000002842 ) ) ;
#21113 = CARTESIAN_POINT ( 'NONE',  ( 5.196152422706629359, -2.999999999999988898, -81.21132486540521711 ) ) ;
#21114 = LINE ( 'NONE', #28739, #26915 ) ;
#21115 = CARTESIAN_POINT ( 'NONE',  ( 3.608439182435180470, -6.249999999999997335, -83.55801270189222407 ) ) ;
#21116 = EDGE_CURVE ( 'NONE', #13036, #21338, #758, .T. ) ;
#21117 = CARTESIAN_POINT ( 'NONE',  ( 107.8122167782374135, 0.7662911109078888172, 1.849990392679712103 ) ) ;
#21118 = CARTESIAN_POINT ( 'NONE',  ( 11.96132486540524198, 1.110223024625156540E-13, 2.499999999999835687 ) ) ;
#21119 =( BOUNDED_CURVE ( )  B_SPLINE_CURVE ( 2, ( #24273, #10476, #19543, #10020, #24426, #19398, #19830, #7840, #10635 ),
 .UNSPECIFIED., .F., .T. ) 
 B_SPLINE_CURVE_WITH_KNOTS ( ( 3, 2, 2, 2, 3 ),
 ( 0.2625000000000007327, 0.2687500000000004885, 0.2750000000000002998, 0.2812500000000000555, 0.2874999999999998113 ),
 .UNSPECIFIED. ) 
 CURVE ( )  GEOMETRIC_REPRESENTATION_ITEM ( )  RATIONAL_B_SPLINE_CURVE ( ( 0.9999999999999912292, 0.9238795325112955092, 1.000000000000000000, 0.9238795325112867385, 1.000000000000000000, 0.9238795325112867385, 1.000000000000000000, 0.9238795325112887369, 0.9999999999999980016 ) ) 
 REPRESENTATION_ITEM ( '' )  );
#21120 = CARTESIAN_POINT ( 'NONE',  ( 119.4377832217620607, 1.849990392679591977, 0.7662911109080692285 ) ) ;
#21121 = CARTESIAN_POINT ( 'NONE',  ( 0.000000000000000000, 5.499999999999991118, -145.5000000000000284 ) ) ;
#21122 = CARTESIAN_POINT ( 'NONE',  ( 139.6069567752852265, -8.946933505375708862, -7.999999993627826989 ) ) ;
#21123 = CARTESIAN_POINT ( 'NONE',  ( 4.763139720814407951, -2.749999999999988454, -138.5000000000000000 ) ) ;
#21124 = CARTESIAN_POINT ( 'NONE',  ( 7.216878364870455975, -6.409875621278545621E-14, -164.3080127018922951 ) ) ;
#21125 = DIRECTION ( 'NONE',  ( 1.000000000000000000, -6.938893903907221278E-15, 0.000000000000000000 ) ) ;
#21126 = CIRCLE ( 'NONE', #20139, 5.500000000000000000 ) ;
#21127 = CARTESIAN_POINT ( 'NONE',  ( -4.763139720814407951, -2.750000000000016431, -79.00000000000001421 ) ) ;
#21128 = ADVANCED_FACE ( 'NONE', ( #27255 ), #11021, .T. ) ;
#21129 = CARTESIAN_POINT ( 'NONE',  ( -3.175426480542816510, 5.499999999999865885, -67.37500000000002842 ) ) ;
#21130 = ADVANCED_FACE ( 'NONE', ( #6226 ), #15646, .T. ) ;
#21131 = CARTESIAN_POINT ( 'NONE',  ( 6.000000000000000888, -3.330669073875464691E-16, -7.560779664488942560E-35 ) ) ;
#21132 = CARTESIAN_POINT ( 'NONE',  ( 144.1086002691896226, -2.071067811865468400, -4.999999999999989342 ) ) ;
#21133 = CARTESIAN_POINT ( 'NONE',  ( 5.196152422706629359, -2.999999999999988898, -87.78867513459486815 ) ) ;
#21134 = CARTESIAN_POINT ( 'NONE',  ( 0.000000000000000000, -5.999999999999991118, -144.4613248654052029 ) ) ;
#21135 = CARTESIAN_POINT ( 'NONE',  ( 157.7812500000000284, 2.485281374238585972, 6.000000000000005329 ) ) ;
#21136 = CARTESIAN_POINT ( 'NONE',  ( 18.06250000000005684, 2.000000000000151879, 0.8284271247461152399 ) ) ;
#21137 = CARTESIAN_POINT ( 'NONE',  ( 5.196152422706629359, -2.999999999999988898, -49.71132486540519579 ) ) ;
#21138 = DIRECTION ( 'NONE',  ( 0.000000000000000000, 1.000000000000000000, 0.000000000000000000 ) ) ;
#21139 = CARTESIAN_POINT ( 'NONE',  ( 118.1872167782374845, -1.849990392679472073, -0.7662911109076485650 ) ) ;
#21140 = CARTESIAN_POINT ( 'NONE',  ( 6.000000000000000888, 1.743066579297358182E-13, -97.58632486540524553 ) ) ;
#21141 = ORIENTED_EDGE ( 'NONE', *, *, #15461, .T. ) ;
#21142 = CARTESIAN_POINT ( 'NONE',  ( 150.4687500000000284, -2.485281374238585972, 6.000000000000005329 ) ) ;
#21143 = CARTESIAN_POINT ( 'NONE',  ( 115.2502832217623592, 1.308140751793696044, -1.308140751793529510 ) ) ;
#21144 = CARTESIAN_POINT ( 'NONE',  ( -3.464101615137725076, 5.999999999999979572, -179.5863248654052029 ) ) ;
#21145 = ORIENTED_EDGE ( 'NONE', *, *, #8147, .T. ) ;
#21146 = EDGE_LOOP ( 'NONE', ( #28070, #25985, #412, #23857 ) ) ;
#21147 = CARTESIAN_POINT ( 'NONE',  ( 19.37500000000019895, -1.414213562372979016, 1.414213562373034527 ) ) ;
#21148 = ORIENTED_EDGE ( 'NONE', *, *, #29977, .F. ) ;
#21149 = CARTESIAN_POINT ( 'NONE',  ( 4.763139720814407951, -2.749999999999988454, -86.00000000000001421 ) ) ;
#21150 = CARTESIAN_POINT ( 'NONE',  ( -5.412658773652684552, -3.125000000000099920, -110.9330127018922667 ) ) ;
#21151 = ORIENTED_EDGE ( 'NONE', *, *, #11446, .T. ) ;
#21152 = PRESENTATION_LAYER_ASSIGNMENT (  '', '', ( #17238 ) ) ;
#21153 = CARTESIAN_POINT ( 'NONE',  ( 0.4044047236351530628, 10.99999999999998224, -31.00000000000002842 ) ) ;
#21154 = CARTESIAN_POINT ( 'NONE',  ( 154.4851497308104058, -3.535533905932725318, 3.535533905932725318 ) ) ;
#21155 = CARTESIAN_POINT ( 'NONE',  ( 6.350852961086080661, -9.614813431917819062E-14, -165.3750000000000284 ) ) ;
#21156 = EDGE_CURVE ( 'NONE', #14326, #18615, #17127, .T. ) ;
#21157 = CARTESIAN_POINT ( 'NONE',  ( 2.775557561562891351E-14, -6.250000000000061284, -47.68301270189223828 ) ) ;
#21158 = CARTESIAN_POINT ( 'NONE',  ( 5.196152422706629359, 3.000000000000002665, -47.03867513459481131 ) ) ;
#21159 =( BOUNDED_CURVE ( )  B_SPLINE_CURVE ( 2, ( #17625, #26947, #13030, #22368, #10718, #7297, #11795, #11329, #30180 ),
 .UNSPECIFIED., .F., .T. ) 
 B_SPLINE_CURVE_WITH_KNOTS ( ( 3, 2, 2, 2, 3 ),
 ( 0.5625000000000009992, 0.5687500000000007550, 0.5750000000000005107, 0.5812500000000003775, 0.5875000000000001332 ),
 .UNSPECIFIED. ) 
 CURVE ( )  GEOMETRIC_REPRESENTATION_ITEM ( )  RATIONAL_B_SPLINE_CURVE ( ( 0.9999999999999877875, 0.9238795325112989509, 1.000000000000000000, 0.9238795325112867385, 1.000000000000000000, 0.9238795325112867385, 1.000000000000000000, 0.9238795325112854062, 1.000000000000001332 ) ) 
 REPRESENTATION_ITEM ( '' )  );
#21160 = VECTOR ( 'NONE', #4172, 1000.000000000000000 ) ;
#21161 = CARTESIAN_POINT ( 'NONE',  ( -4.763139720814407951, -2.750000000000016431, -172.0000000000000284 ) ) ;
#21162 = DIRECTION ( 'NONE',  ( 0.000000000000000000, 8.673617379884043361E-16, 1.000000000000000000 ) ) ;
#21163 = CARTESIAN_POINT ( 'NONE',  ( -3.175426480542816510, 5.499999999999865885, -151.3749999999999716 ) ) ;
#21164 = CARTESIAN_POINT ( 'NONE',  ( 112.6874999999997584, -1.035533905932659149, -2.499999999999603872 ) ) ;
#21165 = CARTESIAN_POINT ( 'NONE',  ( -6.350852961085760029, -1.281975124255709124E-13, -98.62500000000004263 ) ) ;
#21166 = CARTESIAN_POINT ( 'NONE',  ( -5.196152422706601826, 2.999999999999975131, -59.46132486540523132 ) ) ;
#21167 = EDGE_CURVE ( 'NONE', #26645, #4859, #16410, .T. ) ;
#21168 = CARTESIAN_POINT ( 'NONE',  ( -6.350852961085760029, -1.281975124255709124E-13, -88.12500000000000000 ) ) ;
#21169 = CARTESIAN_POINT ( 'NONE',  ( 162.0148502691896510, -3.535533905932725318, -3.535533905932725318 ) ) ;
#21170 = CARTESIAN_POINT ( 'NONE',  ( -0.07584961804942320918, -14.87383459521561591, 8.134942876244384280 ) ) ;
#21171 = VERTEX_POINT ( 'NONE', #2090 ) ;
#21172 = CARTESIAN_POINT ( 'NONE',  ( 10.25000000000012079, -1.873492889144845464, -1.873492889144956486 ) ) ;
#21173 = CARTESIAN_POINT ( 'NONE',  ( 112.6874999999997584, -1.035533905932659149, -2.499999999999603872 ) ) ;
#21174 = DIRECTION ( 'NONE',  ( -7.147005652999508048E-36, 5.642372883946980038E-36, 1.000000000000000000 ) ) ;
#21175 = CIRCLE ( 'NONE', #14340, 0.9999999999999995559 ) ;
#21176 = CARTESIAN_POINT ( 'NONE',  ( 105.8127832217621176, -1.849990392679501827, 0.7662911109077686911 ) ) ;
#21177 = CYLINDRICAL_SURFACE ( 'NONE', #12544, 2.000000000000012879 ) ;
#21178 = EDGE_LOOP ( 'NONE', ( #25791, #15896, #1962, #3920 ) ) ;
#21179 = CARTESIAN_POINT ( 'NONE',  ( 9.687499999999998224, -0.8284271247461152399, -1.999999999999971800 ) ) ;
#21180 = LINE ( 'NONE', #7477, #24094 ) ;
#21181 =( GEOMETRIC_REPRESENTATION_CONTEXT ( 3 ) GLOBAL_UNCERTAINTY_ASSIGNED_CONTEXT ( ( #23785 ) ) GLOBAL_UNIT_ASSIGNED_CONTEXT ( ( #23670, #2607, #26396 ) ) REPRESENTATION_CONTEXT ( 'NONE', 'WORKASPACE' ) );
#21182 = ORIENTED_EDGE ( 'NONE', *, *, #12516, .F. ) ;
#21183 = DIRECTION ( 'NONE',  ( -7.147005652999508048E-36, 5.642372883946980038E-36, 1.000000000000000000 ) ) ;
#21184 = ORIENTED_EDGE ( 'NONE', *, *, #4064, .T. ) ;
#21185 = CARTESIAN_POINT ( 'NONE',  ( 150.9375000000000284, -4.242640687119298093, -4.242640687119298093 ) ) ;
#21186 = ORIENTED_EDGE ( 'NONE', *, *, #9633, .T. ) ;
#21187 = CARTESIAN_POINT ( 'NONE',  ( 6.350852961086080661, -9.614813431917819062E-14, -112.8750000000000568 ) ) ;
#21188 = CARTESIAN_POINT ( 'NONE',  ( 22.25000000000004619, 1.873492889145123019, -1.873492889144956486 ) ) ;
#21189 = CARTESIAN_POINT ( 'NONE',  ( -3.608439182435052128, -6.250000000000110134, -134.8080127018922667 ) ) ;
#21190 = ORIENTED_EDGE ( 'NONE', *, *, #27158, .F. ) ;
#21191 = CYLINDRICAL_SURFACE ( 'NONE', #939, 6.000000000000000888 ) ;
#21192 = CARTESIAN_POINT ( 'NONE',  ( 2.775557561562891351E-14, 6.250000000000033751, -167.5669872981078186 ) ) ;
#21193 = CARTESIAN_POINT ( 'NONE',  ( 110.2499999999998010, -5.551115123125782702E-14, 2.500000000000168754 ) ) ;
#21194 =( LENGTH_UNIT ( ) NAMED_UNIT ( * ) SI_UNIT ( .MILLI., .METRE. ) );
#21195 = TOROIDAL_SURFACE ( 'NONE', #6945, 10.49999999999999645, 0.5000000000000000000 ) ;
#21196 = ADVANCED_FACE ( 'NONE', ( #25733 ), #14112, .T. ) ;
#21197 = ORIENTED_EDGE ( 'NONE', *, *, #2815, .F. ) ;
#21198 = CARTESIAN_POINT ( 'NONE',  ( -0.07587193451662191390, -14.87436656268081414, -8.134582247911094299 ) ) ;
#21199 = ADVANCED_FACE ( 'NONE', ( #30185 ), #23348, .T. ) ;
#21200 = CARTESIAN_POINT ( 'NONE',  ( 4.501142602643242618, 3.771550028933623011, -180.0000000000000853 ) ) ;
#21201 = CARTESIAN_POINT ( 'NONE',  ( 0.000000000000000000, 5.999999999999977796, -136.7886751345947971 ) ) ;
#21202 = CARTESIAN_POINT ( 'NONE',  ( -2.775557561562891351E-14, -5.500000000000115463, -179.2500000000000284 ) ) ;
#21203 = CARTESIAN_POINT ( 'NONE',  ( 109.8752832217622739, -1.849990392679468076, 1.110223024625156540E-13 ) ) ;
#21204 = CARTESIAN_POINT ( 'NONE',  ( -3.608439182435052128, -6.250000000000110134, -176.8080127018922099 ) ) ;
#21205 = CARTESIAN_POINT ( 'NONE',  ( -0.9018315097318220230, -9.098168490268067288, -4.000092554054210048 ) ) ;
#21206 = CARTESIAN_POINT ( 'NONE',  ( 6.000000000000000888, -3.330669073875464691E-16, -7.560779664488942560E-35 ) ) ;
#21207 = CARTESIAN_POINT ( 'NONE',  ( 161.0000000000000568, -11.64607081028603552, -2.895853930524592279 ) ) ;
#21208 = CARTESIAN_POINT ( 'NONE',  ( 4.763139720814407951, -2.749999999999988454, -111.5000000000000426 ) ) ;
#21209 = CARTESIAN_POINT ( 'NONE',  ( 5.196152422706629359, 3.000000000000002665, -166.4613248654052029 ) ) ;
#21210 = ORIENTED_EDGE ( 'NONE', *, *, #8019, .F. ) ;
#21211 = CARTESIAN_POINT ( 'NONE',  ( 21.62500000000017053, 2.649519052838555933, -5.551115123125782702E-14 ) ) ;
#21212 = CARTESIAN_POINT ( 'NONE',  ( -0.004414515218767962011, -15.41919126527335315, 6.290392408496218835 ) ) ;
#21213 = CARTESIAN_POINT ( 'NONE',  ( 0.000000000000000000, -5.999999999999991118, -55.96132486540522422 ) ) ;
#21214 = CARTESIAN_POINT ( 'NONE',  ( 110.2886751345946834, 2.000000000000085265, 1.110223024625156540E-13 ) ) ;
#21215 = ORIENTED_EDGE ( 'NONE', *, *, #8554, .F. ) ;
#21216 = LINE ( 'NONE', #12025, #7454 ) ;
#21217 = CARTESIAN_POINT ( 'NONE',  ( 139.5000000000000000, -8.798545334315205579, 8.160000000000000142 ) ) ;
#21218 = AXIS2_PLACEMENT_3D ( 'NONE', #4980, #24179, #28768 ) ;
#21219 = CARTESIAN_POINT ( 'NONE',  ( 22.33632486540521001, -1.767766952966320915, -1.767766952966542959 ) ) ;
#21220 = CARTESIAN_POINT ( 'NONE',  ( -0.5000000000000004441, -10.00000000000000888, 5.000000000000004441 ) ) ;
#21221 = DIRECTION ( 'NONE',  ( -7.147005652999508048E-36, 5.642372883946980038E-36, 1.000000000000000000 ) ) ;
#21222 = VERTEX_POINT ( 'NONE', #29873 ) ;
#21223 = ORIENTED_EDGE ( 'NONE', *, *, #2389, .T. ) ;
#21224 = CARTESIAN_POINT ( 'NONE',  ( -4.999999999999990230, -24.99999999999999289, 8.000000000000007105 ) ) ;
#21225 = CARTESIAN_POINT ( 'NONE',  ( 133.1250000000000284, 0.000000000000000000, -6.000000000000005329 ) ) ;
#21226 = CARTESIAN_POINT ( 'NONE',  ( 7.216878364870455975, -6.409875621278545621E-14, -139.4419872981078186 ) ) ;
#21227 = LINE ( 'NONE', #11733, #27292 ) ;
#21228 = CARTESIAN_POINT ( 'NONE',  ( 3.464101615137757051, -5.999999999999979572, -93.33632486540517448 ) ) ;
#21229 = DIRECTION ( 'NONE',  ( 0.000000000000000000, 0.000000000000000000, 1.000000000000000000 ) ) ;
#21230 = CARTESIAN_POINT ( 'NONE',  ( 6.000000000000000888, 5.577813053751546416E-15, -165.0863248654052313 ) ) ;
#21231 = EDGE_CURVE ( 'NONE', #3131, #22297, #20255, .T. ) ;
#21232 = DIRECTION ( 'NONE',  ( 0.000000000000000000, 0.000000000000000000, -1.000000000000000000 ) ) ;
#21233 = CARTESIAN_POINT ( 'NONE',  ( 145.8601497308104058, -3.535533905932725318, -3.535533905932725318 ) ) ;
#21234 = CARTESIAN_POINT ( 'NONE',  ( 12.03867513459491789, 1.665334536937734811E-13, -2.500000000000057732 ) ) ;
#21235 = CARTESIAN_POINT ( 'NONE',  ( 12.97617513459487171, -1.035533905932629173, -2.500000000000084821 ) ) ;
#21236 =( LENGTH_UNIT ( ) NAMED_UNIT ( * ) SI_UNIT ( .MILLI., .METRE. ) );
#21237 = CARTESIAN_POINT ( 'NONE',  ( 24.79215710450393928, -1.034327703891616990, -1.956437050582624071 ) ) ;
#21238 = SURFACE_STYLE_USAGE ( .BOTH. , #2485 ) ;
#21239 = CARTESIAN_POINT ( 'NONE',  ( 110.4999999999999432, -2.499999999999891198, 3.330669073875469621E-13 ) ) ;
#21240 = FACE_OUTER_BOUND ( 'NONE', #30298, .T. ) ;
#21241 = ORIENTED_EDGE ( 'NONE', *, *, #845, .T. ) ;
#21242 = CARTESIAN_POINT ( 'NONE',  ( -4.763139720814407951, 2.749999999999946709, -58.25000000000002132 ) ) ;
#21243 = CARTESIAN_POINT ( 'NONE',  ( -5.999999999999963585, 1.780251999655701777E-13, -62.33632486540522422 ) ) ;
#21244 =( BOUNDED_CURVE ( )  B_SPLINE_CURVE ( 2, ( #14210, #2632, #25838, #9718, #30292, #11909, #9254, #14066, #9564 ),
 .UNSPECIFIED., .F., .T. ) 
 B_SPLINE_CURVE_WITH_KNOTS ( ( 3, 2, 2, 2, 3 ),
 ( 0.2416666666666666685, 0.2425925925925925819, 0.2444444444444444364, 0.2462962962962962910, 0.2472222222222222043 ),
 .UNSPECIFIED. ) 
 CURVE ( )  GEOMETRIC_REPRESENTATION_ITEM ( )  RATIONAL_B_SPLINE_CURVE ( ( 0.9330127018922194093, 0.9330127018922204085, 1.000000000000000000, 0.8660254037844388186, 1.000000000000000000, 0.8660254037844388186, 1.000000000000000000, 0.9330127018922205195, 0.9330127018922196314 ) ) 
 REPRESENTATION_ITEM ( '' )  );
#21245 = CARTESIAN_POINT ( 'NONE',  ( 3.464101615137757051, -5.999999999999979572, -151.8363248654051745 ) ) ;
#21246 = ORIENTED_EDGE ( 'NONE', *, *, #15537, .F. ) ;
#21247 = CARTESIAN_POINT ( 'NONE',  ( 117.9372167782374419, -0.7662911109077987781, 1.849990392679591977 ) ) ;
#21248 = CARTESIAN_POINT ( 'NONE',  ( 139.8750000000000284, 0.000000000000000000, 6.000000000000005329 ) ) ;
#21249 = CARTESIAN_POINT ( 'NONE',  ( -3.608439182435115633, 6.249999999999965361, -99.94198729810783277 ) ) ;
#21250 = FACE_OUTER_BOUND ( 'NONE', #6415, .T. ) ;
#21251 =( BOUNDED_CURVE ( )  B_SPLINE_CURVE ( 2, ( #15412, #1696, #20298, #29644, #24738, #22294, #3836, #25031, #8611 ),
 .UNSPECIFIED., .F., .T. ) 
 B_SPLINE_CURVE_WITH_KNOTS ( ( 3, 2, 2, 2, 3 ),
 ( 0.03749999999999957534, 0.04374999999999980987, 0.05000000000000005829, 0.05625000000000029282, 0.06250000000000052736 ),
 .UNSPECIFIED. ) 
 CURVE ( )  GEOMETRIC_REPRESENTATION_ITEM ( )  RATIONAL_B_SPLINE_CURVE ( ( 1.000000000000005107, 0.9238795325112816315, 1.000000000000000000, 0.9238795325112867385, 1.000000000000000000, 0.9238795325112867385, 1.000000000000000000, 0.9238795325112802992, 1.000000000000006439 ) ) 
 REPRESENTATION_ITEM ( '' )  );
#21252 = CARTESIAN_POINT ( 'NONE',  ( 134.4375000000000568, -4.242640687119298093, -4.242640687119298093 ) ) ;
#21253 = CARTESIAN_POINT ( 'NONE',  ( 119.3124999999998295, -1.035533905932689347, 2.500000000000265121 ) ) ;
#21254 = EDGE_CURVE ( 'NONE', #19300, #8188, #16506, .T. ) ;
#21255 = CARTESIAN_POINT ( 'NONE',  ( -3.175426480542816510, -5.500000000000057732, -138.8750000000000568 ) ) ;
#21256 = CIRCLE ( 'NONE', #20782, 9.999999999999996447 ) ;
#21257 = ORIENTED_EDGE ( 'NONE', *, *, #17666, .F. ) ;
#21258 = CARTESIAN_POINT ( 'NONE',  ( 3.464101615137852974, 5.999999999999884537, -163.3363248654052313 ) ) ;
#21259 = CARTESIAN_POINT ( 'NONE',  ( 4.763139720814407951, 2.750000000000002665, -66.25000000000002842 ) ) ;
#21260 = DIRECTION ( 'NONE',  ( 0.000000000000000000, 0.000000000000000000, 1.000000000000000000 ) ) ;
#21261 = CARTESIAN_POINT ( 'NONE',  ( -5.412658773652739619, 3.124999999999975131, -79.68301270189226670 ) ) ;
#21262 = AXIS2_PLACEMENT_3D ( 'NONE', #4356, #22970, #1908 ) ;
#21263 = EDGE_CURVE ( 'NONE', #28771, #26763, #8101, .T. ) ;
#21264 = CARTESIAN_POINT ( 'NONE',  ( -5.999999999999963585, -1.487416814333745711E-14, -139.4136751345948255 ) ) ;
#21265 = CARTESIAN_POINT ( 'NONE',  ( 104.6872167782374277, 1.849990392679532247, 0.7662911109080692285 ) ) ;
#21266 = CARTESIAN_POINT ( 'NONE',  ( 141.0000000000000284, -12.00000000000001066, -4.000000000000003553 ) ) ;
#21267 = CARTESIAN_POINT ( 'NONE',  ( 119.7502832217622455, -1.308140751793501755, 1.308140751793751555 ) ) ;
#21268 = CARTESIAN_POINT ( 'NONE',  ( -3.175426480542816066, 5.499999999999865885, -145.3750000000000000 ) ) ;
#21269 = CARTESIAN_POINT ( 'NONE',  ( -5.412658773652739619, 3.124999999999975131, -154.6830127018922099 ) ) ;
#21270 = CARTESIAN_POINT ( 'NONE',  ( 0.000000000000000000, 0.000000000000000000, 0.000000000000000000 ) ) ;
#21271 = CARTESIAN_POINT ( 'NONE',  ( -4.999999999999886313, -10.50000000000000888, 7.500000000000007105 ) ) ;
#21272 = CARTESIAN_POINT ( 'NONE',  ( -4.763139720814407951, 2.749999999999946709, -79.25000000000004263 ) ) ;
#21273 = CARTESIAN_POINT ( 'NONE',  ( -5.196152422706601826, 2.999999999999975131, -85.53867513459483973 ) ) ;
#21274 = LINE ( 'NONE', #23733, #8744 ) ;
#21275 = CARTESIAN_POINT ( 'NONE',  ( 6.350852961086080661, -9.614813431917819062E-14, -64.87500000000002842 ) ) ;
#21276 = FACE_OUTER_BOUND ( 'NONE', #24862, .T. ) ;
#21277 = CARTESIAN_POINT ( 'NONE',  ( 143.6398502691896510, -3.535533905932752852, 3.535533905932725318 ) ) ;
#21278 = CARTESIAN_POINT ( 'NONE',  ( 1.000000000000000888, -16.31586670994438037, 6.338163299696072173 ) ) ;
#21279 = VECTOR ( 'NONE', #5943, 1000.000000000000000 ) ;
#21280 = CARTESIAN_POINT ( 'NONE',  ( 160.4062500000000284, 6.000000000000005329, -2.485281374238556218 ) ) ;
#21281 = CYLINDRICAL_SURFACE ( 'NONE', #17309, 4.000000000000010658 ) ;
#21282 = CARTESIAN_POINT ( 'NONE',  ( 16.43750000000008527, -1.999999999999851674, 0.8284271247461753029 ) ) ;
#21283 = LINE ( 'NONE', #4533, #25349 ) ;
#21284 = CARTESIAN_POINT ( 'NONE',  ( 116.7497167782375413, 1.308140751793585022, 1.308140751793751555 ) ) ;
#21285 = CARTESIAN_POINT ( 'NONE',  ( -3.464101615137757051, -5.999999999999979572, -145.1636751345948255 ) ) ;
#21286 = ORIENTED_EDGE ( 'NONE', *, *, #15779, .T. ) ;
#21287 = CARTESIAN_POINT ( 'NONE',  ( 147.2812500000000284, 2.485281374238585972, 6.000000000000005329 ) ) ;
#21288 = CARTESIAN_POINT ( 'NONE',  ( 119.0386751345946976, 5.551115123125782702E-14, -1.999999999999890754 ) ) ;
#21289 = CARTESIAN_POINT ( 'NONE',  ( 114.9377832217620750, -1.849990392679501827, -0.7662911109076485650 ) ) ;
#21290 = EDGE_CURVE ( 'NONE', #19006, #6411, #24350, .T. ) ;
#21291 = DIRECTION ( 'NONE',  ( -7.147005652999508048E-36, 5.642372883946980038E-36, 1.000000000000000000 ) ) ;
#21292 = CARTESIAN_POINT ( 'NONE',  ( 20.00000000000004619, 2.000000000000057288, -5.551115123125782702E-14 ) ) ;
#21293 = CARTESIAN_POINT ( 'NONE',  ( -3.608439182435052128, -6.250000000000110134, -151.9419872981077901 ) ) ;
#21294 = ORIENTED_EDGE ( 'NONE', *, *, #15951, .T. ) ;
#21295 = CARTESIAN_POINT ( 'NONE',  ( 4.763139720814407951, 2.750000000000002665, -88.75000000000000000 ) ) ;
#21296 = CARTESIAN_POINT ( 'NONE',  ( 16.06250000000017764, -1.097466725451439196, -2.649519052838478661 ) ) ;
#21297 = EDGE_CURVE ( 'NONE', #25911, #12140, #11614, .T. ) ;
#21298 = CARTESIAN_POINT ( 'NONE',  ( -5.412658773652739619, 3.124999999999975131, -102.1830127018922241 ) ) ;
#21299 = VERTEX_POINT ( 'NONE', #16110 ) ;
#21300 = CARTESIAN_POINT ( 'NONE',  ( 154.1101497308104058, 3.535533905932725318, 3.535533905932725318 ) ) ;
#21301 = CARTESIAN_POINT ( 'NONE',  ( 5.676437577760689912, -9.422458200488941671, -23.04620489006167716 ) ) ;
#21302 =( NAMED_UNIT ( * ) PLANE_ANGLE_UNIT ( ) SI_UNIT ( $, .RADIAN. ) );
#21303 = CYLINDRICAL_SURFACE ( 'NONE', #7830, 6.000000000000000888 ) ;
#21304 =( LENGTH_UNIT ( ) NAMED_UNIT ( * ) SI_UNIT ( .MILLI., .METRE. ) );
#21305 = CARTESIAN_POINT ( 'NONE',  ( 0.000000000000000000, 5.499999999999991118, -174.0000000000000568 ) ) ;
#21306 = CARTESIAN_POINT ( 'NONE',  ( 5.999999999999949374, 1.607695154586804565, -162.0193375672974128 ) ) ;
#21307 = CARTESIAN_POINT ( 'NONE',  ( 0.000000000000000000, 5.499999999999991118, -153.0000000000000284 ) ) ;
#21308 = CARTESIAN_POINT ( 'NONE',  ( 112.3749999999999289, -1.767766952966320915, 1.767766952966431937 ) ) ;
#21309 = CARTESIAN_POINT ( 'NONE',  ( 4.763139720814407951, 2.750000000000002665, -99.25000000000000000 ) ) ;
#21310 =( NAMED_UNIT ( * ) PLANE_ANGLE_UNIT ( ) SI_UNIT ( $, .RADIAN. ) );
#21311 = CARTESIAN_POINT ( 'NONE',  ( 115.4136751345946976, 1.414213562373090038, 1.414213562373034527 ) ) ;
#21313 = CARTESIAN_POINT ( 'NONE',  ( -4.763139720814407951, 2.749999999999946709, -89.75000000000000000 ) ) ;
#21312 = CARTESIAN_POINT ( 'NONE',  ( 6.350852961086080661, -9.614813431917819062E-14, -156.3750000000000000 ) ) ;
#21314 = CARTESIAN_POINT ( 'NONE',  ( 157.7961002691896510, 2.071067811865468400, -4.999999999999989342 ) ) ;
#21315 = LINE ( 'NONE', #258, #8657 ) ;
#21316 = ORIENTED_EDGE ( 'NONE', *, *, #4417, .T. ) ;
#21317 = CARTESIAN_POINT ( 'NONE',  ( 24.81250000000011724, 0.8284271247463557142, -2.000000000000091926 ) ) ;
#21318 = UNCERTAINTY_MEASURE_WITH_UNIT (LENGTH_MEASURE( 1.000000000000000082E-05 ), #22286, 'distance_accuracy_value', 'NONE');
#21319 = CARTESIAN_POINT ( 'NONE',  ( 111.8749999999998437, 1.767766952966348670, -1.767766952966209892 ) ) ;
#21320 = CARTESIAN_POINT ( 'NONE',  ( 160.0000000000000284, -12.64911064067353408, 3.000000000000002665 ) ) ;
#21321 = CARTESIAN_POINT ( 'NONE',  ( 104.9377832217622171, -1.849990392679411677, -0.7662911109076485650 ) ) ;
#21322 = CARTESIAN_POINT ( 'NONE',  ( 20.28867513459483973, 2.500000000000002220, 0.000000000000000000 ) ) ;
#21323 = ORIENTED_EDGE ( 'NONE', *, *, #2899, .F. ) ;
#21324 = CARTESIAN_POINT ( 'NONE',  ( 6.000000000000000888, -1.859271017917181981E-14, -131.1636751345948539 ) ) ;
#21325 = CARTESIAN_POINT ( 'NONE',  ( 0.000000000000000000, -10.00000000000000888, 7.500000000000007105 ) ) ;
#21326 = CARTESIAN_POINT ( 'NONE',  ( 106.4372167782374419, 0.7662911109078588412, -1.849990392679231599 ) ) ;
#21327 = EDGE_CURVE ( 'NONE', #19218, #30081, #20680, .T. ) ;
#21328 = VECTOR ( 'NONE', #793, 1000.000000000000000 ) ;
#21329 = VERTEX_POINT ( 'NONE', #27709 ) ;
#21330 = CARTESIAN_POINT ( 'NONE',  ( 125.0000000000000568, -55.00000000000000711, -7.500000000000007105 ) ) ;
#21331 = CARTESIAN_POINT ( 'NONE',  ( 151.2187500000000284, 2.485281374238555774, -6.000000000000005329 ) ) ;
#21332 = CARTESIAN_POINT ( 'NONE',  ( -4.763139720814407951, -2.750000000000016431, -116.5000000000000426 ) ) ;
#21333 = CARTESIAN_POINT ( 'NONE',  ( 19.62500000000011369, 1.665334536937734811E-13, 2.649519052838278377 ) ) ;
#21334 = ADVANCED_FACE ( 'NONE', ( #2246 ), #6690, .F. ) ;
#21335 =( BOUNDED_CURVE ( )  B_SPLINE_CURVE ( 2, ( #28939, #5143, #17315, #24046, #701, #26631, #19458, #16727, #26192 ),
 .UNSPECIFIED., .F., .T. ) 
 B_SPLINE_CURVE_WITH_KNOTS ( ( 3, 2, 2, 2, 3 ),
 ( 0.1027777777777777457, 0.1037037037037037424, 0.1055555555555555136, 0.1074074074074073959, 0.1083333333333333925 ),
 .UNSPECIFIED. ) 
 CURVE ( )  GEOMETRIC_REPRESENTATION_ITEM ( )  RATIONAL_B_SPLINE_CURVE ( ( 0.9330127018922194093, 0.9330127018922154125, 1.000000000000000000, 0.8660254037844388186, 1.000000000000000000, 0.8660254037844388186, 1.000000000000000000, 0.9330127018922154125, 0.9330127018922194093 ) ) 
 REPRESENTATION_ITEM ( '' )  );
#21336 = CARTESIAN_POINT ( 'NONE',  ( 5.412658773652712085, -3.125000000000086153, -126.9330127018922809 ) ) ;
#21337 = UNCERTAINTY_MEASURE_WITH_UNIT (LENGTH_MEASURE( 1.000000000000000082E-05 ), #21194, 'distance_accuracy_value', 'NONE');
#21338 = VERTEX_POINT ( 'NONE', #10065 ) ;
#21339 = CARTESIAN_POINT ( 'NONE',  ( 2.775557561562891351E-14, -6.250000000000061284, -172.8169872981077901 ) ) ;
#21340 = CARTESIAN_POINT ( 'NONE',  ( 107.3124999999996589, -1.035533905932598975, 2.500000000000205169 ) ) ;
#21341 = CARTESIAN_POINT ( 'NONE',  ( 134.5163997308104342, 4.999999999999989342, 2.071067811865468400 ) ) ;
#21342 = ORIENTED_EDGE ( 'NONE', *, *, #22189, .T. ) ;
#21343 = CARTESIAN_POINT ( 'NONE',  ( 153.5699251345948539, 2.278174593052229469, 5.499999999999796607 ) ) ;
#21344 = PRESENTATION_STYLE_ASSIGNMENT (( #5477 ) ) ;
#21345 = CARTESIAN_POINT ( 'NONE',  ( -4.763139720814407951, -2.750000000000016431, -176.5000000000000000 ) ) ;
#21346 = CARTESIAN_POINT ( 'NONE',  ( 108.1877832217622881, 0.7662911109077388261, -1.849990392679291551 ) ) ;
#21347 = CARTESIAN_POINT ( 'NONE',  ( 3.608439182435180470, -6.249999999999997335, -173.5580127018922383 ) ) ;
#21348 = CARTESIAN_POINT ( 'NONE',  ( -5.999999999999963585, -1.487416814333745711E-14, -75.83632486540521711 ) ) ;
#21349 = CARTESIAN_POINT ( 'NONE',  ( 5.196152422706629359, -2.999999999999988898, -48.21132486540524553 ) ) ;
#21350 = CARTESIAN_POINT ( 'NONE',  ( 6.000000000000000888, -3.330669073875464691E-16, -7.560779664488942560E-35 ) ) ;
#21351 = UNCERTAINTY_MEASURE_WITH_UNIT (LENGTH_MEASURE( 1.000000000000000082E-05 ), #29969, 'distance_accuracy_value', 'NONE');
#21352 = CARTESIAN_POINT ( 'NONE',  ( -4.763139720814407951, -2.750000000000016431, -110.5000000000000426 ) ) ;
#21353 = AXIS2_PLACEMENT_3D ( 'NONE', #15259, #7852, #17263 ) ;
#21354 = CARTESIAN_POINT ( 'NONE',  ( 135.0000000000000284, -9.047800747817511535, -7.999999999998980371 ) ) ;
#21355 = CARTESIAN_POINT ( 'NONE',  ( 6.000000000000000888, 1.607695154586715303, -89.09668783648706381 ) ) ;
#21356 = EDGE_LOOP ( 'NONE', ( #27649, #6095, #6612, #30061 ) ) ;
#21357 = CARTESIAN_POINT ( 'NONE',  ( 18.31250000000011724, -1.097466725451439196, -2.649519052838419153 ) ) ;
#21358 = CARTESIAN_POINT ( 'NONE',  ( 8.673617379884035472E-16, -15.50000000000001421, 5.656854249492387687 ) ) ;
#21359 = CARTESIAN_POINT ( 'NONE',  ( -5.999999999999963585, 1.780251999655701777E-13, -111.8363248654052313 ) ) ;
#21360 = CARTESIAN_POINT ( 'NONE',  ( 5.999999999999949374, 1.607695154586804565, -132.0193375672974412 ) ) ;
#21361 = ORIENTED_EDGE ( 'NONE', *, *, #18932, .F. ) ;
#21362 = CARTESIAN_POINT ( 'NONE',  ( -6.350852961085760029, -1.281975124255709124E-13, -179.6249999999999716 ) ) ;
#21363 = B_SPLINE_CURVE_WITH_KNOTS ( 'NONE', 3,
 ( #26433, #5389, #21994, #6306, #1549, #24747, #3533, #10640, #27036, #3996, #6163, #13271, #25039, #24892, #13415, #6461 ),
 .UNSPECIFIED., .F., .F.,
 ( 4, 2, 2, 2, 2, 2, 2, 4 ),
 ( 0.000000000000000000, 0.001733696408318075163, 0.002600544612477113070, 0.003467392816636151627, 0.004334241020795190184, 0.005201089224954227874, 0.006067937429113266432, 0.006934785633272304989 ),
 .UNSPECIFIED. ) ;
#21364 = VECTOR ( 'NONE', #7473, 1000.000000000000000 ) ;
#21365 = EDGE_CURVE ( 'NONE', #22419, #15757, #3173, .T. ) ;
#21366 = CARTESIAN_POINT ( 'NONE',  ( -3.464101615137725076, 5.999999999999979572, -108.1636751345948397 ) ) ;
#21367 = CARTESIAN_POINT ( 'NONE',  ( -5.196152422706573404, -3.000000000000002665, -77.78867513459481131 ) ) ;
#21368 = ADVANCED_FACE ( 'NONE', ( #5274 ), #24026, .T. ) ;
#21369 = PRODUCT_DEFINITION ( 'UNKNOWN', '', #21764, #2654 ) ;
#21370 = FACE_OUTER_BOUND ( 'NONE', #1126, .T. ) ;
#21371 = EDGE_LOOP ( 'NONE', ( #11757, #18590, #7109, #30293 ) ) ;
#21372 = ORIENTED_EDGE ( 'NONE', *, *, #3884, .T. ) ;
#21373 = CARTESIAN_POINT ( 'NONE',  ( 106.0386751345947118, 0.000000000000000000, -2.000000000000001776 ) ) ;
#21374 = CARTESIAN_POINT ( 'NONE',  ( 136.6875000000000284, 4.242640687119269671, 4.242640687119298093 ) ) ;
#21375 = ORIENTED_EDGE ( 'NONE', *, *, #22466, .T. ) ;
#21376 = PRESENTATION_LAYER_ASSIGNMENT (  '', '', ( #6624 ) ) ;
#21377 = CARTESIAN_POINT ( 'NONE',  ( 3.608439182435180470, 6.249999999999982236, -137.6919872981078186 ) ) ;
#21378 = FILL_AREA_STYLE ('',( #18943 ) ) ;
#21379 = CARTESIAN_POINT ( 'NONE',  ( -5.999999999999964473, 9.063946212346262433E-15, -174.8363248654052313 ) ) ;
#21380 = CARTESIAN_POINT ( 'NONE',  ( -5.999999999999982236, -1.607695154586700426, -116.8466878364870638 ) ) ;
#21381 = CARTESIAN_POINT ( 'NONE',  ( 17.68750000000009592, -0.8284271247460552878, -1.999999999999971800 ) ) ;
#21382 = DIRECTION ( 'NONE',  ( 1.000000000000000000, 0.000000000000000000, -0.000000000000000000 ) ) ;
#21383 = CARTESIAN_POINT ( 'NONE',  ( 7.147005652999508048E-33, -5.642372883946980038E-33, -1183.000000000000000 ) ) ;
#21384 = CARTESIAN_POINT ( 'NONE',  ( -0.5000000000000004441, -10.00000000000000888, 5.000000000000004441 ) ) ;
#21385 = CARTESIAN_POINT ( 'NONE',  ( 139.3913997308104342, -2.071067811865468400, 4.999999999999989342 ) ) ;
#21386 = CARTESIAN_POINT ( 'NONE',  ( 22.53867513459501026, 1.110223024625156540E-13, 2.499999999999835687 ) ) ;
#21387 = CARTESIAN_POINT ( 'NONE',  ( 12.46132486540529882, 1.110223024625156540E-13, -2.500000000000057732 ) ) ;
#21388 = CARTESIAN_POINT ( 'NONE',  ( 23.03867513459492855, 2.220446049250313081E-13, -2.500000000000057732 ) ) ;
#21389 = STYLED_ITEM ( 'NONE', ( #20994 ), #21334 ) ;
#21390 = CARTESIAN_POINT ( 'NONE',  ( 6.000000000000000888, 1.743066579297358182E-13, -60.66367513459481842 ) ) ;
#21391 = DIRECTION ( 'NONE',  ( -8.326672684688675286E-17, -2.081668171172168821E-17, 1.000000000000000000 ) ) ;
#21392 = CARTESIAN_POINT ( 'NONE',  ( 106.3749999999999574, -1.767766952966320915, 1.767766952966431937 ) ) ;
#21393 =( BOUNDED_CURVE ( )  B_SPLINE_CURVE ( 2, ( #30206, #16427, #21158, #25750, #4393 ),
 .UNSPECIFIED., .F., .F. ) 
 B_SPLINE_CURVE_WITH_KNOTS ( ( 3, 2, 3 ),
 ( 0.9972222222222222321, 0.9981481481481481177, 1.000000000000000000 ),
 .UNSPECIFIED. ) 
 CURVE ( )  GEOMETRIC_REPRESENTATION_ITEM ( )  RATIONAL_B_SPLINE_CURVE ( ( 0.9330127018922194093, 0.9330127018922194093, 1.000000000000000000, 0.8660254037844388186, 1.000000000000000000 ) ) 
 REPRESENTATION_ITEM ( '' )  );
#21394 = CARTESIAN_POINT ( 'NONE',  ( 6.000000000000000888, 7.762456499804234384E-14, -142.5863248654051745 ) ) ;
#21395 = ORIENTED_EDGE ( 'NONE', *, *, #20409, .T. ) ;
#21396 = CARTESIAN_POINT ( 'NONE',  ( 6.000000000000052403, -1.607695154586662678, -106.6533121635130072 ) ) ;
#21397 = CARTESIAN_POINT ( 'NONE',  ( -5.999999999999963585, -1.487416814333745711E-14, -87.83632486540521711 ) ) ;
#21398 = DIRECTION ( 'NONE',  ( 1.000000000000000000, 1.665334536937731113E-16, 8.326672684688674053E-17 ) ) ;
#21399 = AXIS2_PLACEMENT_3D ( 'NONE', #13533, #27752, #6879 ) ;
#21400 = ORIENTED_EDGE ( 'NONE', *, *, #12507, .T. ) ;
#21401 = CARTESIAN_POINT ( 'NONE',  ( 116.4997167782376266, 1.308140751793640533, -1.308140751793640533 ) ) ;
#21402 = SURFACE_STYLE_FILL_AREA ( #26430 ) ;
#21403 = CARTESIAN_POINT ( 'NONE',  ( -7.216878364870328078, 0.000000000000000000, -102.6919872981078328 ) ) ;
#21404 = CARTESIAN_POINT ( 'NONE',  ( 159.0000000000000284, -19.99999999999998934, -4.000000000000003553 ) ) ;
#21405 = ADVANCED_FACE ( 'NONE', ( #2825 ), #9759, .F. ) ;
#21406 = CARTESIAN_POINT ( 'NONE',  ( 133.6875000000000284, 4.242640687119269671, 4.242640687119298093 ) ) ;
#21407 = CARTESIAN_POINT ( 'NONE',  ( 117.2499999999998721, 0.000000000000000000, 2.499999999999946709 ) ) ;
#21408 = CARTESIAN_POINT ( 'NONE',  ( -3.175426480542816510, -5.500000000000057732, -129.8750000000000284 ) ) ;
#21409 = ORIENTED_EDGE ( 'NONE', *, *, #13768, .F. ) ;
#21410 = CARTESIAN_POINT ( 'NONE',  ( -5.999999999999962697, 3.323446944526963260E-14, -162.8363248654052313 ) ) ;
#21411 = CARTESIAN_POINT ( 'NONE',  ( -3.175426480542816510, 5.499999999999865885, -59.87500000000005684 ) ) ;
#21412 = CARTESIAN_POINT ( 'NONE',  ( -3.464101615137757051, -5.999999999999979572, -81.58632486540517448 ) ) ;
#21413 = CARTESIAN_POINT ( 'NONE',  ( 159.1446212341123783, -12.00000000000001243, -4.000000000000004441 ) ) ;
#21414 = CARTESIAN_POINT ( 'NONE',  ( 3.608439182435180470, -6.249999999999997335, -86.55801270189223828 ) ) ;
#21415 = UNCERTAINTY_MEASURE_WITH_UNIT (LENGTH_MEASURE( 1.000000000000000082E-05 ), #21905, 'distance_accuracy_value', 'NONE');
#21416 = CARTESIAN_POINT ( 'NONE',  ( -1.000000000000000888, -9.000000000000007105, -4.000000000000003553 ) ) ;
#21417 = CARTESIAN_POINT ( 'NONE',  ( 105.7497167782376266, 1.308140751793696044, 1.308140751793640533 ) ) ;
#21418 = CARTESIAN_POINT ( 'NONE',  ( 0.000000000000000000, -5.999999999999991118, -175.9613248654052313 ) ) ;
#21419 = DIRECTION ( 'NONE',  ( 1.000000000000000000, -5.551115123125773458E-17, 0.000000000000000000 ) ) ;
#21420 = CARTESIAN_POINT ( 'NONE',  ( 116.4377832217621602, 1.849990392679621953, 0.7662911109081291805 ) ) ;
#21421 =( BOUNDED_CURVE ( )  B_SPLINE_CURVE ( 2, ( #10505, #19859, #28599, #8166, #26899, #7567, #26308, #16985, #11123 ),
 .UNSPECIFIED., .F., .T. ) 
 B_SPLINE_CURVE_WITH_KNOTS ( ( 3, 2, 2, 2, 3 ),
 ( 0.8305555555555556024, 0.8314814814814814881, 0.8333333333333333703, 0.8351851851851852526, 0.8361111111111111382 ),
 .UNSPECIFIED. ) 
 CURVE ( )  GEOMETRIC_REPRESENTATION_ITEM ( )  RATIONAL_B_SPLINE_CURVE ( ( 0.9330127018922194093, 0.9330127018922234061, 1.000000000000000000, 0.8660254037844388186, 1.000000000000000000, 0.8660254037844388186, 1.000000000000000000, 0.9330127018922194093, 0.9330127018922194093 ) ) 
 REPRESENTATION_ITEM ( '' )  );
#21422 = CARTESIAN_POINT ( 'NONE',  ( 6.350852961086080661, -9.614813431917819062E-14, -141.3750000000000568 ) ) ;
#21423 = CARTESIAN_POINT ( 'NONE',  ( 139.8520630996757177, -9.423463366246116024, 7.856467294622035524 ) ) ;
#21424 = CARTESIAN_POINT ( 'NONE',  ( -3.608439182435115633, 6.249999999999965361, -153.3080127018922383 ) ) ;
#21425 = CARTESIAN_POINT ( 'NONE',  ( 3.464101615137757051, -5.999999999999979572, -72.91367513459482552 ) ) ;
#21426 = EDGE_CURVE ( 'NONE', #24823, #18709, #23036, .T. ) ;
#21427 = CARTESIAN_POINT ( 'NONE',  ( 4.763139720814407951, 2.750000000000002665, -70.75000000000002842 ) ) ;
#21428 = CARTESIAN_POINT ( 'NONE',  ( 145.0238248654052029, 3.889087296526011706, -3.889087296526011706 ) ) ;
#21429 = DIRECTION ( 'NONE',  ( -7.147005652999508048E-36, 5.642372883946980038E-36, 1.000000000000000000 ) ) ;
#21430 = CARTESIAN_POINT ( 'NONE',  ( 4.763139720814407951, 2.750000000000002665, -66.25000000000002842 ) ) ;
#21431 =( BOUNDED_CURVE ( )  B_SPLINE_CURVE ( 2, ( #27329, #18310, #9064, #8920, #18457, #2157, #16175, #11404, #16022 ),
 .UNSPECIFIED., .F., .T. ) 
 B_SPLINE_CURVE_WITH_KNOTS ( ( 3, 2, 2, 2, 3 ),
 ( 0.5694444444444444198, 0.5703703703703704164, 0.5722222222222221877, 0.5740740740740740700, 0.5749999999999999556 ),
 .UNSPECIFIED. ) 
 CURVE ( )  GEOMETRIC_REPRESENTATION_ITEM ( )  RATIONAL_B_SPLINE_CURVE ( ( 0.9330127018922194093, 0.9330127018922154125, 1.000000000000000000, 0.8660254037844388186, 1.000000000000000000, 0.8660254037844388186, 1.000000000000000000, 0.9330127018922234061, 0.9330127018922194093 ) ) 
 REPRESENTATION_ITEM ( '' )  );
#21432 = CARTESIAN_POINT ( 'NONE',  ( 139.5983683982788648, -9.179625746858260271, 7.992216821685455663 ) ) ;
#21433 = CARTESIAN_POINT ( 'NONE',  ( 108.4761751345945697, 0.8284271247462053900, 2.000000000000151879 ) ) ;
#21434 = CARTESIAN_POINT ( 'NONE',  ( 160.6875000000000284, 4.242640687119269671, 4.242640687119298093 ) ) ;
#21435 = CARTESIAN_POINT ( 'NONE',  ( 135.0000000000025864, -7.147641677108396152, -8.399623149008458967 ) ) ;
#21436 = CARTESIAN_POINT ( 'NONE',  ( 136.0000000000000284, -8.798545334315205579, -8.160000000000000142 ) ) ;
#21437 = CARTESIAN_POINT ( 'NONE',  ( 6.000000000000000888, 1.743066579297358182E-13, -82.58632486540520290 ) ) ;
#21438 = EDGE_CURVE ( 'NONE', #20404, #3063, #23596, .T. ) ;
#21439 = ORIENTED_EDGE ( 'NONE', *, *, #24446, .F. ) ;
#21440 = CARTESIAN_POINT ( 'NONE',  ( 151.5000000000000284, 6.000000000000005329, 0.000000000000000000 ) ) ;
#21441 = CARTESIAN_POINT ( 'NONE',  ( -2.775557561562891351E-14, -5.500000000000115463, -153.7500000000000568 ) ) ;
#21442 = CARTESIAN_POINT ( 'NONE',  ( 3.464101615137757051, -5.999999999999979572, -158.4136751345948255 ) ) ;
#21443 = CARTESIAN_POINT ( 'NONE',  ( -5.412658773652739619, 3.124999999999975131, -47.31698729810784698 ) ) ;
#21444 = AXIS2_PLACEMENT_3D ( 'NONE', #19758, #29580, #8062 ) ;
#21445 = CARTESIAN_POINT ( 'NONE',  ( 20.50000000000015632, -1.999999999999890754, -5.551115123125782702E-14 ) ) ;
#21446 = CARTESIAN_POINT ( 'NONE',  ( -7.216878364870328078, 0.000000000000000000, -155.1919872981078186 ) ) ;
#21447 = ORIENTED_EDGE ( 'NONE', *, *, #3884, .F. ) ;
#21448 = CARTESIAN_POINT ( 'NONE',  ( 6.350852961086080661, -9.614813431917819062E-14, -91.87500000000001421 ) ) ;
#21449 = CARTESIAN_POINT ( 'NONE',  ( 7.216878364870455975, -6.409875621278545621E-14, -102.8080127018922383 ) ) ;
#21450 = ORIENTED_EDGE ( 'NONE', *, *, #28374, .T. ) ;
#21451 = CARTESIAN_POINT ( 'NONE',  ( 3.464101615137852974, 5.999999999999884537, -147.4136751345947687 ) ) ;
#21452 = CARTESIAN_POINT ( 'NONE',  ( 153.3601497308104058, -3.535533905932725318, -3.535533905932725318 ) ) ;
#21453 = VECTOR ( 'NONE', #10002, 1000.000000000000000 ) ;
#21454 = DIRECTION ( 'NONE',  ( -1.000000000000000000, 0.000000000000000000, 0.000000000000000000 ) ) ;
#21455 = LINE ( 'NONE', #2842, #11686 ) ;
#21456 = CARTESIAN_POINT ( 'NONE',  ( -5.196152422706573404, -3.000000000000002665, -68.21132486540520290 ) ) ;
#21457 = VECTOR ( 'NONE', #9423, 1000.000000000000000 ) ;
#21458 = VECTOR ( 'NONE', #11413, 1000.000000000000000 ) ;
#21459 =( NAMED_UNIT ( * ) SI_UNIT ( $, .STERADIAN. ) SOLID_ANGLE_UNIT ( ) );
#21460 = CARTESIAN_POINT ( 'NONE',  ( -3.175426480542816066, 5.499999999999865885, -164.8750000000000568 ) ) ;
#21461 = CARTESIAN_POINT ( 'NONE',  ( 0.000000000000000000, 5.999999999999977796, -58.21132486540525974 ) ) ;
#21462 = CARTESIAN_POINT ( 'NONE',  ( 3.175426480543072749, 5.499999999999865885, -151.6250000000000284 ) ) ;
#21463 = CIRCLE ( 'NONE', #13636, 1.000000000000000888 ) ;
#21464 = ADVANCED_FACE ( 'NONE', ( #16848 ), #21587, .T. ) ;
#21465 = CARTESIAN_POINT ( 'NONE',  ( 111.9374999999997868, 2.500000000000114575, -1.035533905932508825 ) ) ;
#21466 = CARTESIAN_POINT ( 'NONE',  ( 5.196152422706629359, -2.999999999999988898, -51.78867513459483973 ) ) ;
#21467 = EDGE_CURVE ( 'NONE', #5616, #29584, #19000, .T. ) ;
#21468 = CARTESIAN_POINT ( 'NONE',  ( 0.000000000000000000, 5.499999999999991118, -100.5000000000000284 ) ) ;
#21469 = CARTESIAN_POINT ( 'NONE',  ( 141.8363248654052029, 0.000000000000000000, -5.500000000000005329 ) ) ;
#21470 = CARTESIAN_POINT ( 'NONE',  ( 4.763139720814407951, -2.749999999999988454, -90.50000000000002842 ) ) ;
#21471 = DIRECTION ( 'NONE',  ( 1.000000000000000000, -0.000000000000000000, -0.000000000000000000 ) ) ;
#21472 = CARTESIAN_POINT ( 'NONE',  ( 158.0773502691896510, 5.000000000000004441, 0.000000000000000000 ) ) ;
#21473 = DIRECTION ( 'NONE',  ( -7.147005652999508048E-36, 5.642372883946980038E-36, 1.000000000000000000 ) ) ;
#21474 = CIRCLE ( 'NONE', #2784, 6.000000000000012434 ) ;
#21475 = CARTESIAN_POINT ( 'NONE',  ( 112.2499999999998153, -5.551115123125782702E-14, 2.500000000000168754 ) ) ;
#21476 = CYLINDRICAL_SURFACE ( 'NONE', #3076, 6.000000000000000888 ) ;
#21477 = CARTESIAN_POINT ( 'NONE',  ( -5.999999999999963585, -1.487416814333745711E-14, -71.91367513459482552 ) ) ;
#21478 = ADVANCED_FACE ( 'NONE', ( #6795 ), #1731, .T. ) ;
#21479 = DIRECTION ( 'NONE',  ( 6.938893903907222067E-15, -1.000000000000000000, 0.000000000000000000 ) ) ;
#21480 = ORIENTED_EDGE ( 'NONE', *, *, #11929, .T. ) ;
#21481 = CARTESIAN_POINT ( 'NONE',  ( 159.0000000000000284, -11.07692307692306777, -4.615384615384604317 ) ) ;
#21482 = DIRECTION ( 'NONE',  ( -0.000000000000000000, 1.000000000000000000, -0.000000000000000000 ) ) ;
#21483 = CARTESIAN_POINT ( 'NONE',  ( 106.4997167782374845, 1.308140751793640533, -1.308140751793418488 ) ) ;
#21484 = EDGE_LOOP ( 'NONE', ( #28101, #13754, #18021, #29808 ) ) ;
#21485 = STYLED_ITEM ( 'NONE', ( #14859 ), #5546 ) ;
#21486 = EDGE_LOOP ( 'NONE', ( #15823, #17062, #30229, #22262 ) ) ;
#21487 = CARTESIAN_POINT ( 'NONE',  ( 145.4062500000000284, 6.000000000000005329, -2.485281374238555774 ) ) ;
#21488 = ORIENTED_EDGE ( 'NONE', *, *, #9118, .T. ) ;
#21489 = CARTESIAN_POINT ( 'NONE',  ( 6.350852961086080661, -9.614813431917819062E-14, -117.3750000000000142 ) ) ;
#21490 = CARTESIAN_POINT ( 'NONE',  ( 17.18750000000010303, 1.097466725451679892, -2.649519052838358757 ) ) ;
#21491 = CARTESIAN_POINT ( 'NONE',  ( -5.412658773652739619, 3.124999999999975131, -123.1830127018922525 ) ) ;
#21492 = ORIENTED_EDGE ( 'NONE', *, *, #8921, .T. ) ;
#21493 = CARTESIAN_POINT ( 'NONE',  ( -6.000000000000007105, -1.607695154586655129, -68.84668783648704959 ) ) ;
#21494 = CARTESIAN_POINT ( 'NONE',  ( -7.216878364870328078, 0.000000000000000000, -164.1919872981078754 ) ) ;
#21495 = CARTESIAN_POINT ( 'NONE',  ( 110.3124999999998863, -1.035533905932659149, 2.500000000000144773 ) ) ;
#21496 = AXIS2_PLACEMENT_3D ( 'NONE', #6501, #6803, #6661 ) ;
#21497 = CARTESIAN_POINT ( 'NONE',  ( 134.1413997308104058, 2.071067811865468400, -4.999999999999989342 ) ) ;
#21498 = ORIENTED_EDGE ( 'NONE', *, *, #25462, .T. ) ;
#21499 = CARTESIAN_POINT ( 'NONE',  ( 0.2148510768240012581, -15.54319609401394331, -8.041199716608099735 ) ) ;
#21500 = CARTESIAN_POINT ( 'NONE',  ( -3.973952007372655526, 10.26128916632344357, -20.48836482813350912 ) ) ;
#21501 = CARTESIAN_POINT ( 'NONE',  ( 3.464101615137852974, 5.999999999999884537, -137.8363248654052313 ) ) ;
#21502 = CARTESIAN_POINT ( 'NONE',  ( -3.175426480542816510, -5.500000000000057732, -179.3750000000000568 ) ) ;
#21503 = CARTESIAN_POINT ( 'NONE',  ( 107.6877832217621744, -0.7662911109077987781, 1.849990392679652151 ) ) ;
#21504 = CARTESIAN_POINT ( 'NONE',  ( 6.000000000000000888, 1.607695154586715303, -100.5193375672974270 ) ) ;
#21505 = CARTESIAN_POINT ( 'NONE',  ( -5.412658773652684552, -3.125000000000099920, -176.9330127018922099 ) ) ;
#21506 = DIRECTION ( 'NONE',  ( -7.147005652999508048E-36, 5.642372883946980038E-36, 1.000000000000000000 ) ) ;
#21507 = EDGE_CURVE ( 'NONE', #14008, #7517, #20642, .T. ) ;
#21508 = CARTESIAN_POINT ( 'NONE',  ( -5.196152422706573404, -3.000000000000002665, -48.71132486540518869 ) ) ;
#21509 = CARTESIAN_POINT ( 'NONE',  ( 6.350852961086080661, -9.614813431917819062E-14, -121.8750000000000426 ) ) ;
#21510 = CARTESIAN_POINT ( 'NONE',  ( -4.763139720814407951, -2.750000000000016431, -116.5000000000000426 ) ) ;
#21511 = DIRECTION ( 'NONE',  ( -7.147005652999508048E-36, 5.642372883946980038E-36, 1.000000000000000000 ) ) ;
#21512 = CARTESIAN_POINT ( 'NONE',  ( -3.464101615137757051, -5.999999999999979572, -131.6636751345948539 ) ) ;
#21513 = ORIENTED_EDGE ( 'NONE', *, *, #610, .F. ) ;
#21514 = CARTESIAN_POINT ( 'NONE',  ( 17.00000000000007105, -1.873492889144845464, 1.873492889144845464 ) ) ;
#21515 = CARTESIAN_POINT ( 'NONE',  ( -5.999999999999963585, -1.487416814333745711E-14, -126.8363248654052171 ) ) ;
#21516 = CARTESIAN_POINT ( 'NONE',  ( -5.196152422706573404, -3.000000000000002665, -137.2113248654052029 ) ) ;
#21517 = CARTESIAN_POINT ( 'NONE',  ( 6.000000000000000888, 7.762456499804234384E-14, -132.0863248654052313 ) ) ;
#21518 = EDGE_CURVE ( 'NONE', #16922, #17680, #5388, .T. ) ;
#21519 = ADVANCED_FACE ( 'NONE', ( #13600 ), #20329, .T. ) ;
#21520 = ORIENTED_EDGE ( 'NONE', *, *, #5486, .T. ) ;
#21521 = DIRECTION ( 'NONE',  ( 0.000000000000000000, 5.551115123125767911E-17, -1.000000000000000000 ) ) ;
#21522 = CARTESIAN_POINT ( 'NONE',  ( -4.763139720814407951, -2.750000000000016431, -176.5000000000000000 ) ) ;
#21523 = EDGE_LOOP ( 'NONE', ( #14804, #652, #17150, #4428 ) ) ;
#21524 = CARTESIAN_POINT ( 'NONE',  ( 6.000000000000052403, -1.607695154586662678, -77.23066243270261566 ) ) ;
#21525 =( BOUNDED_CURVE ( )  B_SPLINE_CURVE ( 2, ( #3469, #29742, #27274, #24521, #6247, #8082, #1640, #18106, #29430 ),
 .UNSPECIFIED., .F., .T. ) 
 B_SPLINE_CURVE_WITH_KNOTS ( ( 3, 2, 2, 2, 3 ),
 ( 0.6638888888888889728, 0.6648148148148147474, 0.6666666666666667407, 0.6685185185185185119, 0.6694444444444445086 ),
 .UNSPECIFIED. ) 
 CURVE ( )  GEOMETRIC_REPRESENTATION_ITEM ( )  RATIONAL_B_SPLINE_CURVE ( ( 0.9330127018922194093, 0.9330127018922274029, 1.000000000000000000, 0.8660254037844388186, 1.000000000000000000, 0.8660254037844388186, 1.000000000000000000, 0.9330127018922154125, 0.9330127018922194093 ) ) 
 REPRESENTATION_ITEM ( '' )  );
#21526 = ORIENTED_EDGE ( 'NONE', *, *, #26698, .T. ) ;
#21527 = EDGE_LOOP ( 'NONE', ( #19728, #8066, #6388, #27263 ) ) ;
#21528 = CARTESIAN_POINT ( 'NONE',  ( 132.9375000000000284, -4.242640687119298093, -4.242640687119298093 ) ) ;
#21529 = CARTESIAN_POINT ( 'NONE',  ( 135.0148502691896510, -3.535533905932725318, -3.535533905932725318 ) ) ;
#21530 = ORIENTED_EDGE ( 'NONE', *, *, #5580, .F. ) ;
#21531 = CARTESIAN_POINT ( 'NONE',  ( -3.608439182435115633, 6.249999999999965361, -128.4419872981078186 ) ) ;
#21532 = CARTESIAN_POINT ( 'NONE',  ( 12.56249999999998579, 1.097466725451619718, 2.649519052838178457 ) ) ;
#21533 = CARTESIAN_POINT ( 'NONE',  ( 18.96132486540530593, 1.110223024625156540E-13, 2.499999999999724665 ) ) ;
#21534 = ORIENTED_EDGE ( 'NONE', *, *, #24317, .F. ) ;
#21535 = CARTESIAN_POINT ( 'NONE',  ( 18.93750000000016698, 2.000000000000091926, -0.8284271247462354770 ) ) ;
#21536 = DIRECTION ( 'NONE',  ( -7.147005652999508048E-36, 5.642372883946980038E-36, 1.000000000000000000 ) ) ;
#21537 = CARTESIAN_POINT ( 'NONE',  ( 5.196152422706629359, -2.999999999999988898, -91.71132486540523132 ) ) ;
#21538 = CARTESIAN_POINT ( 'NONE',  ( 137.7976497308104058, 0.000000000000000000, 5.000000000000004441 ) ) ;
#21539 = CARTESIAN_POINT ( 'NONE',  ( 23.03867513459492855, 2.220446049250313081E-13, -2.500000000000057732 ) ) ;
#21540 = LINE ( 'NONE', #14777, #14814 ) ;
#21541 = CARTESIAN_POINT ( 'NONE',  ( 15.28867513459483618, 2.500000000000113243, -1.665334536937734811E-13 ) ) ;
#21542 = CYLINDRICAL_SURFACE ( 'NONE', #7665, 6.000000000000000888 ) ;
#21543 = CARTESIAN_POINT ( 'NONE',  ( 109.0863248654051034, -1.414213562373145550, 1.414213562373256572 ) ) ;
#21544 = CARTESIAN_POINT ( 'NONE',  ( 105.7499999999998010, 1.110223024625156540E-13, -2.499999999999946709 ) ) ;
#21545 = EDGE_CURVE ( 'NONE', #10765, #29837, #23281, .T. ) ;
#21546 = FACE_OUTER_BOUND ( 'NONE', #20075, .T. ) ;
#21547 = EDGE_LOOP ( 'NONE', ( #22763, #9991, #26377, #27232 ) ) ;
#21548 = CARTESIAN_POINT ( 'NONE',  ( -4.763139720814407951, 2.749999999999946709, -49.25000000000001421 ) ) ;
#21549 = EDGE_CURVE ( 'NONE', #22218, #6732, #25781, .T. ) ;
#21550 = CARTESIAN_POINT ( 'NONE',  ( 0.000000000000000000, 0.000000000000000000, 0.000000000000000000 ) ) ;
#21551 = CARTESIAN_POINT ( 'NONE',  ( -5.999999999999971578, 1.607695154586715303, -152.4033121635129930 ) ) ;
#21552 = ORIENTED_EDGE ( 'NONE', *, *, #22293, .T. ) ;
#21553 = CARTESIAN_POINT ( 'NONE',  ( 115.7497167782375698, 1.308140751793751555, 1.308140751793973600 ) ) ;
#21554 = CARTESIAN_POINT ( 'NONE',  ( 12.46132486540529882, 1.110223024625156540E-13, -2.500000000000057732 ) ) ;
#21555 = CARTESIAN_POINT ( 'NONE',  ( 11.81250000000006040, 0.8284271247463557142, -2.000000000000031530 ) ) ;
#21556 = CARTESIAN_POINT ( 'NONE',  ( -3.608439182435115633, 6.249999999999965361, -102.9419872981078470 ) ) ;
#21557 = CARTESIAN_POINT ( 'NONE',  ( 132.9375000000000284, -4.242640687119298093, -4.242640687119298093 ) ) ;
#21558 = CARTESIAN_POINT ( 'NONE',  ( 116.6874999999997726, -1.035533905932659149, -2.499999999999784173 ) ) ;
#21559 = CARTESIAN_POINT ( 'NONE',  ( -4.763139720814407951, 2.749999999999946709, -130.2500000000000284 ) ) ;
#21560 = VERTEX_POINT ( 'NONE', #23103 ) ;
#21561 = CARTESIAN_POINT ( 'NONE',  ( 6.000000000000000888, 1.743066579297358182E-13, -61.58632486540521001 ) ) ;
#21562 = CARTESIAN_POINT ( 'NONE',  ( -2.775557561562891351E-14, -5.500000000000115463, -57.75000000000002132 ) ) ;
#21563 = AXIS2_PLACEMENT_3D ( 'NONE', #23500, #20731, #18904 ) ;
#21564 = CARTESIAN_POINT ( 'NONE',  ( -5.196152422706573404, -3.000000000000002665, -81.71132486540521711 ) ) ;
#21565 = CARTESIAN_POINT ( 'NONE',  ( -9.999999999999980460, -60.00000000000001421, 3.000000000000002665 ) ) ;
#21566 = CARTESIAN_POINT ( 'NONE',  ( 5.412658773652712085, -3.125000000000086153, -80.43301270189223828 ) ) ;
#21567 = AXIS2_PLACEMENT_3D ( 'NONE', #12639, #19682, #1080 ) ;
#21568 = DIRECTION ( 'NONE',  ( 1.000000000000000000, 1.665334536937736783E-16, 2.220446049250315546E-16 ) ) ;
#21569 = CARTESIAN_POINT ( 'NONE',  ( 106.3747167782374703, -5.551115123125782702E-14, -1.849990392679523588 ) ) ;
#21570 =( NAMED_UNIT ( * ) PLANE_ANGLE_UNIT ( ) SI_UNIT ( $, .RADIAN. ) );
#21571 = EDGE_CURVE ( 'NONE', #20811, #4004, #22790, .T. ) ;
#21572 = CARTESIAN_POINT ( 'NONE',  ( 113.4377832217621460, 1.849990392679591977, 0.7662911109080692285 ) ) ;
#21573 = EDGE_CURVE ( 'NONE', #20381, #8862, #18951, .T. ) ;
#21574 = CARTESIAN_POINT ( 'NONE',  ( 3.175426480543072749, -5.500000000000105693, -138.6250000000000568 ) ) ;
#21575 = LINE ( 'NONE', #28597, #24591 ) ;
#21576 = CARTESIAN_POINT ( 'NONE',  ( -3.608439182435052128, -6.250000000000110134, -149.8080127018922667 ) ) ;
#21577 = CARTESIAN_POINT ( 'NONE',  ( 161.0000000000000284, 1.347111479062088799E-15, 11.00000000000000355 ) ) ;
#21578 = CARTESIAN_POINT ( 'NONE',  ( 3.175426480543072749, -5.500000000000105693, -71.12500000000004263 ) ) ;
#21579 = CARTESIAN_POINT ( 'NONE',  ( -3.175426480542816510, -5.500000000000057732, -63.87500000000001421 ) ) ;
#21580 = DIRECTION ( 'NONE',  ( -7.147005652999508048E-36, 5.642372883946980038E-36, 1.000000000000000000 ) ) ;
#21581 = CARTESIAN_POINT ( 'NONE',  ( 146.6398502691896510, -3.535533905932752852, 3.535533905932725318 ) ) ;
#21582 = DIRECTION ( 'NONE',  ( 1.000000000000000000, 6.938893903907222067E-15, 0.000000000000000000 ) ) ;
#21583 = CARTESIAN_POINT ( 'NONE',  ( 154.3125000000000284, 4.242640687119298093, -4.242640687119298093 ) ) ;
#21584 = CARTESIAN_POINT ( 'NONE',  ( -0.5000000000000004441, -14.50000000000001243, -8.500000000000007105 ) ) ;
#21585 = AXIS2_PLACEMENT_3D ( 'NONE', #26119, #5217, #7527 ) ;
#21586 = CARTESIAN_POINT ( 'NONE',  ( 3.464101615137757051, -5.999999999999979572, -57.91367513459482552 ) ) ;
#21587 = CYLINDRICAL_SURFACE ( 'NONE', #6173, 6.000000000000000888 ) ;
#21588 = ORIENTED_EDGE ( 'NONE', *, *, #1725, .T. ) ;
#21589 = CIRCLE ( 'NONE', #19606, 0.5000000000000004441 ) ;
#21590 = CARTESIAN_POINT ( 'NONE',  ( 151.0312500000000568, -2.485281374238555774, -6.000000000000005329 ) ) ;
#21591 = CARTESIAN_POINT ( 'NONE',  ( -4.999999999999886313, -10.00000000000000888, 8.000000000000007105 ) ) ;
#21592 = CARTESIAN_POINT ( 'NONE',  ( 6.000000000000000888, 1.743066579297358182E-13, -102.0863248654051887 ) ) ;
#21593 = CARTESIAN_POINT ( 'NONE',  ( -3.175426480542816510, 5.499999999999865885, -176.8750000000000568 ) ) ;
#21594 = CARTESIAN_POINT ( 'NONE',  ( 20.18750000000014566, 0.8284271247463557142, 1.999999999999911626 ) ) ;
#21595 = EDGE_LOOP ( 'NONE', ( #24831, #29991, #28807, #26839 ) ) ;
#21596 = CARTESIAN_POINT ( 'NONE',  ( 3.608439182435180470, -6.249999999999997335, -151.6919872981078186 ) ) ;
#21597 = EDGE_LOOP ( 'NONE', ( #15262, #29647, #7516, #6808, #15690 ) ) ;
#21598 = CARTESIAN_POINT ( 'NONE',  ( 6.350852961086080661, -9.614813431917819062E-14, -84.37500000000005684 ) ) ;
#21599 = CARTESIAN_POINT ( 'NONE',  ( 15.87500000000016698, -2.649519052838000821, -1.110223024625156540E-13 ) ) ;
#21600 =( BOUNDED_CURVE ( )  B_SPLINE_CURVE ( 2, ( #29441, #20097, #1651, #8414, #6109, #15521, #15001, #7909, #14436 ),
 .UNSPECIFIED., .F., .T. ) 
 B_SPLINE_CURVE_WITH_KNOTS ( ( 3, 2, 2, 2, 3 ),
 ( 0.2874999999999998113, 0.2937499999999995670, 0.2999999999999993783, 0.3062499999999991340, 0.3124999999999988898 ),
 .UNSPECIFIED. ) 
 CURVE ( )  GEOMETRIC_REPRESENTATION_ITEM ( )  RATIONAL_B_SPLINE_CURVE ( ( 1.000000000000001998, 0.9238795325112847401, 1.000000000000000000, 0.9238795325112867385, 1.000000000000000000, 0.9238795325112867385, 1.000000000000000000, 0.9238795325113002832, 0.9999999999999864553 ) ) 
 REPRESENTATION_ITEM ( '' )  );
#21601 = ORIENTED_EDGE ( 'NONE', *, *, #19113, .T. ) ;
#21602 = CARTESIAN_POINT ( 'NONE',  ( 6.000000000000000888, -6.507448562710137091E-15, -176.1636751345947971 ) ) ;
#21603 = FACE_OUTER_BOUND ( 'NONE', #5053, .T. ) ;
#21604 = CARTESIAN_POINT ( 'NONE',  ( -3.464101615137725076, 5.999999999999979572, -58.66367513459482552 ) ) ;
#21605 = COLOUR_RGB ( '', 0.66274510, 0.83137255, 0.94901961) ;
#21606 = CARTESIAN_POINT ( 'NONE',  ( 111.3363248654049755, -1.414213562373256572, -1.414213562372923505 ) ) ;
#21607 = CARTESIAN_POINT ( 'NONE',  ( 135.4056618780830092, -8.496329914204098444, 8.215405480166593222 ) ) ;
#21608 =( NAMED_UNIT ( * ) PLANE_ANGLE_UNIT ( ) SI_UNIT ( $, .RADIAN. ) );
#21609 = EDGE_CURVE ( 'NONE', #21672, #15617, #15618, .T. ) ;
#21610 =( BOUNDED_CURVE ( )  B_SPLINE_CURVE ( 2, ( #5033, #21053, #28381, #9675, #12310, #11708, #19352, #7361, #434 ),
 .UNSPECIFIED., .F., .T. ) 
 B_SPLINE_CURVE_WITH_KNOTS ( ( 3, 2, 2, 2, 3 ),
 ( 0.5916666666666666741, 0.5925925925925925597, 0.5944444444444444420, 0.5962962962962963243, 0.5972222222222222099 ),
 .UNSPECIFIED. ) 
 CURVE ( )  GEOMETRIC_REPRESENTATION_ITEM ( )  RATIONAL_B_SPLINE_CURVE ( ( 0.9330127018922194093, 0.9330127018922194093, 1.000000000000000000, 0.8660254037844388186, 1.000000000000000000, 0.8660254037844388186, 1.000000000000000000, 0.9330127018922194093, 0.9330127018922194093 ) ) 
 REPRESENTATION_ITEM ( '' )  );
#21611 = CARTESIAN_POINT ( 'NONE',  ( 6.350852961086080661, -9.614813431917819062E-14, -166.8750000000000568 ) ) ;
#21612 = CARTESIAN_POINT ( 'NONE',  ( 135.0000000000000284, -6.982120021884474781, -8.500000000000007105 ) ) ;
#21613 = CARTESIAN_POINT ( 'NONE',  ( 6.350852961086080661, -9.614813431917819062E-14, -153.3750000000000000 ) ) ;
#21614 = CARTESIAN_POINT ( 'NONE',  ( 104.8415063509460055, -1.908493649053821795, 1.110223024625156540E-13 ) ) ;
#21615 = CARTESIAN_POINT ( 'NONE',  ( 3.464101615137757051, -5.999999999999979572, -103.8363248654052171 ) ) ;
#21616 = CARTESIAN_POINT ( 'NONE',  ( 4.763139720814407951, -2.749999999999988454, -93.50000000000002842 ) ) ;
#21617 = CARTESIAN_POINT ( 'NONE',  ( 24.16367513459488592, 1.767766952966487448, -1.767766952966431937 ) ) ;
#21618 = CARTESIAN_POINT ( 'NONE',  ( 3.175426480543072749, 5.499999999999865885, -85.62500000000000000 ) ) ;
#21619 = CARTESIAN_POINT ( 'NONE',  ( 135.1800748654052029, -2.278174593051888408, 5.500000000000135891 ) ) ;
#21620 = CARTESIAN_POINT ( 'NONE',  ( 157.0461002691896795, -2.071067811865468400, 4.999999999999989342 ) ) ;
#21621 = DIRECTION ( 'NONE',  ( 1.000000000000000000, 0.000000000000000000, 0.000000000000000000 ) ) ;
#21622 = CARTESIAN_POINT ( 'NONE',  ( 23.75000000000013145, 1.665334536937734811E-13, -2.000000000000057288 ) ) ;
#21623 = CARTESIAN_POINT ( 'NONE',  ( 114.1250000000000142, 1.767766952966293159, 1.767766952966320915 ) ) ;
#21624 = CARTESIAN_POINT ( 'NONE',  ( 117.2886751345947971, 2.000000000000140332, 2.220446049250313081E-13 ) ) ;
#21625 = LINE ( 'NONE', #998, #14629 ) ;
#21626 = CARTESIAN_POINT ( 'NONE',  ( 0.000000000000000000, 0.000000000000000000, 0.000000000000000000 ) ) ;
#21627 = EDGE_LOOP ( 'NONE', ( #22711, #5046, #2914, #7367 ) ) ;
#21628 = DIRECTION ( 'NONE',  ( 0.000000000000000000, 0.000000000000000000, -1.000000000000000000 ) ) ;
#21629 = CARTESIAN_POINT ( 'NONE',  ( 119.1877832217621034, 0.7662911109078588412, -1.849990392679411677 ) ) ;
#21630 = TOROIDAL_SURFACE ( 'NONE', #26986, 6.000000000000000000, 5.000000000000004441 ) ;
#21631 = ORIENTED_EDGE ( 'NONE', *, *, #12931, .T. ) ;
#21632 = ORIENTED_EDGE ( 'NONE', *, *, #13594, .T. ) ;
#21633 = ORIENTED_EDGE ( 'NONE', *, *, #15885, .F. ) ;
#21634 = EDGE_CURVE ( 'NONE', #25526, #11814, #9607, .T. ) ;
#21635 = CARTESIAN_POINT ( 'NONE',  ( -3.175426480542816510, -5.500000000000057732, -108.8750000000000426 ) ) ;
#21636 = CARTESIAN_POINT ( 'NONE',  ( 3.608439182435180470, -6.249999999999997335, -124.0580127018922099 ) ) ;
#21637 = EDGE_LOOP ( 'NONE', ( #24222, #20205, #14911, #9837 ) ) ;
#21638 = CARTESIAN_POINT ( 'NONE',  ( 2.081668171172167281E-16, 3.582034040661430693E-16, -2.499999999999999112 ) ) ;
#21639 = CARTESIAN_POINT ( 'NONE',  ( -5.412658773652684552, -3.125000000000099920, -159.5669872981078186 ) ) ;
#21640 = CARTESIAN_POINT ( 'NONE',  ( 108.1249999999999574, 1.767766952966293159, 1.767766952966431937 ) ) ;
#21641 = CARTESIAN_POINT ( 'NONE',  ( 133.8601497308104342, -3.535533905932725318, -3.535533905932725318 ) ) ;
#21642 = CARTESIAN_POINT ( 'NONE',  ( -3.608439182435115633, 6.249999999999965361, -63.30801270189224539 ) ) ;
#21643 = ORIENTED_EDGE ( 'NONE', *, *, #26320, .F. ) ;
#21644 = ADVANCED_FACE ( 'NONE', ( #8812 ), #24918, .F. ) ;
#21645 = CARTESIAN_POINT ( 'NONE',  ( -3.675482141847861151, 10.37335300580275188, -20.24150316489821932 ) ) ;
#21646 = CARTESIAN_POINT ( 'NONE',  ( 117.7886751345947545, -1.999999999999946265, 1.110223024625156540E-13 ) ) ;
#21647 = CARTESIAN_POINT ( 'NONE',  ( -6.350852961085760029, -1.281975124255709124E-13, -175.1250000000000284 ) ) ;
#21648 = CARTESIAN_POINT ( 'NONE',  ( 108.8752832217621744, -1.849990392679468076, 1.110223024625156540E-13 ) ) ;
#21649 = APPLICATION_CONTEXT ( 'automotive_design' ) ;
#21650 = CARTESIAN_POINT ( 'NONE',  ( -5.196152422706601826, 2.999999999999975131, -99.96132486540520290 ) ) ;
#21651 = CARTESIAN_POINT ( 'NONE',  ( -5.412658773652684552, -3.125000000000099920, -178.4330127018922667 ) ) ;
#21652 = CARTESIAN_POINT ( 'NONE',  ( 119.7261751345945413, -1.999999999999941602, 0.8284271247464759513 ) ) ;
#21653 =( LENGTH_UNIT ( ) NAMED_UNIT ( * ) SI_UNIT ( .MILLI., .METRE. ) );
#21654 = CARTESIAN_POINT ( 'NONE',  ( -3.175426480542816066, -5.500000000000057732, -113.3750000000000568 ) ) ;
#21655 = CARTESIAN_POINT ( 'NONE',  ( 11.00000000000001599, -6.106226635438360972E-16, -14.99152654425661702 ) ) ;
#21656 = CARTESIAN_POINT ( 'NONE',  ( 6.350852961086080661, -9.614813431917819062E-14, -115.8750000000000000 ) ) ;
#21657 = FILL_AREA_STYLE_COLOUR ( '', #17583 ) ;
#21658 = FACE_OUTER_BOUND ( 'NONE', #17675, .T. ) ;
#21659 = CIRCLE ( 'NONE', #9393, 0.5000000000000004441 ) ;
#21660 = VERTEX_POINT ( 'NONE', #29 ) ;
#21661 = CARTESIAN_POINT ( 'NONE',  ( 18.93750000000004619, -1.097466725451439196, 2.649519052838178457 ) ) ;
#21662 = CARTESIAN_POINT ( 'NONE',  ( 135.0000000000000284, 0.000000000000000000, 0.000000000000000000 ) ) ;
#21663 = DIRECTION ( 'NONE',  ( 1.000000000000000000, 0.000000000000000000, -0.000000000000000000 ) ) ;
#21664 = VERTEX_POINT ( 'NONE', #16218 ) ;
#21665 = CARTESIAN_POINT ( 'NONE',  ( -5.999999999999963585, -1.487416814333745711E-14, -126.8363248654052171 ) ) ;
#21666 = MECHANICAL_DESIGN_GEOMETRIC_PRESENTATION_REPRESENTATION (  '', ( #25574 ), #14108 ) ;
#21667 = CARTESIAN_POINT ( 'NONE',  ( 17.16367513459499250, 1.767766952966431937, -1.767766952966431937 ) ) ;
#21668 = CARTESIAN_POINT ( 'NONE',  ( 22.64882486540529172, 2.500000000000144773, -1.035533905932809473 ) ) ;
#21669 = ORIENTED_EDGE ( 'NONE', *, *, #12923, .T. ) ;
#21670 = CARTESIAN_POINT ( 'NONE',  ( 22.28867513459495342, 2.500000000000113243, -1.665334536937734811E-13 ) ) ;
#21671 = ORIENTED_EDGE ( 'NONE', *, *, #12036, .F. ) ;
#21672 = VERTEX_POINT ( 'NONE', #4639 ) ;
#21673 = CARTESIAN_POINT ( 'NONE',  ( 5.999999999999949374, 1.607695154586804565, -85.51933756729742697 ) ) ;
#21674 = CARTESIAN_POINT ( 'NONE',  ( 160.6875000000000284, 4.242640687119269671, 4.242640687119298093 ) ) ;
#21675 = ADVANCED_FACE ( 'NONE', ( #18804 ), #186, .T. ) ;
#21676 = AXIS2_PLACEMENT_3D ( 'NONE', #18755, #4743, #1987 ) ;
#21677 = CARTESIAN_POINT ( 'NONE',  ( -3.608439182435115633, 6.249999999999965361, -134.4419872981077901 ) ) ;
#21678 = CARTESIAN_POINT ( 'NONE',  ( 24.21132486540530948, -2.499999999999946709, -2.220446049250313081E-13 ) ) ;
#21679 = AXIS2_PLACEMENT_3D ( 'NONE', #11717, #23666, #2743 ) ;
#21680 = AXIS2_PLACEMENT_3D ( 'NONE', #7559, #26300, #5254 ) ;
#21681 = CARTESIAN_POINT ( 'NONE',  ( 5.196152422706629359, 3.000000000000002665, -131.0386751345948824 ) ) ;
#21682 = CARTESIAN_POINT ( 'NONE',  ( 144.0074251345948539, 2.278174593051996322, -5.500000000000026645 ) ) ;
#21683 = ORIENTED_EDGE ( 'NONE', *, *, #22928, .F. ) ;
#21684 = CARTESIAN_POINT ( 'NONE',  ( 0.000000000000000000, 5.999999999999977796, -135.2886751345948539 ) ) ;
#21685 = EDGE_CURVE ( 'NONE', #27377, #2648, #18960, .T. ) ;
#21686 = CARTESIAN_POINT ( 'NONE',  ( 3.464101615137757051, -5.999999999999979572, -91.83632486540516027 ) ) ;
#21687 = EDGE_CURVE ( 'NONE', #14008, #3491, #17998, .T. ) ;
#21688 = CARTESIAN_POINT ( 'NONE',  ( 140.3288997308104058, 4.999999999999989342, -2.071067811865468400 ) ) ;
#21689 = DIRECTION ( 'NONE',  ( 0.8660254037844381525, -0.5000000000000008882, -2.220446049250315053E-16 ) ) ;
#21690 = CARTESIAN_POINT ( 'NONE',  ( 0.000000000000000000, 5.999999999999977796, -146.7113248654052313 ) ) ;
#21691 = DIRECTION ( 'NONE',  ( 1.000000000000000000, -5.551115123125773458E-17, -1.260129944081490338E-35 ) ) ;
#21692 = CARTESIAN_POINT ( 'NONE',  ( 107.3749999999999574, -1.767766952966293159, 1.767766952966431937 ) ) ;
#21693 = CARTESIAN_POINT ( 'NONE',  ( 0.000000000000000000, 5.499999999999991118, -141.0000000000000000 ) ) ;
#21694 = AXIS2_PLACEMENT_3D ( 'NONE', #1299, #10712, #8526 ) ;
#21695 = CARTESIAN_POINT ( 'NONE',  ( 104.7401757384974275, 1.849990392679522477, -0.1213543097418731814 ) ) ;
#21696 = ORIENTED_EDGE ( 'NONE', *, *, #11584, .F. ) ;
#21697 = CARTESIAN_POINT ( 'NONE',  ( 0.000000000000000000, 5.499999999999991118, -51.00000000000004263 ) ) ;
#21698 = DIRECTION ( 'NONE',  ( -7.147005652999508048E-36, 5.642372883946980038E-36, 1.000000000000000000 ) ) ;
#21699 = DIRECTION ( 'NONE',  ( 0.000000000000000000, -0.3428396514843867759, 0.9393939393939395588 ) ) ;
#21700 =( BOUNDED_CURVE ( )  B_SPLINE_CURVE ( 2, ( #1037, #20393, #22405, #29750, #6400, #8726, #6108, #24389, #24533 ),
 .UNSPECIFIED., .F., .T. ) 
 B_SPLINE_CURVE_WITH_KNOTS ( ( 3, 2, 2, 2, 3 ),
 ( 0.5138888888888888395, 0.5148148148148148362, 0.5166666666666667185, 0.5185185185185184897, 0.5194444444444444864 ),
 .UNSPECIFIED. ) 
 CURVE ( )  GEOMETRIC_REPRESENTATION_ITEM ( )  RATIONAL_B_SPLINE_CURVE ( ( 0.9330127018922194093, 0.9330127018922154125, 1.000000000000000000, 0.8660254037844388186, 1.000000000000000000, 0.8660254037844388186, 1.000000000000000000, 0.9330127018922154125, 0.9330127018922194093 ) ) 
 REPRESENTATION_ITEM ( '' )  );
#21701 = CARTESIAN_POINT ( 'NONE',  ( 5.196152422706629359, 3.000000000000002665, -152.9613248654052597 ) ) ;
#21702 = VERTEX_POINT ( 'NONE', #14364 ) ;
#21703 = CARTESIAN_POINT ( 'NONE',  ( 117.4997167782374987, 1.308140751793696044, -1.308140751793640533 ) ) ;
#21704 = CARTESIAN_POINT ( 'NONE',  ( 5.412658773652712085, -3.125000000000086153, -99.06698729810781856 ) ) ;
#21705 = DIRECTION ( 'NONE',  ( -7.147005652999508048E-36, 5.642372883946980038E-36, 1.000000000000000000 ) ) ;
#21706 = CARTESIAN_POINT ( 'NONE',  ( 20.52382486540534856, 1.035533905932809473, -2.499999999999904521 ) ) ;
#21707 = CARTESIAN_POINT ( 'NONE',  ( 117.6250000000000000, -1.767766952966376426, -1.767766952966320915 ) ) ;
#21708 = CYLINDRICAL_SURFACE ( 'NONE', #9085, 6.000000000000000888 ) ;
#21709 = ADVANCED_FACE ( 'NONE', ( #7256 ), #23702, .T. ) ;
#21710 = CARTESIAN_POINT ( 'NONE',  ( 4.763139720814407951, -2.749999999999988454, -129.5000000000000000 ) ) ;
#21711 = ORIENTED_EDGE ( 'NONE', *, *, #26401, .F. ) ;
#21712 = CARTESIAN_POINT ( 'NONE',  ( 116.0000000000000142, 6.735557395310442023E-16, 5.500000000000000000 ) ) ;
#21713 = CARTESIAN_POINT ( 'NONE',  ( -2.775557561562891351E-14, -5.500000000000115463, -60.75000000000002842 ) ) ;
#21714 = FACE_OUTER_BOUND ( 'NONE', #18245, .T. ) ;
#21715 = CARTESIAN_POINT ( 'NONE',  ( 140.5000000000000284, -10.99818166789401275, -4.799999999999998934 ) ) ;
#21716 = EDGE_CURVE ( 'NONE', #25854, #17182, #8296, .T. ) ;
#21717 = CARTESIAN_POINT ( 'NONE',  ( 3.977757852569170804, 10.25981801084817135, -29.50831862515141069 ) ) ;
#21718 = CARTESIAN_POINT ( 'NONE',  ( -5.412658773652684552, -3.125000000000099920, -86.93301270189223828 ) ) ;
#21719 = CARTESIAN_POINT ( 'NONE',  ( 6.000000000000000888, -1.607695154586752384, -100.6533121635130072 ) ) ;
#21720 = DIRECTION ( 'NONE',  ( -5.551115123125774074E-17, -1.000000000000000000, -6.394689268473234689E-36 ) ) ;
#21721 = SURFACE_STYLE_FILL_AREA ( #19565 ) ;
#21722 = CARTESIAN_POINT ( 'NONE',  ( -10.00000000000000178, -89.00000000000001421, -4.000000000000003553 ) ) ;
#21723 = CARTESIAN_POINT ( 'NONE',  ( 115.3127832217621886, 1.849990392679562001, -0.7662911109076485650 ) ) ;
#21724 = CARTESIAN_POINT ( 'NONE',  ( -3.175426480542816066, 5.499999999999865885, -136.3750000000000568 ) ) ;
#21725 = CARTESIAN_POINT ( 'NONE',  ( 139.9385832302453991, -9.134974910517927427, 7.783976842244119787 ) ) ;
#21726 = CARTESIAN_POINT ( 'NONE',  ( 7.216878364870455975, -6.409875621278545621E-14, -150.8080127018922099 ) ) ;
#21727 = CARTESIAN_POINT ( 'NONE',  ( 6.000000000000052403, -1.607695154586662678, -70.65331216351297883 ) ) ;
#21728 = SURFACE_STYLE_FILL_AREA ( #26606 ) ;
#21729 = CARTESIAN_POINT ( 'NONE',  ( -3.175426480542816066, 5.499999999999865885, -67.37500000000002842 ) ) ;
#21730 = CARTESIAN_POINT ( 'NONE',  ( 5.196152422706629359, 3.000000000000002665, -114.5386751345948113 ) ) ;
#21731 = CARTESIAN_POINT ( 'NONE',  ( 6.350852961086080661, -9.614813431917819062E-14, -54.37500000000002842 ) ) ;
#21732 = FILL_AREA_STYLE_COLOUR ( '', #11138 ) ;
#21733 = CARTESIAN_POINT ( 'NONE',  ( 145.2336002691896795, -4.999999999999989342, 2.071067811865468400 ) ) ;
#21734 = CARTESIAN_POINT ( 'NONE',  ( 150.0937500000000284, 6.000000000000005329, 2.485281374238585972 ) ) ;
#21735 = CARTESIAN_POINT ( 'NONE',  ( 0.000000000000000000, 0.000000000000000000, -44.99152654425658682 ) ) ;
#21736 = CARTESIAN_POINT ( 'NONE',  ( 17.75000000000015632, 1.110223024625156540E-13, -2.000000000000001776 ) ) ;
#21737 = CARTESIAN_POINT ( 'NONE',  ( 0.000000000000000000, -5.999999999999991118, -98.53867513459479710 ) ) ;
#21738 = VECTOR ( 'NONE', #25677, 1000.000000000000000 ) ;
#21739 = ORIENTED_EDGE ( 'NONE', *, *, #11188, .T. ) ;
#21740 = CARTESIAN_POINT ( 'NONE',  ( 142.9687500000000000, -2.485281374238585972, 6.000000000000005329 ) ) ;
#21741 =( BOUNDED_CURVE ( )  B_SPLINE_CURVE ( 2, ( #20246, #11037, #4241, #22548, #20382, #27571, #1482, #15971, #6551 ),
 .UNSPECIFIED., .F., .F. ) 
 B_SPLINE_CURVE_WITH_KNOTS ( ( 3, 2, 2, 2, 3 ),
 ( 0.8416666666666666741, 0.8425925925925925597, 0.8444444444444444420, 0.8462962962962963243, 0.8472222222222222099 ),
 .UNSPECIFIED. ) 
 CURVE ( )  GEOMETRIC_REPRESENTATION_ITEM ( )  RATIONAL_B_SPLINE_CURVE ( ( 0.9330127018922194093, 0.9330127018922194093, 1.000000000000000000, 0.8660254037844388186, 1.000000000000000000, 0.8660254037844388186, 1.000000000000000000, 0.9330127018922194093, 0.9330127018922194093 ) ) 
 REPRESENTATION_ITEM ( '' )  );
#21742 = EDGE_CURVE ( 'NONE', #15338, #16735, #11494, .T. ) ;
#21743 = UNCERTAINTY_MEASURE_WITH_UNIT (LENGTH_MEASURE( 1.000000000000000082E-05 ), #19254, 'distance_accuracy_value', 'NONE');
#21744 = EDGE_CURVE ( 'NONE', #20037, #29700, #10292, .T. ) ;
#21745 = CARTESIAN_POINT ( 'NONE',  ( 6.000000000000014211, -1.607695154586730180, -158.2306624327026441 ) ) ;
#21746 = CARTESIAN_POINT ( 'NONE',  ( -6.350852961085760029, -1.281975124255709124E-13, -176.6250000000000568 ) ) ;
#21747 = CARTESIAN_POINT ( 'NONE',  ( 19.50000000000009948, -1.999999999999835243, 0.000000000000000000 ) ) ;
#21748 = CARTESIAN_POINT ( 'NONE',  ( 5.412658773652739619, 3.124999999999988898, -152.8169872981078186 ) ) ;
#21749 = ORIENTED_EDGE ( 'NONE', *, *, #15132, .T. ) ;
#21750 = CARTESIAN_POINT ( 'NONE',  ( -2.775557561562891351E-14, -5.500000000000115463, -84.74999999999998579 ) ) ;
#21751 = CARTESIAN_POINT ( 'NONE',  ( 3.608439182435180470, -6.249999999999997335, -103.0580127018922383 ) ) ;
#21752 = CARTESIAN_POINT ( 'NONE',  ( 0.000000000000000000, 0.000000000000000000, 0.000000000000000000 ) ) ;
#21753 = CARTESIAN_POINT ( 'NONE',  ( -3.175426480542816510, 5.499999999999865885, -167.8750000000000568 ) ) ;
#21754 = DIRECTION ( 'NONE',  ( -1.000000000000000000, -1.665334536937736783E-16, -2.220446049250315546E-16 ) ) ;
#21755 = CARTESIAN_POINT ( 'NONE',  ( 111.2738248654049897, -1.999999999999881650, -0.8284271247459350507 ) ) ;
#21756 = CARTESIAN_POINT ( 'NONE',  ( 135.0029060396470300, -6.966976446535451117, 8.000000000000007105 ) ) ;
#21757 = CARTESIAN_POINT ( 'NONE',  ( -6.350852961085760029, -1.281975124255709124E-13, -164.6249999999999716 ) ) ;
#21758 = CARTESIAN_POINT ( 'NONE',  ( 160.5074251345948255, 2.278174593052136210, -5.499999999999888978 ) ) ;
#21759 = CARTESIAN_POINT ( 'NONE',  ( -4.763139720814407951, -2.750000000000016431, -146.5000000000000284 ) ) ;
#21760 = CARTESIAN_POINT ( 'NONE',  ( -4.999999999999990230, -55.00000000000002132, -7.500000000000007105 ) ) ;
#21761 = CARTESIAN_POINT ( 'NONE',  ( -4.763139720814407951, 2.749999999999946709, -92.75000000000000000 ) ) ;
#21762 = CARTESIAN_POINT ( 'NONE',  ( -5.999999999999963585, 9.296355089585909904E-15, -168.8363248654052029 ) ) ;
#21763 = CARTESIAN_POINT ( 'NONE',  ( -2.775557561562891351E-14, -5.500000000000115463, -87.75000000000000000 ) ) ;
#21764 = PRODUCT_DEFINITION_FORMATION_WITH_SPECIFIED_SOURCE ( 'ANY', '', #10914, .NOT_KNOWN. ) ;
#21765 = CARTESIAN_POINT ( 'NONE',  ( 155.9136751345948539, 0.000000000000000000, -5.500000000000005329 ) ) ;
#21766 = CYLINDRICAL_SURFACE ( 'NONE', #12611, 6.000000000000000888 ) ;
#21767 = CARTESIAN_POINT ( 'NONE',  ( 109.8124999999997868, 1.035533905932779275, -2.499999999999784173 ) ) ;
#21768 = LINE ( 'NONE', #28798, #2133 ) ;
#21769 = CARTESIAN_POINT ( 'NONE',  ( 3.464101615137757051, -5.999999999999979572, -73.83632486540521711 ) ) ;
#21770 = DIRECTION ( 'NONE',  ( -1.000000000000000000, -1.665334536937731113E-16, 1.526556658859586792E-16 ) ) ;
#21771 = ORIENTED_EDGE ( 'NONE', *, *, #28023, .T. ) ;
#21772 = CARTESIAN_POINT ( 'NONE',  ( 6.000000000000000888, 1.743066579297358182E-13, -83.16367513459481131 ) ) ;
#21773 = CARTESIAN_POINT ( 'NONE',  ( 121.3127832217621034, 1.849990392679682127, -0.7662911109075883909 ) ) ;
#21774 = CARTESIAN_POINT ( 'NONE',  ( 110.8988248654050182, 0.8284271247462654530, 2.000000000000271783 ) ) ;
#21775 = ORIENTED_EDGE ( 'NONE', *, *, #27158, .T. ) ;
#21776 =( BOUNDED_CURVE ( )  B_SPLINE_CURVE ( 2, ( #13953, #14106, #6983, #70, #18688, #11640, #18384, #30026, #15946 ),
 .UNSPECIFIED., .F., .T. ) 
 B_SPLINE_CURVE_WITH_KNOTS ( ( 3, 2, 2, 2, 3 ),
 ( 0.5027777777777777679, 0.5037037037037037646, 0.5055555555555555358, 0.5074074074074074181, 0.5083333333333333037 ),
 .UNSPECIFIED. ) 
 CURVE ( )  GEOMETRIC_REPRESENTATION_ITEM ( )  RATIONAL_B_SPLINE_CURVE ( ( 0.9330127018922194093, 0.9330127018922194093, 1.000000000000000000, 0.8660254037844388186, 1.000000000000000000, 0.8660254037844388186, 1.000000000000000000, 0.9330127018922234061, 0.9330127018922194093 ) ) 
 REPRESENTATION_ITEM ( '' )  );
#21777 = EDGE_CURVE ( 'NONE', #17671, #14644, #20293, .T. ) ;
#21778 = EDGE_LOOP ( 'NONE', ( #28960, #17977, #11845, #30197, #7953, #27988, #19667, #20730, #28428, #26395, #28837, #7253, #1822, #21632, #23004, #12326, #23409, #29543, #7883, #1041, #19921, #29179, #11528, #4541, #7438, #10811, #23076, #24358, #16454, #9231, #1519, #19244, #15691, #14263, #29140, #21029, #26071, #27611, #29506, #8034, #6695, #8289, #16145, #26883, #16639, #15183, #26747, #22804, #29253, #23897, #29762, #3008, #28065, #2754, #27186, #13693, #7235, #5415, #30348, #20942, #12250, #20196, #14295, #2097, #4739, #27346, #30121, #13421, #23815, #3839, #7875, #27896, #21342, #16276, #4231, #15983, #22768, #29187, #1383, #17073, #15659, #24751, #21375, #28176, #5761, #17520, #3275, #26179, #11835, #451, #23653, #9795, #7334, #1543, #9204, #12112, #13343, #27224, #30384, #28622, #28207, #13523, #13169, #6463, #10792, #27113, #18474, #16269, #22993, #10107, #23184, #1816, #6449, #9516, #10365, #4456, #11874, #11383, #21498, #19723, #19400, #20454, #7762, #15965, #20149, #29642, #4616, #4110, #7451, #3048, #12167, #30159, #24507, #6203, #859, #18283, #23272, #10510, #23309, #11286, #23029, #24548, #8704, #19915, #6244, #10985, #16034, #14614, #15062, #301, #20920, #15167, #19515, #2173, #14842, #13930, #19958, #27217, #16627, #2471, #18545, #6275, #13819, #16184, #19658, #26241, #10287, #13491, #18129, #11886, #5509, #1880, #26097, #7814, #4314, #25649, #22872, #15782, #1420, #6169, #13056, #24932 ) ) ;
#21779 = CARTESIAN_POINT ( 'NONE',  ( 145.6875000000000284, 4.242640687119269671, 4.242640687119298093 ) ) ;
#21780 = ORIENTED_EDGE ( 'NONE', *, *, #16577, .T. ) ;
#21781 = CARTESIAN_POINT ( 'NONE',  ( 3.175426480543072749, -5.500000000000105693, -102.6250000000000000 ) ) ;
#21782 = CARTESIAN_POINT ( 'NONE',  ( 20.25000000000009948, 1.873492889145067508, -1.873492889144956486 ) ) ;
#21783 = CARTESIAN_POINT ( 'NONE',  ( 2.775557561562891351E-14, 6.250000000000033751, -124.9330127018922809 ) ) ;
#21784 = ORIENTED_EDGE ( 'NONE', *, *, #20711, .T. ) ;
#21785 = CARTESIAN_POINT ( 'NONE',  ( 0.000000000000000000, 5.999999999999977796, -111.2886751345948397 ) ) ;
#21786 = CARTESIAN_POINT ( 'NONE',  ( 5.412658773652712085, -3.125000000000086153, -159.0669872981078754 ) ) ;
#21787 = CARTESIAN_POINT ( 'NONE',  ( 106.3124999999997584, -1.035533905932659149, 2.500000000000205169 ) ) ;
#21788 = CARTESIAN_POINT ( 'NONE',  ( 3.608439182435180470, -6.249999999999997335, -58.05801270189221697 ) ) ;
#21789 = VERTEX_POINT ( 'NONE', #26716 ) ;
#21790 = LINE ( 'NONE', #28972, #15739 ) ;
#21791 = DIRECTION ( 'NONE',  ( -1.000000000000000000, 0.000000000000000000, 0.000000000000000000 ) ) ;
#21792 = CARTESIAN_POINT ( 'NONE',  ( 141.2738248654052313, -3.889087296526011706, 3.889087296526011706 ) ) ;
#21793 = CARTESIAN_POINT ( 'NONE',  ( 3.175426480543072749, -5.500000000000105693, -180.6250000000000284 ) ) ;
#21794 = CARTESIAN_POINT ( 'NONE',  ( 104.8752832217621602, -1.849990392679495832, 2.220446049250313081E-13 ) ) ;
#21795 = CARTESIAN_POINT ( 'NONE',  ( 2.775557561562891351E-14, 6.250000000000033751, -166.9330127018922099 ) ) ;
#21796 = B_SPLINE_CURVE_WITH_KNOTS ( 'NONE', 3,
 ( #15820, #27419, #6704, #11349, #6386, #29592, #30202, #4083 ),
 .UNSPECIFIED., .F., .F.,
 ( 4, 2, 2, 4 ),
 ( 0.000000000000000000, 0.0002342670595278595010, 0.0003514005892917859177, 0.0004685341190557123343 ),
 .UNSPECIFIED. ) ;
#21797 = CARTESIAN_POINT ( 'NONE',  ( 119.3511751345946550, 2.000000000000061728, 0.8284271247463557142 ) ) ;
#21798 = CARTESIAN_POINT ( 'NONE',  ( 23.25000000000004974, 5.551115123125782702E-14, 1.999999999999946265 ) ) ;
#21799 = CARTESIAN_POINT ( 'NONE',  ( 0.000000000000000000, 5.499999999999991118, -113.9999999999999858 ) ) ;
#21800 = DIRECTION ( 'NONE',  ( 5.551115123125785167E-17, -1.000000000000000000, -8.881784197001256268E-16 ) ) ;
#21801 = CARTESIAN_POINT ( 'NONE',  ( 3.175426480543072749, -5.500000000000105693, -116.1250000000000000 ) ) ;
#21802 = CARTESIAN_POINT ( 'NONE',  ( 1.000000000000000888, -16.43939393939394833, -5.999693900976793337 ) ) ;
#21803 = CARTESIAN_POINT ( 'NONE',  ( 148.9761751345948255, 3.889087296526011706, 3.889087296526011706 ) ) ;
#21804 = ORIENTED_EDGE ( 'NONE', *, *, #8869, .F. ) ;
#21805 = EDGE_CURVE ( 'NONE', #452, #30157, #28115, .T. ) ;
#21806 = CARTESIAN_POINT ( 'NONE',  ( 120.8124999999997726, 1.035533905932899401, -2.499999999999844569 ) ) ;
#21807 = CARTESIAN_POINT ( 'NONE',  ( 15.00000000000000000, 0.000000000000000000, -16.50000000000000355 ) ) ;
#21808 = VERTEX_POINT ( 'NONE', #12350 ) ;
#21809 = CARTESIAN_POINT ( 'NONE',  ( 111.6636751345947829, -1.414213562373090038, 1.414213562373034527 ) ) ;
#21810 = DIRECTION ( 'NONE',  ( 0.000000000000000000, 0.000000000000000000, -1.000000000000000000 ) ) ;
#21811 = CARTESIAN_POINT ( 'NONE',  ( 6.000000000000000888, 1.607695154586715303, -110.0966878364870638 ) ) ;
#21812 = VERTEX_POINT ( 'NONE', #1085 ) ;
#21813 = CARTESIAN_POINT ( 'NONE',  ( 24.82006884940611613, 1.953411417485240831, -0.9991708543551893751 ) ) ;
#21814 = EDGE_CURVE ( 'NONE', #3203, #20658, #21119, .T. ) ;
#21815 = ORIENTED_EDGE ( 'NONE', *, *, #27470, .T. ) ;
#21816 = EDGE_LOOP ( 'NONE', ( #11194, #11142, #15931, #4681 ) ) ;
#21817 = CARTESIAN_POINT ( 'NONE',  ( 132.4687500000000284, -2.485281374238585972, 6.000000000000005329 ) ) ;
#21818 = CARTESIAN_POINT ( 'NONE',  ( 160.0312500000000284, -2.485281374238555774, -6.000000000000005329 ) ) ;
#21819 = CARTESIAN_POINT ( 'NONE',  ( 11.00000000000014921, 2.000000000000112799, 0.000000000000000000 ) ) ;
#21820 = ORIENTED_EDGE ( 'NONE', *, *, #27221, .T. ) ;
#21821 = CARTESIAN_POINT ( 'NONE',  ( 157.2113248654052313, 5.500000000000005329, 0.000000000000000000 ) ) ;
#21822 = CARTESIAN_POINT ( 'NONE',  ( -7.216878364870328078, 0.000000000000000000, -134.1919872981078754 ) ) ;
#21823 = PRESENTATION_STYLE_ASSIGNMENT (( #10453 ) ) ;
#21824 = CARTESIAN_POINT ( 'NONE',  ( -3.464101615137725076, 5.999999999999979572, -49.66367513459484684 ) ) ;
#21825 = CARTESIAN_POINT ( 'NONE',  ( 144.4761751345948255, 3.889087296526011706, 3.889087296526011706 ) ) ;
#21826 = ORIENTED_EDGE ( 'NONE', *, *, #436, .F. ) ;
#21827 = CARTESIAN_POINT ( 'NONE',  ( 14.56249999999998934, -1.999999999999851674, -0.8284271247462354770 ) ) ;
#21828 = CARTESIAN_POINT ( 'NONE',  ( -6.000000000000000888, 1.067854986875958443E-15, 7.560779664488942560E-35 ) ) ;
#21829 = CARTESIAN_POINT ( 'NONE',  ( -19.99999999999998224, -54.99999999999990763, 5.000000000000004441 ) ) ;
#21830 = CARTESIAN_POINT ( 'NONE',  ( 137.1413997308104342, 2.071067811865468400, -4.999999999999989342 ) ) ;
#21831 = CARTESIAN_POINT ( 'NONE',  ( 138.0863248654052313, 0.000000000000000000, 5.500000000000005329 ) ) ;
#21832 = CARTESIAN_POINT ( 'NONE',  ( 15.35117513459492677, 2.500000000000144773, 1.035533905932689347 ) ) ;
#21833 = CARTESIAN_POINT ( 'NONE',  ( -4.999999999999886313, -15.00000000000001421, -7.500000000000007105 ) ) ;
#21834 = FACE_OUTER_BOUND ( 'NONE', #4601, .T. ) ;
#21835 = CARTESIAN_POINT ( 'NONE',  ( 105.8749999999999574, 1.767766952966320915, -1.767766952966320915 ) ) ;
#21836 = CARTESIAN_POINT ( 'NONE',  ( -5.999999999999963585, -1.487416814333745711E-14, -122.3363248654052029 ) ) ;
#21837 = CARTESIAN_POINT ( 'NONE',  ( 4.763139720814407951, -2.749999999999988454, -135.5000000000000000 ) ) ;
#21838 = FACE_OUTER_BOUND ( 'NONE', #19962, .T. ) ;
#21839 = ORIENTED_EDGE ( 'NONE', *, *, #22013, .F. ) ;
#21840 = EDGE_CURVE ( 'NONE', #25123, #10004, #5530, .T. ) ;
#21841 = CARTESIAN_POINT ( 'NONE',  ( 4.763139720814407951, -2.749999999999988454, -47.00000000000004263 ) ) ;
#21842 = CARTESIAN_POINT ( 'NONE',  ( -10.00000000000000178, -19.99999999999998934, 4.000000000000003553 ) ) ;
#21843 = ORIENTED_EDGE ( 'NONE', *, *, #17359, .F. ) ;
#21844 = CARTESIAN_POINT ( 'NONE',  ( 118.8747167782375840, 5.551115123125782702E-14, 1.849990392679523588 ) ) ;
#21845 = CARTESIAN_POINT ( 'NONE',  ( 118.6636751345946550, -1.414213562373117794, 1.414213562373256572 ) ) ;
#21846 = CARTESIAN_POINT ( 'NONE',  ( 3.608439182435180470, -6.249999999999997335, -97.69198729810781856 ) ) ;
#21847 = CONICAL_SURFACE ( 'NONE', #25770, 577.3502691896271699, 0.5235987755982998149 ) ;
#21848 = CARTESIAN_POINT ( 'NONE',  ( 6.000000000000052403, -1.607695154586662678, -78.15331216351297883 ) ) ;
#21849 = ADVANCED_FACE ( 'NONE', ( #3373 ), #10322, .T. ) ;
#21850 = DIRECTION ( 'NONE',  ( 0.000000000000000000, 0.000000000000000000, -1.000000000000000000 ) ) ;
#21851 = CARTESIAN_POINT ( 'NONE',  ( 114.7499999999999147, -5.551115123125782702E-14, -2.499999999999946709 ) ) ;
#21852 = CARTESIAN_POINT ( 'NONE',  ( 140.8531441848278689, -11.85314418482570353, 4.000138456839522405 ) ) ;
#21853 = CARTESIAN_POINT ( 'NONE',  ( 3.175426480543072749, 5.499999999999865885, -130.6250000000000284 ) ) ;
#21854 = ORIENTED_EDGE ( 'NONE', *, *, #7678, .F. ) ;
#21855 = CARTESIAN_POINT ( 'NONE',  ( 160.8911125001014284, -11.51406693544466009, 3.382303552187507112 ) ) ;
#21856 = AXIS2_PLACEMENT_3D ( 'NONE', #27869, #23450, #22987 ) ;
#21857 = CARTESIAN_POINT ( 'NONE',  ( 4.763139720814407951, 2.750000000000002665, -54.25000000000002132 ) ) ;
#21858 = CARTESIAN_POINT ( 'NONE',  ( 6.000000000000000888, 1.743066579297358182E-13, -69.66367513459481131 ) ) ;
#21859 = DIRECTION ( 'NONE',  ( 1.000000000000000000, -5.551115123125773458E-17, -1.260129944081490338E-35 ) ) ;
#21860 = CARTESIAN_POINT ( 'NONE',  ( 2.693961096941849487, 10.67153403684353385, -19.62422301979503203 ) ) ;
#21861 =( BOUNDED_CURVE ( )  B_SPLINE_CURVE ( 2, ( #1226, #7543, #16953, #14789, #23988, #17100, #24134, #26281, #14643 ),
 .UNSPECIFIED., .F., .T. ) 
 B_SPLINE_CURVE_WITH_KNOTS ( ( 3, 2, 2, 2, 3 ),
 ( 0.7647058823529411242, 0.7720588235294117974, 0.7794117647058823595, 0.7867647058823529216, 0.7941176470588234837 ),
 .UNSPECIFIED. ) 
 CURVE ( )  GEOMETRIC_REPRESENTATION_ITEM ( )  RATIONAL_B_SPLINE_CURVE ( ( 1.000000000000000000, 0.9238795325112867385, 1.000000000000000000, 0.9238795325112867385, 1.000000000000000000, 0.9238795325112867385, 1.000000000000000000, 0.9238795325112867385, 1.000000000000000000 ) ) 
 REPRESENTATION_ITEM ( '' )  );
#21862 = CARTESIAN_POINT ( 'NONE',  ( 3.608439182435180470, -6.249999999999997335, -79.05801270189225249 ) ) ;
#21863 = CARTESIAN_POINT ( 'NONE',  ( 116.3988248654050039, -0.8284271247460852639, -1.999999999999911626 ) ) ;
#21864 = LINE ( 'NONE', #26449, #54 ) ;
#21865 = CARTESIAN_POINT ( 'NONE',  ( 104.1247167782375556, -1.849990392679468076, 0.000000000000000000 ) ) ;
#21866 =( LENGTH_UNIT ( ) NAMED_UNIT ( * ) SI_UNIT ( .MILLI., .METRE. ) );
#21867 = CARTESIAN_POINT ( 'NONE',  ( -5.196152422706601826, 2.999999999999975131, -60.96132486540523132 ) ) ;
#21868 = CARTESIAN_POINT ( 'NONE',  ( 114.1252832217622313, -8.326672684688674053E-14, -1.849990392679412565 ) ) ;
#21869 =( BOUNDED_CURVE ( )  B_SPLINE_CURVE ( 2, ( #11426, #27643, #18031, #27487, #29508, #4315, #20158, #22917, #11263 ),
 .UNSPECIFIED., .F., .T. ) 
 B_SPLINE_CURVE_WITH_KNOTS ( ( 3, 2, 2, 2, 3 ),
 ( 0.1718750000000000000, 0.1796875000000000000, 0.1875000000000000000, 0.1953125000000000000, 0.2031250000000000000 ),
 .UNSPECIFIED. ) 
 CURVE ( )  GEOMETRIC_REPRESENTATION_ITEM ( )  RATIONAL_B_SPLINE_CURVE ( ( 1.000000000000000000, 0.9238795325112867385, 1.000000000000000000, 0.9238795325112867385, 1.000000000000000000, 0.9238795325112867385, 1.000000000000000000, 0.9238795325112867385, 1.000000000000000000 ) ) 
 REPRESENTATION_ITEM ( '' )  );
#21870 = CARTESIAN_POINT ( 'NONE',  ( -4.763139720814407951, -2.750000000000016431, -139.0000000000000000 ) ) ;
#21871 = CARTESIAN_POINT ( 'NONE',  ( 140.0000000000000000, -9.910236803014807805, 7.559842130755045631 ) ) ;
#21872 = CARTESIAN_POINT ( 'NONE',  ( 3.608439182435180470, -6.249999999999997335, -154.0580127018922099 ) ) ;
#21873 = FACE_OUTER_BOUND ( 'NONE', #1885, .T. ) ;
#21874 = EDGE_CURVE ( 'NONE', #21808, #5958, #28721, .T. ) ;
#21875 = CARTESIAN_POINT ( 'NONE',  ( 3.175426480543072749, 5.499999999999865885, -70.62500000000004263 ) ) ;
#21876 = CARTESIAN_POINT ( 'NONE',  ( -3.175426480542816510, 5.499999999999865885, -61.37500000000000000 ) ) ;
#21877 = DIRECTION ( 'NONE',  ( 1.000000000000000000, -0.000000000000000000, -0.000000000000000000 ) ) ;
#21878 = ORIENTED_EDGE ( 'NONE', *, *, #5752, .T. ) ;
#21879 = CARTESIAN_POINT ( 'NONE',  ( 139.0461002691896510, -2.071067811865468400, 4.999999999999989342 ) ) ;
#21880 = CARTESIAN_POINT ( 'NONE',  ( 152.0625000000000568, -4.242640687119298093, 4.242640687119298093 ) ) ;
#21881 = CARTESIAN_POINT ( 'NONE',  ( -5.196152422706601826, 2.999999999999975131, -97.53867513459479710 ) ) ;
#21882 = CIRCLE ( 'NONE', #10138, 1.999999999999998224 ) ;
#21883 = CARTESIAN_POINT ( 'NONE',  ( 0.000000000000000000, 0.000000000000000000, 0.000000000000000000 ) ) ;
#21884 = EDGE_CURVE ( 'NONE', #23373, #3569, #5325, .T. ) ;
#21885 = EDGE_CURVE ( 'NONE', #29510, #17448, #21861, .T. ) ;
#21886 = EDGE_LOOP ( 'NONE', ( #11678, #28971, #15735 ) ) ;
#21887 = CARTESIAN_POINT ( 'NONE',  ( 144.1875000000000284, 4.242640687119269671, 4.242640687119298093 ) ) ;
#21888 = CARTESIAN_POINT ( 'NONE',  ( 6.000000000000000888, 1.743066579297358182E-13, -71.16367513459481131 ) ) ;
#21889 = CARTESIAN_POINT ( 'NONE',  ( 104.8513327624231408, 0.7142157997211321385, 1.784475575595019459 ) ) ;
#21890 = CARTESIAN_POINT ( 'NONE',  ( 6.350852961086080661, -9.614813431917819062E-14, -175.8750000000000284 ) ) ;
#21891 = CARTESIAN_POINT ( 'NONE',  ( 17.25000000000001421, 1.665334536937734811E-13, 2.000000000000001776 ) ) ;
#21892 = ORIENTED_EDGE ( 'NONE', *, *, #27707, .F. ) ;
#21893 = CARTESIAN_POINT ( 'NONE',  ( 2.775557561562891351E-14, 6.250000000000033751, -152.5669872981077901 ) ) ;
#21894 = ORIENTED_EDGE ( 'NONE', *, *, #9688, .T. ) ;
#21895 = CARTESIAN_POINT ( 'NONE',  ( 4.763139720814407951, 2.750000000000002665, -81.25000000000004263 ) ) ;
#21896 = CARTESIAN_POINT ( 'NONE',  ( 15.56250000000015810, 1.097466725451679892, 2.649519052838298805 ) ) ;
#21897 = CIRCLE ( 'NONE', #18983, 12.00000000000000178 ) ;
#21898 = CARTESIAN_POINT ( 'NONE',  ( -3.608439182435052128, -6.250000000000110134, -103.3080127018922383 ) ) ;
#21899 = COLOUR_RGB ( '', 0.66274510, 0.83137255, 0.94901961) ;
#21900 = VERTEX_POINT ( 'NONE', #3079 ) ;
#21901 = CARTESIAN_POINT ( 'NONE',  ( 119.9999999999998437, 2.090674230939232547, 1.116850201264615761 ) ) ;
#21902 = VECTOR ( 'NONE', #12422, 1000.000000000000000 ) ;
#21903 = CARTESIAN_POINT ( 'NONE',  ( 2.686045755586594197, -10.67338275482132204, -19.62059632520456276 ) ) ;
#21904 = CYLINDRICAL_SURFACE ( 'NONE', #14273, 1.000000000000000000 ) ;
#21905 =( LENGTH_UNIT ( ) NAMED_UNIT ( * ) SI_UNIT ( .MILLI., .METRE. ) );
#21906 = CARTESIAN_POINT ( 'NONE',  ( -2.775557561562891351E-14, -5.500000000000115463, -167.2500000000000000 ) ) ;
#21907 = CARTESIAN_POINT ( 'NONE',  ( -3.175426480542816510, -5.500000000000057732, -150.8750000000000000 ) ) ;
#21908 = DIRECTION ( 'NONE',  ( 1.000000000000000000, -5.551115123125773458E-17, -1.260129944081490338E-35 ) ) ;
#21909 = EDGE_CURVE ( 'NONE', #2895, #25883, #27118, .T. ) ;
#21910 = CARTESIAN_POINT ( 'NONE',  ( 4.763139720814407951, -2.749999999999988454, -92.00000000000002842 ) ) ;
#21911 = CARTESIAN_POINT ( 'NONE',  ( 0.000000000000000000, 0.000000000000000000, 0.000000000000000000 ) ) ;
#21912 = ADVANCED_FACE ( 'NONE', ( #6565 ), #16443, .T. ) ;
#21913 = CARTESIAN_POINT ( 'NONE',  ( 3.175426480543072749, 5.499999999999865885, -78.12500000000001421 ) ) ;
#21914 = DIRECTION ( 'NONE',  ( 1.000000000000000000, -5.551115123125773458E-17, -1.260129944081490338E-35 ) ) ;
#21915 = CARTESIAN_POINT ( 'NONE',  ( 106.9136751345946692, -1.414213562373034527, -1.414213562372812483 ) ) ;
#21916 = CARTESIAN_POINT ( 'NONE',  ( 108.0624999999998010, 2.500000000000114575, 1.035533905932929599 ) ) ;
#21917 = DIRECTION ( 'NONE',  ( -0.000000000000000000, -0.000000000000000000, -1.000000000000000000 ) ) ;
#21918 =( LENGTH_UNIT ( ) NAMED_UNIT ( * ) SI_UNIT ( .MILLI., .METRE. ) );
#21919 = EDGE_CURVE ( 'NONE', #6626, #30104, #24671, .T. ) ;
#21920 = VERTEX_POINT ( 'NONE', #7026 ) ;
#21921 = FILL_AREA_STYLE_COLOUR ( '', #5724 ) ;
#21922 = FACE_BOUND ( 'NONE', #16640, .T. ) ;
#21923 = CARTESIAN_POINT ( 'NONE',  ( -3.464101615137725076, 5.999999999999979572, -80.58632486540516027 ) ) ;
#21924 = CARTESIAN_POINT ( 'NONE',  ( 119.0002832217622455, -1.308140751793585022, -1.308140751793529510 ) ) ;
#21925 = VERTEX_POINT ( 'NONE', #27031 ) ;
#21926 = CARTESIAN_POINT ( 'NONE',  ( 147.5625000000000284, -4.242640687119298093, 4.242640687119298093 ) ) ;
#21927 = ORIENTED_EDGE ( 'NONE', *, *, #9674, .F. ) ;
#21928 = CARTESIAN_POINT ( 'NONE',  ( -6.350852961085760029, -1.281975124255709124E-13, -107.6250000000000426 ) ) ;
#21929 = CARTESIAN_POINT ( 'NONE',  ( 7.216878364870455975, -6.409875621278545621E-14, -126.8080127018922383 ) ) ;
#21930 = CARTESIAN_POINT ( 'NONE',  ( 6.000000000000052403, -1.607695154586662678, -60.73066243270260856 ) ) ;
#21931 = CARTESIAN_POINT ( 'NONE',  ( 3.608439182435180470, 6.249999999999982236, -160.1919872981078470 ) ) ;
#21932 = CARTESIAN_POINT ( 'NONE',  ( 106.1874999999999289, 1.035533905932839449, 2.500000000000265121 ) ) ;
#21933 = CARTESIAN_POINT ( 'NONE',  ( 146.9136751345948539, 0.000000000000000000, -5.500000000000005329 ) ) ;
#21934 = CARTESIAN_POINT ( 'NONE',  ( 5.412658773652712085, -3.125000000000086153, -56.43301270189227381 ) ) ;
#21935 = ORIENTED_EDGE ( 'NONE', *, *, #18895, .F. ) ;
#21936 = DIRECTION ( 'NONE',  ( -1.000000000000000000, 0.000000000000000000, 0.000000000000000000 ) ) ;
#21937 = CARTESIAN_POINT ( 'NONE',  ( -1.580833713216677205, 10.88751498504595361, -19.20858708930976988 ) ) ;
#21938 = CARTESIAN_POINT ( 'NONE',  ( 5.196152422706629359, 3.000000000000002665, -137.9613248654052313 ) ) ;
#21939 = CIRCLE ( 'NONE', #23915, 1.000000000000000000 ) ;
#21940 = CARTESIAN_POINT ( 'NONE',  ( 6.350852961086080661, -9.614813431917819062E-14, -172.8750000000000284 ) ) ;
#21941 = CARTESIAN_POINT ( 'NONE',  ( 105.8127832217621176, -1.849990392679501827, 0.7662911109077686911 ) ) ;
#21942 = CARTESIAN_POINT ( 'NONE',  ( 152.9925748654052029, 2.278174593051965235, 5.500000000000058620 ) ) ;
#21943 = CARTESIAN_POINT ( 'NONE',  ( -5.412658773652684552, -3.125000000000099920, -167.9330127018922099 ) ) ;
#21944 = DIRECTION ( 'NONE',  ( 0.000000000000000000, 0.000000000000000000, 1.000000000000000000 ) ) ;
#21945 = LINE ( 'NONE', #8089, #12359 ) ;
#21946 = EDGE_CURVE ( 'NONE', #11887, #28765, #25153, .T. ) ;
#21947 = CARTESIAN_POINT ( 'NONE',  ( -3.175426480542816066, 5.499999999999865885, -115.3750000000000000 ) ) ;
#21948 = CARTESIAN_POINT ( 'NONE',  ( 135.9026099654455493, -8.798545334315235777, 8.160000000000003695 ) ) ;
#21949 = EDGE_CURVE ( 'NONE', #25259, #29296, #21024, .T. ) ;
#21950 = CARTESIAN_POINT ( 'NONE',  ( -6.350852961085760029, -1.281975124255709124E-13, -107.6250000000000426 ) ) ;
#21951 = VECTOR ( 'NONE', #1285, 1000.000000000000000 ) ;
#21952 = CARTESIAN_POINT ( 'NONE',  ( 6.000000000000000888, -1.859271017917181981E-14, -101.1636751345948397 ) ) ;
#21953 = ORIENTED_EDGE ( 'NONE', *, *, #9361, .F. ) ;
#21954 = CARTESIAN_POINT ( 'NONE',  ( 120.0624999999998721, 2.500000000000114575, 1.035533905932869425 ) ) ;
#21955 = CARTESIAN_POINT ( 'NONE',  ( 6.000000000000000888, 1.743066579297358182E-13, -75.66367513459485394 ) ) ;
#21956 =( BOUNDED_CURVE ( )  B_SPLINE_CURVE ( 2, ( #19818, #781, #24261, #17541, #7826, #19387, #17242, #24125, #19238 ),
 .UNSPECIFIED., .F., .T. ) 
 B_SPLINE_CURVE_WITH_KNOTS ( ( 3, 2, 2, 2, 3 ),
 ( 0.8583333333333332815, 0.8592592592592592782, 0.8611111111111111605, 0.8629629629629629317, 0.8638888888888889284 ),
 .UNSPECIFIED. ) 
 CURVE ( )  GEOMETRIC_REPRESENTATION_ITEM ( )  RATIONAL_B_SPLINE_CURVE ( ( 0.9330127018922194093, 0.9330127018922154125, 1.000000000000000000, 0.8660254037844388186, 1.000000000000000000, 0.8660254037844388186, 1.000000000000000000, 0.9330127018922154125, 0.9330127018922194093 ) ) 
 REPRESENTATION_ITEM ( '' )  );
#21957 = CARTESIAN_POINT ( 'NONE',  ( -5.999999999999919176, 1.607695154586804565, -86.40331216351303567 ) ) ;
#21958 = ORIENTED_EDGE ( 'NONE', *, *, #6887, .F. ) ;
#21959 = CARTESIAN_POINT ( 'NONE',  ( -7.216878364870328078, 0.000000000000000000, -78.69198729810784698 ) ) ;
#21960 =( NAMED_UNIT ( * ) SI_UNIT ( $, .STERADIAN. ) SOLID_ANGLE_UNIT ( ) );
#21961 = VERTEX_POINT ( 'NONE', #1966 ) ;
#21962 = CARTESIAN_POINT ( 'NONE',  ( 6.000000000000000888, -3.330669073875464691E-16, -7.560779664488942560E-35 ) ) ;
#21963 = VECTOR ( 'NONE', #29844, 1000.000000000000000 ) ;
#21964 = VERTEX_POINT ( 'NONE', #29336 ) ;
#21965 = CARTESIAN_POINT ( 'NONE',  ( 134.2648502691896510, 3.535533905932725318, 3.535533905932752852 ) ) ;
#21966 = ORIENTED_EDGE ( 'NONE', *, *, #9332, .T. ) ;
#21967 = CARTESIAN_POINT ( 'NONE',  ( 2.775557561562891351E-14, -6.250000000000061284, -132.3169872981078186 ) ) ;
#21968 =( NAMED_UNIT ( * ) PLANE_ANGLE_UNIT ( ) SI_UNIT ( $, .RADIAN. ) );
#21969 = CARTESIAN_POINT ( 'NONE',  ( 0.000000000000000000, 5.999999999999977796, -83.71132486540521711 ) ) ;
#21970 = CARTESIAN_POINT ( 'NONE',  ( 6.000000000000000888, -1.859271017917181981E-14, -116.1636751345948255 ) ) ;
#21971 = AXIS2_PLACEMENT_3D ( 'NONE', #9442, #11777, #11150 ) ;
#21972 = ORIENTED_EDGE ( 'NONE', *, *, #3756, .F. ) ;
#21973 = CARTESIAN_POINT ( 'NONE',  ( 16.25000000000009948, 1.665334536937734811E-13, 2.000000000000001776 ) ) ;
#21974 = CARTESIAN_POINT ( 'NONE',  ( -5.999999999999963585, -1.487416814333745711E-14, -134.9136751345948255 ) ) ;
#21975 = CARTESIAN_POINT ( 'NONE',  ( 5.196152422706629359, -2.999999999999988898, -138.7886751345947971 ) ) ;
#21976 = FILL_AREA_STYLE_COLOUR ( '', #14262 ) ;
#21977 = CARTESIAN_POINT ( 'NONE',  ( 136.9538997308104058, -2.071067811865468400, -4.999999999999989342 ) ) ;
#21978 = CARTESIAN_POINT ( 'NONE',  ( 3.464101615137757051, -5.999999999999979572, -46.83632486540521001 ) ) ;
#21979 = CARTESIAN_POINT ( 'NONE',  ( -5.412658773652684552, -3.125000000000099920, -69.56698729810784698 ) ) ;
#21980 = CARTESIAN_POINT ( 'NONE',  ( -3.464101615137757051, -5.999999999999979572, -64.16367513459478289 ) ) ;
#21981 = CARTESIAN_POINT ( 'NONE',  ( 105.9374999999997584, 2.500000000000144773, -1.035533905932568999 ) ) ;
#21982 = CARTESIAN_POINT ( 'NONE',  ( -5.999999999999971578, 1.607695154586715303, -127.4806624327025872 ) ) ;
#21983 = EDGE_CURVE ( 'NONE', #341, #20441, #26387, .T. ) ;
#21984 = CARTESIAN_POINT ( 'NONE',  ( 0.000000000000000000, 5.499999999999991118, -136.5000000000000000 ) ) ;
#21985 = CARTESIAN_POINT ( 'NONE',  ( 3.464101615137852974, 5.999999999999884537, -166.9136751345947971 ) ) ;
#21986 = ORIENTED_EDGE ( 'NONE', *, *, #27334, .T. ) ;
#21987 = CARTESIAN_POINT ( 'NONE',  ( 13.46132486540532724, 1.665334536937734811E-13, -2.500000000000057732 ) ) ;
#21988 = CARTESIAN_POINT ( 'NONE',  ( 3.175426480543072749, 5.499999999999865885, -46.62500000000006395 ) ) ;
#21989 = CARTESIAN_POINT ( 'NONE',  ( 6.000000000000000888, -1.607695154586752384, -159.7306624327026157 ) ) ;
#21990 = CARTESIAN_POINT ( 'NONE',  ( 112.5386751345946550, 8.326672684688674053E-14, 2.000000000000001776 ) ) ;
#21991 = ORIENTED_EDGE ( 'NONE', *, *, #18192, .F. ) ;
#21992 = CARTESIAN_POINT ( 'NONE',  ( 112.9997167782376835, -1.308140751793557266, 1.308140751793751555 ) ) ;
#21993 = CARTESIAN_POINT ( 'NONE',  ( -5.412658773652684552, -3.125000000000099920, -98.06698729810780435 ) ) ;
#21994 = CARTESIAN_POINT ( 'NONE',  ( 135.0000000000000284, 5.838252472155780914, -1.149616569750068207 ) ) ;
#21995 = CARTESIAN_POINT ( 'NONE',  ( 155.6324251345948255, -5.500000000000012434, -2.278174593052012309 ) ) ;
#21996 = CARTESIAN_POINT ( 'NONE',  ( 112.7499999999998579, -5.551115123125782702E-14, -2.499999999999946709 ) ) ;
#21997 = SURFACE_STYLE_USAGE ( .BOTH. , #22153 ) ;
#21998 = CARTESIAN_POINT ( 'NONE',  ( 141.0863248654052313, 0.000000000000000000, 5.500000000000005329 ) ) ;
#21999 = VERTEX_POINT ( 'NONE', #17706 ) ;
#22000 = EDGE_CURVE ( 'NONE', #15423, #17032, #25446, .T. ) ;
#22001 = CARTESIAN_POINT ( 'NONE',  ( 4.763139720814407951, 2.750000000000002665, -58.75000000000002132 ) ) ;
#22002 = CARTESIAN_POINT ( 'NONE',  ( -5.999999999999963585, 1.780251999655701777E-13, -68.91367513459482552 ) ) ;
#22003 = CARTESIAN_POINT ( 'NONE',  ( -5.999999999999963585, 1.780251999655701777E-13, -62.33632486540522422 ) ) ;
#22004 = CARTESIAN_POINT ( 'NONE',  ( 1.584453406822469601, 10.89233254831497177, -19.19936552286312903 ) ) ;
#22005 = CARTESIAN_POINT ( 'NONE',  ( -5.412658773652684552, -3.125000000000099920, -77.93301270189223828 ) ) ;
#22006 = CARTESIAN_POINT ( 'NONE',  ( 1.110223024625164183E-16, -2.000000000000012879, -1.776356839400262692E-15 ) ) ;
#22007 = CARTESIAN_POINT ( 'NONE',  ( 157.5788997308104058, -4.999999999999989342, 2.071067811865468400 ) ) ;
#22008 = FACE_OUTER_BOUND ( 'NONE', #18104, .T. ) ;
#22009 = CARTESIAN_POINT ( 'NONE',  ( -5.999999999999919176, 1.607695154586804565, -79.48066243270261566 ) ) ;
#22010 =( LENGTH_UNIT ( ) NAMED_UNIT ( * ) SI_UNIT ( .MILLI., .METRE. ) );
#22011 = CARTESIAN_POINT ( 'NONE',  ( -3.464101615137725076, 5.999999999999979572, -104.5863248654052029 ) ) ;
#22012 = EDGE_CURVE ( 'NONE', #20142, #27374, #11369, .T. ) ;
#22013 = EDGE_CURVE ( 'NONE', #1699, #25773, #12476, .T. ) ;
#22014 = CARTESIAN_POINT ( 'NONE',  ( 6.350852961086080661, -9.614813431917819062E-14, -138.3750000000000568 ) ) ;
#22015 = CARTESIAN_POINT ( 'NONE',  ( 3.464101615137852974, 5.999999999999884537, -68.83632486540518869 ) ) ;
#22016 = LINE ( 'NONE', #5408, #5668 ) ;
#22017 = CARTESIAN_POINT ( 'NONE',  ( 5.196152422706629359, 3.000000000000002665, -67.46132486540523132 ) ) ;
#22018 = CARTESIAN_POINT ( 'NONE',  ( 3.175426480543072749, 5.499999999999865885, -72.12500000000005684 ) ) ;
#22019 = CARTESIAN_POINT ( 'NONE',  ( 3.175426480543072749, 5.499999999999865885, -57.12500000000004974 ) ) ;
#22020 = ORIENTED_EDGE ( 'NONE', *, *, #20179, .T. ) ;
#22021 = CARTESIAN_POINT ( 'NONE',  ( 142.3273502691896510, -5.000000000000004441, 0.000000000000000000 ) ) ;
#22022 = CARTESIAN_POINT ( 'NONE',  ( 152.8125000000000568, 4.242640687119298093, -4.242640687119298093 ) ) ;
#22023 = CARTESIAN_POINT ( 'NONE',  ( 3.464101615137852974, 5.999999999999884537, -97.91367513459481131 ) ) ;
#22024 = CARTESIAN_POINT ( 'NONE',  ( 15.31250000000006928, -0.8284271247461753029, 1.999999999999911626 ) ) ;
#22025 = CARTESIAN_POINT ( 'NONE',  ( 115.2113248654050750, -1.999999999999918510, 1.110223024625156540E-13 ) ) ;
#22026 = CARTESIAN_POINT ( 'NONE',  ( 114.4372167782375271, 0.7662911109078588412, -1.849990392679351725 ) ) ;
#22027 = ORIENTED_EDGE ( 'NONE', *, *, #27221, .F. ) ;
#22028 = CARTESIAN_POINT ( 'NONE',  ( 141.2812500000000284, 2.485281374238585972, 6.000000000000005329 ) ) ;
#22029 = CARTESIAN_POINT ( 'NONE',  ( -5.999999999999963585, -1.487416814333745711E-14, -122.3363248654052029 ) ) ;
#22030 = CIRCLE ( 'NONE', #21093, 0.5000000000000004441 ) ;
#22031 =( BOUNDED_CURVE ( )  B_SPLINE_CURVE ( 2, ( #10699, #22514, #15147, #11005, #24479, #17922, #27239, #29231, #1601 ),
 .UNSPECIFIED., .F., .F. ) 
 B_SPLINE_CURVE_WITH_KNOTS ( ( 3, 2, 2, 2, 3 ),
 ( 0.4374999999999999445, 0.4437500000000001443, 0.4500000000000003997, 0.4562500000000006550, 0.4625000000000009104 ),
 .UNSPECIFIED. ) 
 CURVE ( )  GEOMETRIC_REPRESENTATION_ITEM ( )  RATIONAL_B_SPLINE_CURVE ( ( 1.000000000000000666, 0.9238795325112860723, 1.000000000000000000, 0.9238795325112867385, 1.000000000000000000, 0.9238795325112867385, 1.000000000000000000, 0.9238795325112759693, 1.000000000000010880 ) ) 
 REPRESENTATION_ITEM ( '' )  );
#22032 = CARTESIAN_POINT ( 'NONE',  ( 6.000000000000052403, -1.607695154586662678, -102.1533121635129646 ) ) ;
#22033 = AXIS2_PLACEMENT_3D ( 'NONE', #5339, #12460, #28835 ) ;
#22034 = CARTESIAN_POINT ( 'NONE',  ( 6.350852961086080661, -9.614813431917819062E-14, -177.3750000000000284 ) ) ;
#22035 = CARTESIAN_POINT ( 'NONE',  ( 17.87500000000008527, 1.414213562373312083, -1.414213562373145550 ) ) ;
#22036 = CARTESIAN_POINT ( 'NONE',  ( -7.216878364870328078, 0.000000000000000000, -150.6919872981077901 ) ) ;
#22037 = ORIENTED_EDGE ( 'NONE', *, *, #27810, .F. ) ;
#22038 = EDGE_CURVE ( 'NONE', #12351, #2749, #10477, .T. ) ;
#22039 = CARTESIAN_POINT ( 'NONE',  ( 4.763139720814407951, -2.749999999999988454, -84.50000000000001421 ) ) ;
#22040 = CARTESIAN_POINT ( 'NONE',  ( 3.608439182435180470, -6.249999999999997335, -94.05801270189226670 ) ) ;
#22041 =( BOUNDED_CURVE ( )  B_SPLINE_CURVE ( 2, ( #19508, #14329, #17065, #5345, #28390, #753, #26540, #10140, #26394 ),
 .UNSPECIFIED., .F., .T. ) 
 B_SPLINE_CURVE_WITH_KNOTS ( ( 3, 2, 2, 2, 3 ),
 ( 0.4638888888888889062, 0.4648148148148147918, 0.4666666666666666741, 0.4685185185185185563, 0.4694444444444444420 ),
 .UNSPECIFIED. ) 
 CURVE ( )  GEOMETRIC_REPRESENTATION_ITEM ( )  RATIONAL_B_SPLINE_CURVE ( ( 0.9330127018922194093, 0.9330127018922234061, 1.000000000000000000, 0.8660254037844388186, 1.000000000000000000, 0.8660254037844388186, 1.000000000000000000, 0.9330127018922194093, 0.9330127018922194093 ) ) 
 REPRESENTATION_ITEM ( '' )  );
#22042 = CARTESIAN_POINT ( 'NONE',  ( 119.9999999999999289, 2.500000000000057732, 1.110223024625156540E-13 ) ) ;
#22043 = SURFACE_SIDE_STYLE ('',( #12707 ) ) ;
#22044 = DIRECTION ( 'NONE',  ( 1.000000000000000000, 0.000000000000000000, 0.000000000000000000 ) ) ;
#22045 = CARTESIAN_POINT ( 'NONE',  ( 135.0710545211900353, -7.730464060720690256, -8.358520852376209120 ) ) ;
#22046 = CARTESIAN_POINT ( 'NONE',  ( 124.9999999999999432, -70.00000000000000000, -7.500000000000007105 ) ) ;
#22047 = ADVANCED_FACE ( 'NONE', ( #16296 ), #25617, .T. ) ;
#22048 =( NAMED_UNIT ( * ) SI_UNIT ( $, .STERADIAN. ) SOLID_ANGLE_UNIT ( ) );
#22049 = EDGE_CURVE ( 'NONE', #6232, #20568, #175, .T. ) ;
#22050 = CARTESIAN_POINT ( 'NONE',  ( 3.175426480543072749, 5.499999999999865885, -168.1250000000000000 ) ) ;
#22051 = CARTESIAN_POINT ( 'NONE',  ( 118.1488248654049613, -1.999999999999941602, 0.8284271247462955401 ) ) ;
#22052 = CARTESIAN_POINT ( 'NONE',  ( 6.350852961086080661, -9.614813431917819062E-14, -147.3750000000000284 ) ) ;
#22053 = CARTESIAN_POINT ( 'NONE',  ( 0.000000000000000000, 0.000000000000000000, 0.000000000000000000 ) ) ;
#22054 = AXIS2_PLACEMENT_3D ( 'NONE', #19157, #26627, #28493 ) ;
#22055 = CARTESIAN_POINT ( 'NONE',  ( -2.775557561562891351E-14, -5.500000000000115463, -95.25000000000000000 ) ) ;
#22056 = CARTESIAN_POINT ( 'NONE',  ( 141.9300748654051745, 2.278174593051702335, -5.500000000000323297 ) ) ;
#22057 = DIRECTION ( 'NONE',  ( -7.147005652999508048E-36, 5.642372883946980038E-36, 1.000000000000000000 ) ) ;
#22058 = CARTESIAN_POINT ( 'NONE',  ( 3.175426480543072749, -5.500000000000105693, -78.62500000000001421 ) ) ;
#22059 = AXIS2_PLACEMENT_3D ( 'NONE', #21383, #25974, #7243 ) ;
#22060 = CARTESIAN_POINT ( 'NONE',  ( 135.2738248654052313, -3.889087296526011706, 3.889087296526011706 ) ) ;
#22061 = CARTESIAN_POINT ( 'NONE',  ( 139.6830278787118402, -9.225297888154202042, -7.967375165638989287 ) ) ;
#22062 = CARTESIAN_POINT ( 'NONE',  ( -3.464101615137725076, 5.999999999999979572, -155.5863248654052029 ) ) ;
#22063 = CIRCLE ( 'NONE', #26997, 1.000000000000000222 ) ;
#22064 = CARTESIAN_POINT ( 'NONE',  ( 5.196152422706629359, 3.000000000000002665, -125.0386751345948255 ) ) ;
#22065 = CARTESIAN_POINT ( 'NONE',  ( -5.999999999999963585, 1.780251999655701777E-13, -74.33632486540523132 ) ) ;
#22066 = DIRECTION ( 'NONE',  ( 1.000000000000000000, -5.551115123125773458E-17, -1.260129944081490338E-35 ) ) ;
#22067 = ORIENTED_EDGE ( 'NONE', *, *, #10363, .T. ) ;
#22068 = CARTESIAN_POINT ( 'NONE',  ( 161.3437500000000568, -6.000000000000005329, -2.485281374238555774 ) ) ;
#22069 = CARTESIAN_POINT ( 'NONE',  ( 140.5000000000000284, -11.45643923738959202, 5.000000000000004441 ) ) ;
#22070 = CARTESIAN_POINT ( 'NONE',  ( -5.196152422706601826, 2.999999999999975131, -82.53867513459483973 ) ) ;
#22071 = CARTESIAN_POINT ( 'NONE',  ( 104.6247167782375271, 1.849990392679523588, 0.000000000000000000 ) ) ;
#22072 = CARTESIAN_POINT ( 'NONE',  ( -5.999999999999956479, -1.607695154586745057, -116.2693375672974270 ) ) ;
#22073 = ORIENTED_EDGE ( 'NONE', *, *, #9983, .T. ) ;
#22074 = EDGE_LOOP ( 'NONE', ( #3058, #6620, #21186, #26521 ) ) ;
#22075 = ADVANCED_FACE ( 'NONE', ( #12425 ), #19306, .T. ) ;
#22076 = CARTESIAN_POINT ( 'NONE',  ( -4.763139720814407951, 2.749999999999946709, -101.7500000000000000 ) ) ;
#22077 = AXIS2_PLACEMENT_3D ( 'NONE', #4236, #25425, #17957 ) ;
#22078 = CARTESIAN_POINT ( 'NONE',  ( -3.608439182435115633, 6.249999999999965361, -117.3080127018922525 ) ) ;
#22079 = ORIENTED_EDGE ( 'NONE', *, *, #26126, .F. ) ;
#22080 = CARTESIAN_POINT ( 'NONE',  ( 3.464101615137757051, -5.999999999999979572, -60.91367513459483263 ) ) ;
#22081 = VECTOR ( 'NONE', #16864, 1000.000000000000000 ) ;
#22082 = CARTESIAN_POINT ( 'NONE',  ( -7.216878364870328078, 0.000000000000000000, -158.1919872981078186 ) ) ;
#22083 = LINE ( 'NONE', #5770, #17670 ) ;
#22084 = CARTESIAN_POINT ( 'NONE',  ( -3.608439182435115633, 6.249999999999965361, -58.80801270189223118 ) ) ;
#22085 = ORIENTED_EDGE ( 'NONE', *, *, #20751, .T. ) ;
#22086 = CARTESIAN_POINT ( 'NONE',  ( -5.999999999999963585, 8.134310703387671600E-14, -116.9136751345948539 ) ) ;
#22087 = EDGE_CURVE ( 'NONE', #9038, #4270, #21768, .T. ) ;
#22088 = DIRECTION ( 'NONE',  ( -8.326672684688675286E-17, -2.081668171172168821E-17, 1.000000000000000000 ) ) ;
#22089 = CARTESIAN_POINT ( 'NONE',  ( -5.380303083296078093, 9.596003543682472881, -22.31547897336682951 ) ) ;
#22090 = CARTESIAN_POINT ( 'NONE',  ( 155.8050748654052313, 5.500000000000012434, 2.278174593052012309 ) ) ;
#22091 = CARTESIAN_POINT ( 'NONE',  ( 6.350852961086080661, -9.614813431917819062E-14, -174.3750000000000284 ) ) ;
#22092 = CARTESIAN_POINT ( 'NONE',  ( 118.6249999999998010, -1.767766952966431937, -1.767766952966209892 ) ) ;
#22093 = FACE_OUTER_BOUND ( 'NONE', #11768, .T. ) ;
#22094 = CARTESIAN_POINT ( 'NONE',  ( -7.216878364870328078, 0.000000000000000000, -168.0580127018922383 ) ) ;
#22095 = CARTESIAN_POINT ( 'NONE',  ( -0.6046674458933997132, -9.395332554106689216, 4.067501169440991049 ) ) ;
#22096 = CARTESIAN_POINT ( 'NONE',  ( 24.68750000000014566, -0.8284271247460553989, -2.000000000000151879 ) ) ;
#22097 =( BOUNDED_CURVE ( )  B_SPLINE_CURVE ( 2, ( #18953, #5073, #4784, #23840, #12202, #28122, #11745, #16657, #12339 ),
 .UNSPECIFIED., .F., .F. ) 
 B_SPLINE_CURVE_WITH_KNOTS ( ( 3, 2, 2, 2, 3 ),
 ( 0.4972222222222222321, 0.4981481481481481177, 0.5000000000000000000, 0.5018518518518517713, 0.5027777777777777679 ),
 .UNSPECIFIED. ) 
 CURVE ( )  GEOMETRIC_REPRESENTATION_ITEM ( )  RATIONAL_B_SPLINE_CURVE ( ( 0.9330127018922194093, 0.9330127018922194093, 1.000000000000000000, 0.8660254037844388186, 1.000000000000000000, 0.8660254037844388186, 1.000000000000000000, 0.9330127018922194093, 0.9330127018922194093 ) ) 
 REPRESENTATION_ITEM ( '' )  );
#22098 = CARTESIAN_POINT ( 'NONE',  ( -3.175426480542816066, 5.499999999999865885, -118.3750000000000284 ) ) ;
#22099 = CARTESIAN_POINT ( 'NONE',  ( 135.2583738898383103, -8.263074927440506201, 8.258625120961028188 ) ) ;
#22100 = CARTESIAN_POINT ( 'NONE',  ( -3.175426480542816510, -5.500000000000057732, -105.8750000000000284 ) ) ;
#22101 = LINE ( 'NONE', #1178, #15330 ) ;
#22102 = CARTESIAN_POINT ( 'NONE',  ( 135.0000000000000284, -8.500000000000007105, 8.000000000000007105 ) ) ;
#22103 = CARTESIAN_POINT ( 'NONE',  ( 6.000000000000000888, 1.607695154586715303, -118.5193375672974412 ) ) ;
#22104 = VERTEX_POINT ( 'NONE', #712 ) ;
#22105 = CARTESIAN_POINT ( 'NONE',  ( 14.75000000000012434, 1.873492889145067508, 1.873492889144734441 ) ) ;
#22106 = CARTESIAN_POINT ( 'NONE',  ( 119.4999999999999289, -2.499999999999919176, 0.000000000000000000 ) ) ;
#22107 = VECTOR ( 'NONE', #9015, 1000.000000000000000 ) ;
#22108 = CARTESIAN_POINT ( 'NONE',  ( -3.464101615137757051, -5.999999999999979572, -76.16367513459483973 ) ) ;
#22109 = ORIENTED_EDGE ( 'NONE', *, *, #5445, .F. ) ;
#22110 = CARTESIAN_POINT ( 'NONE',  ( -5.412658773652739619, 3.124999999999975131, -80.31698729810781856 ) ) ;
#22111 = CARTESIAN_POINT ( 'NONE',  ( 5.999999999999949374, -1.607695154586841868, -129.1533121635129930 ) ) ;
#22112 = ORIENTED_EDGE ( 'NONE', *, *, #26330, .T. ) ;
#22113 = CARTESIAN_POINT ( 'NONE',  ( -5.999999999999963585, 1.780251999655701777E-13, -61.41367513459483973 ) ) ;
#22114 = EDGE_LOOP ( 'NONE', ( #2165, #27473, #12969, #27633 ) ) ;
#22115 = ORIENTED_EDGE ( 'NONE', *, *, #7278, .T. ) ;
#22116 = CARTESIAN_POINT ( 'NONE',  ( 132.5773502691896510, 5.000000000000004441, 0.000000000000000000 ) ) ;
#22117 = EDGE_CURVE ( 'NONE', #16860, #15423, #15802, .T. ) ;
#22118 = EDGE_CURVE ( 'NONE', #3951, #11992, #28504, .T. ) ;
#22119 = VERTEX_POINT ( 'NONE', #14716 ) ;
#22120 = CARTESIAN_POINT ( 'NONE',  ( 5.412658773652739619, 3.124999999999988898, -134.8169872981078186 ) ) ;
#22121 = CARTESIAN_POINT ( 'NONE',  ( 6.000000000000000888, 1.607695154586715303, -131.0966878364870922 ) ) ;
#22122 =( LENGTH_UNIT ( ) NAMED_UNIT ( * ) SI_UNIT ( .MILLI., .METRE. ) );
#22123 = VECTOR ( 'NONE', #7818, 1000.000000000000000 ) ;
#22124 = ORIENTED_EDGE ( 'NONE', *, *, #13988, .F. ) ;
#22125 = CARTESIAN_POINT ( 'NONE',  ( 15.37500000000011013, -1.414213562373034527, 1.414213562373034527 ) ) ;
#22126 = CARTESIAN_POINT ( 'NONE',  ( 1.000000000000000888, -16.43939393939395188, -5.999693900976774685 ) ) ;
#22127 = DIRECTION ( 'NONE',  ( 1.000000000000000000, 0.000000000000000000, 0.000000000000000000 ) ) ;
#22128 = FACE_OUTER_BOUND ( 'NONE', #5063, .T. ) ;
#22129 = AXIS2_PLACEMENT_3D ( 'NONE', #17779, #5443, #3292 ) ;
#22130 = CARTESIAN_POINT ( 'NONE',  ( 135.0000000000000284, -9.047800747817552391, 7.500000000000007105 ) ) ;
#22131 = CARTESIAN_POINT ( 'NONE',  ( 0.9563234411482145481, -15.26191353904648551, -8.566444784294999337 ) ) ;
#22132 = CARTESIAN_POINT ( 'NONE',  ( 3.608439182435180470, 6.249999999999982236, -68.69198729810780435 ) ) ;
#22133 = CARTESIAN_POINT ( 'NONE',  ( -3.608439182435115633, 6.249999999999965361, -54.94198729810780435 ) ) ;
#22134 = DIRECTION ( 'NONE',  ( 0.000000000000000000, 0.000000000000000000, -1.000000000000000000 ) ) ;
#22135 = CARTESIAN_POINT ( 'NONE',  ( 5.999999999999949374, 1.607695154586804565, -75.01933756729745539 ) ) ;
#22136 =( BOUNDED_CURVE ( )  B_SPLINE_CURVE ( 2, ( #1721, #6320, #18188, #25059, #16060, #2035, #3857, #18345, #11277 ),
 .UNSPECIFIED., .F., .T. ) 
 B_SPLINE_CURVE_WITH_KNOTS ( ( 3, 2, 2, 2, 3 ),
 ( 0.1406250000000000000, 0.1484375000000000000, 0.1562500000000000000, 0.1640625000000000000, 0.1718750000000000000 ),
 .UNSPECIFIED. ) 
 CURVE ( )  GEOMETRIC_REPRESENTATION_ITEM ( )  RATIONAL_B_SPLINE_CURVE ( ( 1.000000000000000000, 0.9238795325112867385, 1.000000000000000000, 0.9238795325112867385, 1.000000000000000000, 0.9238795325112867385, 1.000000000000000000, 0.9238795325112867385, 1.000000000000000000 ) ) 
 REPRESENTATION_ITEM ( '' )  );
#22137 = CARTESIAN_POINT ( 'NONE',  ( 3.175426480543072749, -5.500000000000105693, -128.1249999999999716 ) ) ;
#22138 = ORIENTED_EDGE ( 'NONE', *, *, #23072, .F. ) ;
#22139 = CARTESIAN_POINT ( 'NONE',  ( 5.999999999999988454, 1.607695154586737729, -158.0966878364870922 ) ) ;
#22140 = DIRECTION ( 'NONE',  ( -7.147005652999508048E-36, 5.642372883946980038E-36, 1.000000000000000000 ) ) ;
#22141 = CARTESIAN_POINT ( 'NONE',  ( 5.196152422706629359, -2.999999999999988898, -159.7886751345948255 ) ) ;
#22142 = CARTESIAN_POINT ( 'NONE',  ( 112.7261751345945413, -1.999999999999941602, 0.8284271247465359034 ) ) ;
#22143 = VERTEX_POINT ( 'NONE', #21624 ) ;
#22144 = CARTESIAN_POINT ( 'NONE',  ( 112.7497167782374845, 1.308140751793779311, 1.308140751793973600 ) ) ;
#22145 = CARTESIAN_POINT ( 'NONE',  ( 11.03867513459494454, 1.665334536937734811E-13, -2.500000000000113243 ) ) ;
#22146 = CARTESIAN_POINT ( 'NONE',  ( 10.50000000000003730, -1.999999999999835243, 0.000000000000000000 ) ) ;
#22147 = CARTESIAN_POINT ( 'NONE',  ( -5.412658773652739619, 3.124999999999975131, -96.81698729810783277 ) ) ;
#22148 = CIRCLE ( 'NONE', #1518, 0.5000000000000004441 ) ;
#22149 = FILL_AREA_STYLE ('',( #15095 ) ) ;
#22150 = DIRECTION ( 'NONE',  ( 1.000000000000000000, 0.000000000000000000, 0.000000000000000000 ) ) ;
#22151 = CARTESIAN_POINT ( 'NONE',  ( 113.4374999999998721, -2.499999999999994671, 1.035533905932869425 ) ) ;
#22152 = AXIS2_PLACEMENT_3D ( 'NONE', #29292, #17211, #15373 ) ;
#22153 = SURFACE_SIDE_STYLE ('',( #3384 ) ) ;
#22154 = CARTESIAN_POINT ( 'NONE',  ( 140.3637585460053572, -11.68187927300244411, 4.222310544175132740 ) ) ;
#22155 = ADVANCED_FACE ( 'NONE', ( #3004 ), #10470, .F. ) ;
#22156 = CARTESIAN_POINT ( 'NONE',  ( 25.31250000000007816, 2.649519052838419153, -1.097466725451439196 ) ) ;
#22157 = CIRCLE ( 'NONE', #3493, 11.00000000000001599 ) ;
#22158 = CARTESIAN_POINT ( 'NONE',  ( 159.5094690746824142, -11.10052039921582079, 4.558404387674897862 ) ) ;
#22159 = CARTESIAN_POINT ( 'NONE',  ( 4.763139720814407951, 2.750000000000002665, -48.25000000000001421 ) ) ;
#22160 = DIRECTION ( 'NONE',  ( -1.000000000000000000, -1.665334536937731113E-16, 1.526556658859586792E-16 ) ) ;
#22161 = CARTESIAN_POINT ( 'NONE',  ( 5.196152422706629359, -2.999999999999988898, -134.2886751345947971 ) ) ;
#22162 = CARTESIAN_POINT ( 'NONE',  ( 2.775557561562891351E-14, -6.250000000000061284, -76.18301270189226670 ) ) ;
#22163 = CARTESIAN_POINT ( 'NONE',  ( -5.999999999999904965, -1.607695154586834541, -173.2693375672974412 ) ) ;
#22164 = CARTESIAN_POINT ( 'NONE',  ( 152.8913997308104626, -2.071067811865468400, 4.999999999999989342 ) ) ;
#22165 = AXIS2_PLACEMENT_3D ( 'NONE', #993, #17021, #21914 ) ;
#22166 = CARTESIAN_POINT ( 'NONE',  ( -5.999999999999962697, 3.323446944526963260E-14, -149.3363248654052313 ) ) ;
#22167 = DIRECTION ( 'NONE',  ( -7.147005652999508048E-36, 5.642372883946980038E-36, 1.000000000000000000 ) ) ;
#22168 = CARTESIAN_POINT ( 'NONE',  ( -5.999999999999963585, 1.780251999655701777E-13, -47.91367513459483973 ) ) ;
#22169 = CARTESIAN_POINT ( 'NONE',  ( 135.4369124609227129, -8.875665394635735339, 8.012677223695028772 ) ) ;
#22170 = CARTESIAN_POINT ( 'NONE',  ( -6.350852961085760029, -1.281975124255709124E-13, -128.6250000000000000 ) ) ;
#22171 = CARTESIAN_POINT ( 'NONE',  ( 5.196152422706629359, 3.000000000000002665, -68.96132486540523132 ) ) ;
#22172 = DIRECTION ( 'NONE',  ( -0.000000000000000000, -0.000000000000000000, -1.000000000000000000 ) ) ;
#22173 = CARTESIAN_POINT ( 'NONE',  ( 6.000000000000000888, 1.607695154586715303, -67.51933756729745539 ) ) ;
#22174 = CARTESIAN_POINT ( 'NONE',  ( 3.175426480543072749, -5.500000000000105693, -60.62500000000000000 ) ) ;
#22175 = CARTESIAN_POINT ( 'NONE',  ( -4.763139720814407951, -2.750000000000016431, -55.00000000000004974 ) ) ;
#22176 = SURFACE_SIDE_STYLE ('',( #5268 ) ) ;
#22177 = VERTEX_POINT ( 'NONE', #26204 ) ;
#22178 = CARTESIAN_POINT ( 'NONE',  ( 153.4687500000000853, -2.485281374238585972, 6.000000000000005329 ) ) ;
#22179 = CARTESIAN_POINT ( 'NONE',  ( 15.87500000000008349, 1.414213562373201061, -1.414213562373090038 ) ) ;
#22180 = AXIS2_PLACEMENT_3D ( 'NONE', #29211, #1582, #8173 ) ;
#22181 = ADVANCED_FACE ( 'NONE', ( #26494 ), #21476, .T. ) ;
#22182 = CARTESIAN_POINT ( 'NONE',  ( 114.9613248654051318, 1.665334536937734811E-13, 2.000000000000223821 ) ) ;
#22183 = CARTESIAN_POINT ( 'NONE',  ( 113.4997167782376550, 1.308140751793640533, -1.308140751793640533 ) ) ;
#22184 = ORIENTED_EDGE ( 'NONE', *, *, #2899, .T. ) ;
#22185 = CARTESIAN_POINT ( 'NONE',  ( 145.5937500000000284, 6.000000000000005329, 2.485281374238585972 ) ) ;
#22186 = CARTESIAN_POINT ( 'NONE',  ( 161.3871073408037375, -5.626013716664558295, -1.762305681933894475 ) ) ;
#22187 = EDGE_LOOP ( 'NONE', ( #13808, #14337, #13732, #19477 ) ) ;
#22188 = CARTESIAN_POINT ( 'NONE',  ( -2.775557561562891351E-14, -5.500000000000115463, -144.7500000000000568 ) ) ;
#22189 = EDGE_CURVE ( 'NONE', #9271, #13246, #2039, .T. ) ;
#22190 = CARTESIAN_POINT ( 'NONE',  ( 3.608439182435180470, 6.249999999999982236, -50.69198729810784698 ) ) ;
#22191 = CARTESIAN_POINT ( 'NONE',  ( 16.62500000000013856, -1.414213562372867994, -1.414213562373145550 ) ) ;
#22192 = ORIENTED_EDGE ( 'NONE', *, *, #6044, .F. ) ;
#22193 = CARTESIAN_POINT ( 'NONE',  ( -3.608439182435115633, 6.249999999999965361, -147.9419872981078470 ) ) ;
#22194 = CARTESIAN_POINT ( 'NONE',  ( -3.175426480542816510, -5.500000000000057732, -80.37500000000002842 ) ) ;
#22195 = CARTESIAN_POINT ( 'NONE',  ( 13.62500000000005329, 5.551115123125782702E-14, 2.649519052838167354 ) ) ;
#22196 = VERTEX_POINT ( 'NONE', #18883 ) ;
#22197 = CARTESIAN_POINT ( 'NONE',  ( -5.999999999999964473, 9.063946212346262433E-15, -175.4136751345948824 ) ) ;
#22198 = FACE_OUTER_BOUND ( 'NONE', #443, .T. ) ;
#22199 = FACE_OUTER_BOUND ( 'NONE', #8779, .T. ) ;
#22200 = CARTESIAN_POINT ( 'NONE',  ( 135.9026387045187221, -8.798545334315203803, -8.160000000000000142 ) ) ;
#22201 = DIRECTION ( 'NONE',  ( -1.000000000000000000, 0.000000000000000000, 0.000000000000000000 ) ) ;
#22202 = CARTESIAN_POINT ( 'NONE',  ( -2.775557561562891351E-14, -5.500000000000115463, -159.7500000000000568 ) ) ;
#22203 = LINE ( 'NONE', #29708, #23665 ) ;
#22204 = CARTESIAN_POINT ( 'NONE',  ( -3.175426480542816510, -5.500000000000057732, -143.3750000000000000 ) ) ;
#22205 = CARTESIAN_POINT ( 'NONE',  ( 134.9999999999999432, 5.815044816414753015, 1.151864612277130551 ) ) ;
#22206 =( NAMED_UNIT ( * ) SI_UNIT ( $, .STERADIAN. ) SOLID_ANGLE_UNIT ( ) );
#22207 = CARTESIAN_POINT ( 'NONE',  ( 3.175426480543072749, 5.499999999999865885, -94.62500000000002842 ) ) ;
#22208 = DIRECTION ( 'NONE',  ( 0.000000000000000000, -1.000000000000000000, 0.000000000000000000 ) ) ;
#22209 = DIRECTION ( 'NONE',  ( -7.147005652999508048E-36, 5.642372883946980038E-36, 1.000000000000000000 ) ) ;
#22210 = CARTESIAN_POINT ( 'NONE',  ( -6.350852961085760029, -1.281975124255709124E-13, -79.12500000000001421 ) ) ;
#22211 = CARTESIAN_POINT ( 'NONE',  ( 152.5461002691896795, -2.071067811865468400, 4.999999999999989342 ) ) ;
#22212 = CARTESIAN_POINT ( 'NONE',  ( 6.000000000000000888, -1.859271017917181981E-14, -114.6636751345948255 ) ) ;
#22213 = DIRECTION ( 'NONE',  ( 1.000000000000000000, -5.551115123125774074E-17, 0.000000000000000000 ) ) ;
#22214 = EDGE_CURVE ( 'NONE', #3609, #25966, #27101, .T. ) ;
#22215 = CARTESIAN_POINT ( 'NONE',  ( 0.000000000000000000, 0.000000000000000000, 0.000000000000000000 ) ) ;
#22216 = DIRECTION ( 'NONE',  ( 1.000000000000000000, -5.551115123125773458E-17, -1.260129944081490338E-35 ) ) ;
#22217 =( BOUNDED_CURVE ( )  B_SPLINE_CURVE ( 2, ( #25381, #20955, #18361, #25542, #13608, #13454, #27834, #22800, #2209 ),
 .UNSPECIFIED., .F., .T. ) 
 B_SPLINE_CURVE_WITH_KNOTS ( ( 3, 2, 2, 2, 3 ),
 ( 0.6406250000000000000, 0.6484375000000000000, 0.6562500000000000000, 0.6640625000000000000, 0.6718750000000000000 ),
 .UNSPECIFIED. ) 
 CURVE ( )  GEOMETRIC_REPRESENTATION_ITEM ( )  RATIONAL_B_SPLINE_CURVE ( ( 1.000000000000000000, 0.9238795325112867385, 1.000000000000000000, 0.9238795325112867385, 1.000000000000000000, 0.9238795325112867385, 1.000000000000000000, 0.9238795325112867385, 1.000000000000000000 ) ) 
 REPRESENTATION_ITEM ( '' )  );
#22218 = VERTEX_POINT ( 'NONE', #7180 ) ;
#22219 = CARTESIAN_POINT ( 'NONE',  ( 160.5937500000000284, 6.000000000000005329, 2.485281374238585972 ) ) ;
#22220 = CARTESIAN_POINT ( 'NONE',  ( 6.000000000000000888, 1.743066579297358182E-13, -73.58632486540520290 ) ) ;
#22221 = CARTESIAN_POINT ( 'NONE',  ( -5.999999999999963585, 8.134310703387671600E-14, -131.3363248654052313 ) ) ;
#22222 = CARTESIAN_POINT ( 'NONE',  ( 120.1252832217621176, -5.551115123125782702E-14, -1.849990392679523588 ) ) ;
#22223 = VERTEX_POINT ( 'NONE', #25914 ) ;
#22224 = EDGE_CURVE ( 'NONE', #22958, #15258, #22229, .T. ) ;
#22225 =( BOUNDED_CURVE ( )  B_SPLINE_CURVE ( 2, ( #15880, #6910, #21060, #16332, #25178, #25652, #22903, #13722, #1847 ),
 .UNSPECIFIED., .F., .T. ) 
 B_SPLINE_CURVE_WITH_KNOTS ( ( 3, 2, 2, 2, 3 ),
 ( 0.5638888888888888840, 0.5648148148148148806, 0.5666666666666666519, 0.5685185185185185341, 0.5694444444444444198 ),
 .UNSPECIFIED. ) 
 CURVE ( )  GEOMETRIC_REPRESENTATION_ITEM ( )  RATIONAL_B_SPLINE_CURVE ( ( 0.9330127018922194093, 0.9330127018922194093, 1.000000000000000000, 0.8660254037844388186, 1.000000000000000000, 0.8660254037844388186, 1.000000000000000000, 0.9330127018922234061, 0.9330127018922194093 ) ) 
 REPRESENTATION_ITEM ( '' )  );
#22226 = CARTESIAN_POINT ( 'NONE',  ( -3.175426480542816510, 5.499999999999865885, -107.8750000000000284 ) ) ;
#22227 = CARTESIAN_POINT ( 'NONE',  ( -14.99999999999999289, -54.99999999999990763, 7.500000000000007105 ) ) ;
#22228 = CARTESIAN_POINT ( 'NONE',  ( -5.412658773652684552, -3.125000000000099920, -118.4330127018922099 ) ) ;
#22229 = CIRCLE ( 'NONE', #20761, 12.50000000000000178 ) ;
#22230 = ORIENTED_EDGE ( 'NONE', *, *, #11577, .F. ) ;
#22231 = FACE_OUTER_BOUND ( 'NONE', #1397, .T. ) ;
#22232 = CARTESIAN_POINT ( 'NONE',  ( 106.3749999999999574, -1.767766952966320915, 1.767766952966431937 ) ) ;
#22233 = DIRECTION ( 'NONE',  ( -7.147005652999508048E-36, 5.642372883946980038E-36, 1.000000000000000000 ) ) ;
#22234 = CARTESIAN_POINT ( 'NONE',  ( -3.608439182435052128, -6.250000000000110134, -50.80801270189224539 ) ) ;
#22235 = VERTEX_POINT ( 'NONE', #21320 ) ;
#22236 = CARTESIAN_POINT ( 'NONE',  ( -5.999999999999963585, -1.487416814333745711E-14, -167.3363248654052029 ) ) ;
#22237 = CARTESIAN_POINT ( 'NONE',  ( 116.0000000000000142, 0.000000000000000000, -5.500000000000000000 ) ) ;
#22238 = CARTESIAN_POINT ( 'NONE',  ( 110.0622167782374987, -1.849990392679441875, 0.7662911109079489913 ) ) ;
#22239 = CYLINDRICAL_SURFACE ( 'NONE', #3199, 2.499999999999999112 ) ;
#22240 = CARTESIAN_POINT ( 'NONE',  ( 4.000000000000004441, -2.220446049250312095E-16, -5.040519776325966696E-35 ) ) ;
#22241 = CARTESIAN_POINT ( 'NONE',  ( 3.175426480543072749, -5.500000000000105693, -167.1250000000000000 ) ) ;
#22242 = CARTESIAN_POINT ( 'NONE',  ( 104.9377832217622171, -1.849990392679411677, -0.7662911109076485650 ) ) ;
#22243 = CARTESIAN_POINT ( 'NONE',  ( -5.999999999999962697, 3.323446944526963260E-14, -158.3363248654052313 ) ) ;
#22244 = CARTESIAN_POINT ( 'NONE',  ( 2.775557561562891351E-14, -6.250000000000061284, -169.1830127018922383 ) ) ;
#22245 = CARTESIAN_POINT ( 'NONE',  ( -5.999999999999963585, 1.780251999655701777E-13, -47.91367513459483973 ) ) ;
#22246 = CARTESIAN_POINT ( 'NONE',  ( 4.763139720814407951, -2.749999999999988454, -115.9999999999999858 ) ) ;
#22247 = LINE ( 'NONE', #8242, #21279 ) ;
#22248 = CARTESIAN_POINT ( 'NONE',  ( -3.175426480542816510, 5.499999999999865885, -104.8750000000000142 ) ) ;
#22249 = FACE_OUTER_BOUND ( 'NONE', #27272, .T. ) ;
#22250 =( NAMED_UNIT ( * ) SI_UNIT ( $, .STERADIAN. ) SOLID_ANGLE_UNIT ( ) );
#22251 = CARTESIAN_POINT ( 'NONE',  ( 130.0000000000000284, -60.00000000000001421, 4.000000000000003553 ) ) ;
#22252 = ORIENTED_EDGE ( 'NONE', *, *, #2849, .T. ) ;
#22253 = CARTESIAN_POINT ( 'NONE',  ( 13.75000000000012257, 1.873492889145067508, 1.873492889144734441 ) ) ;
#22254 = CARTESIAN_POINT ( 'NONE',  ( 119.1249999999999432, 1.767766952966348670, 1.767766952966431937 ) ) ;
#22255 = EDGE_CURVE ( 'NONE', #4728, #22693, #26148, .T. ) ;
#22256 = CARTESIAN_POINT ( 'NONE',  ( 143.3363248654052029, 0.000000000000000000, -5.500000000000005329 ) ) ;
#22257 = VERTEX_POINT ( 'NONE', #15644 ) ;
#22258 = CARTESIAN_POINT ( 'NONE',  ( -4.763139720814407951, 2.749999999999946709, -158.7500000000000568 ) ) ;
#22259 = CARTESIAN_POINT ( 'NONE',  ( 135.5000000000000000, -9.047800747817552391, 7.500000000000007105 ) ) ;
#22260 = CIRCLE ( 'NONE', #19796, 14.49999999999999822 ) ;
#22261 = CARTESIAN_POINT ( 'NONE',  ( 2.775557561562891351E-14, 6.250000000000033751, -82.06698729810779014 ) ) ;
#22262 = ORIENTED_EDGE ( 'NONE', *, *, #2860, .F. ) ;
#22263 = ADVANCED_FACE ( 'NONE', ( #8212 ), #12725, .T. ) ;
#22264 = FACE_OUTER_BOUND ( 'NONE', #19223, .T. ) ;
#22265 = ORIENTED_EDGE ( 'NONE', *, *, #7099, .F. ) ;
#22266 = VERTEX_POINT ( 'NONE', #22369 ) ;
#22267 = CARTESIAN_POINT ( 'NONE',  ( 155.0625000000000284, -4.242640687119298093, 4.242640687119298093 ) ) ;
#22268 = B_SPLINE_CURVE_WITH_KNOTS ( 'NONE', 3,
 ( #19115, #12366, #7420, #21715 ),
 .UNSPECIFIED., .F., .F.,
 ( 4, 4 ),
 ( 0.000000000000000000, 0.0002043583609089599416 ),
 .UNSPECIFIED. ) ;
#22269 = CARTESIAN_POINT ( 'NONE',  ( 2.775557561562891351E-14, -6.250000000000061284, -136.1830127018922667 ) ) ;
#22270 = VERTEX_POINT ( 'NONE', #10869 ) ;
#22271 = CARTESIAN_POINT ( 'NONE',  ( -3.608439182435115633, 6.249999999999965361, -123.9419872981078043 ) ) ;
#22272 = CARTESIAN_POINT ( 'NONE',  ( 3.175426480543072749, -5.500000000000105693, -170.1250000000000000 ) ) ;
#22273 = CARTESIAN_POINT ( 'NONE',  ( 6.000000000000000888, -1.859271017917181981E-14, -167.1636751345948539 ) ) ;
#22274 = CARTESIAN_POINT ( 'NONE',  ( 19.96132486540530593, 5.551115123125782702E-14, 2.500000000000002220 ) ) ;
#22275 = ORIENTED_EDGE ( 'NONE', *, *, #24287, .F. ) ;
#22276 = CARTESIAN_POINT ( 'NONE',  ( 16.50000000000004263, -1.999999999999835243, 0.000000000000000000 ) ) ;
#22277 = CARTESIAN_POINT ( 'NONE',  ( -5.999999999999971578, 1.607695154586715303, -134.9806624327026157 ) ) ;
#22278 = CARTESIAN_POINT ( 'NONE',  ( 5.196152422706629359, 3.000000000000002665, -164.0386751345947971 ) ) ;
#22279 =( LENGTH_UNIT ( ) NAMED_UNIT ( * ) SI_UNIT ( .MILLI., .METRE. ) );
#22280 = CARTESIAN_POINT ( 'NONE',  ( -3.464101615137725076, 5.999999999999979572, -90.16367513459483973 ) ) ;
#22281 = CARTESIAN_POINT ( 'NONE',  ( 139.7738248654052313, -3.889087296526011706, 3.889087296526011706 ) ) ;
#22282 = CARTESIAN_POINT ( 'NONE',  ( 0.000000000000000000, 5.999999999999977796, -46.21132486540524553 ) ) ;
#22283 = CARTESIAN_POINT ( 'NONE',  ( 2.775557561562891351E-14, -6.250000000000061284, -67.81698729810781856 ) ) ;
#22284 = CARTESIAN_POINT ( 'NONE',  ( -3.608439182435115633, 6.249999999999965361, -56.44198729810781145 ) ) ;
#22285 = DIRECTION ( 'NONE',  ( 1.000000000000000000, -5.551115123125773458E-17, -1.260129944081490338E-35 ) ) ;
#22286 =( LENGTH_UNIT ( ) NAMED_UNIT ( * ) SI_UNIT ( .MILLI., .METRE. ) );
#22287 = CARTESIAN_POINT ( 'NONE',  ( 1.000000000000000888, -15.50000000000001421, 5.656854249492387687 ) ) ;
#22288 = CYLINDRICAL_SURFACE ( 'NONE', #3924, 6.000000000000000888 ) ;
#22289 = CARTESIAN_POINT ( 'NONE',  ( 0.000000000000000000, 5.499999999999991118, -127.5000000000000568 ) ) ;
#22290 = CARTESIAN_POINT ( 'NONE',  ( -5.999999999999963585, 1.780251999655701777E-13, -91.41367513459486815 ) ) ;
#22291 = ORIENTED_EDGE ( 'NONE', *, *, #7847, .F. ) ;
#22292 = CARTESIAN_POINT ( 'NONE',  ( 24.18750000000012079, -2.649519052838238409, -1.097466725451499370 ) ) ;
#22293 = EDGE_CURVE ( 'NONE', #15054, #18896, #27126, .T. ) ;
#22294 = CARTESIAN_POINT ( 'NONE',  ( 160.1175748654052029, 5.500000000000012434, -2.278174593052012309 ) ) ;
#22295 = CARTESIAN_POINT ( 'NONE',  ( 16.77382486540527751, 2.500000000000144773, 1.035533905932749299 ) ) ;
#22296 = EDGE_CURVE ( 'NONE', #8435, #20245, #14616, .T. ) ;
#22297 = VERTEX_POINT ( 'NONE', #10548 ) ;
#22298 = CARTESIAN_POINT ( 'NONE',  ( 114.5622167782375556, 1.849990392679682127, -0.7662911109076485650 ) ) ;
#22299 = CARTESIAN_POINT ( 'NONE',  ( 0.000000000000000000, 0.000000000000000000, 0.000000000000000000 ) ) ;
#22300 = CARTESIAN_POINT ( 'NONE',  ( 2.775557561562891351E-14, -6.250000000000061284, -94.81698729810783277 ) ) ;
#22301 = CARTESIAN_POINT ( 'NONE',  ( 3.464101615137757051, -5.999999999999979572, -173.4136751345948255 ) ) ;
#22302 = CARTESIAN_POINT ( 'NONE',  ( 116.0000000000000142, 0.000000000000000000, -5.500000000000000000 ) ) ;
#22303 = CARTESIAN_POINT ( 'NONE',  ( 113.8124999999998437, 1.035533905932749299, -2.499999999999904521 ) ) ;
#22304 = CARTESIAN_POINT ( 'NONE',  ( -5.999999999999919176, 1.607695154586804565, -77.40331216351302146 ) ) ;
#22305 = VECTOR ( 'NONE', #28941, 1000.000000000000000 ) ;
#22306 = ORIENTED_EDGE ( 'NONE', *, *, #17953, .F. ) ;
#22307 = CARTESIAN_POINT ( 'NONE',  ( 24.68750000000011724, -1.097466725451379244, 2.649519052838238409 ) ) ;
#22308 = CARTESIAN_POINT ( 'NONE',  ( 160.2036198215142520, -11.22298632203329483, 4.248469099170785412 ) ) ;
#22309 = CARTESIAN_POINT ( 'NONE',  ( -2.775557561562891351E-14, -5.500000000000115463, -47.25000000000001421 ) ) ;
#22310 = CARTESIAN_POINT ( 'NONE',  ( 3.464101615137757051, -5.999999999999979572, -59.41367513459481842 ) ) ;
#22311 = CARTESIAN_POINT ( 'NONE',  ( -5.196152422706573404, -3.000000000000002665, -80.21132486540521711 ) ) ;
#22312 = CARTESIAN_POINT ( 'NONE',  ( 3.608439182435180470, 6.249999999999982236, -77.05801270189225249 ) ) ;
#22313 =( BOUNDED_CURVE ( )  B_SPLINE_CURVE ( 2, ( #28098, #14336, #23673, #14615, #307, #5052, #14762, #19079, #1639 ),
 .UNSPECIFIED., .F., .T. ) 
 B_SPLINE_CURVE_WITH_KNOTS ( ( 3, 2, 2, 2, 3 ),
 ( 0.8124999999999993339, 0.8187499999999995337, 0.8249999999999997335, 0.8312500000000000444, 0.8375000000000002442 ),
 .UNSPECIFIED. ) 
 CURVE ( )  GEOMETRIC_REPRESENTATION_ITEM ( )  RATIONAL_B_SPLINE_CURVE ( ( 1.000000000000008216, 0.9238795325112786339, 1.000000000000000000, 0.9238795325112867385, 1.000000000000000000, 0.9238795325112867385, 1.000000000000000000, 0.9238795325112840739, 1.000000000000002665 ) ) 
 REPRESENTATION_ITEM ( '' )  );
#22314 = DIRECTION ( 'NONE',  ( -7.147005652999508048E-36, 5.642372883946980038E-36, 1.000000000000000000 ) ) ;
#22315 = CARTESIAN_POINT ( 'NONE',  ( 149.4226497308104058, 5.000000000000004441, 0.000000000000000000 ) ) ;
#22316 = CARTESIAN_POINT ( 'NONE',  ( -4.999999999999990230, -14.50000000000001243, -8.000000000000007105 ) ) ;
#22317 = CARTESIAN_POINT ( 'NONE',  ( -1.110223024625164676E-16, 2.000000000000012879, 2.021286199229734960E-15 ) ) ;
#22318 = LINE ( 'NONE', #16976, #14344 ) ;
#22319 = DIRECTION ( 'NONE',  ( 0.000000000000000000, 0.000000000000000000, -1.000000000000000000 ) ) ;
#22320 = CARTESIAN_POINT ( 'NONE',  ( -3.175426480542816066, -5.500000000000057732, -132.8750000000000284 ) ) ;
#22321 = CARTESIAN_POINT ( 'NONE',  ( 0.000000000000000000, -5.999999999999991118, -177.4613248654052313 ) ) ;
#22322 = CARTESIAN_POINT ( 'NONE',  ( 3.608439182435180470, -6.249999999999997335, -149.5580127018922951 ) ) ;
#22323 = CARTESIAN_POINT ( 'NONE',  ( 16.28867513459492145, 2.500000000000002220, 0.000000000000000000 ) ) ;
#22324 = EDGE_LOOP ( 'NONE', ( #27911, #30375, #29693, #10324 ) ) ;
#22325 = CARTESIAN_POINT ( 'NONE',  ( 4.763139720814407951, -2.749999999999988454, -66.50000000000000000 ) ) ;
#22326 = CYLINDRICAL_SURFACE ( 'NONE', #14901, 6.000000000000000888 ) ;
#22327 = CARTESIAN_POINT ( 'NONE',  ( 3.175426480543072749, -5.500000000000105693, -59.12499999999999289 ) ) ;
#22328 = EDGE_CURVE ( 'NONE', #15344, #26402, #28296, .T. ) ;
#22329 = CARTESIAN_POINT ( 'NONE',  ( -5.196152422706601826, 2.999999999999975131, -170.4613248654052313 ) ) ;
#22330 = ORIENTED_EDGE ( 'NONE', *, *, #4387, .F. ) ;
#22331 = CARTESIAN_POINT ( 'NONE',  ( 148.2187500000000284, 2.485281374238556218, -6.000000000000005329 ) ) ;
#22332 = FACE_OUTER_BOUND ( 'NONE', #24707, .T. ) ;
#22333 = CARTESIAN_POINT ( 'NONE',  ( 16.12500000000002842, 1.414213562373201061, 1.414213562373034527 ) ) ;
#22334 = CARTESIAN_POINT ( 'NONE',  ( -5.999999999999964473, 9.063946212346262433E-15, -175.4136751345948824 ) ) ;
#22335 = CARTESIAN_POINT ( 'NONE',  ( 110.6872167782375840, 1.849990392679562001, 0.7662911109078287542 ) ) ;
#22336 = VERTEX_POINT ( 'NONE', #12572 ) ;
#22337 = CARTESIAN_POINT ( 'NONE',  ( 143.6250000000000284, 0.000000000000000000, -6.000000000000005329 ) ) ;
#22338 = CARTESIAN_POINT ( 'NONE',  ( -6.000000000000000888, 1.067854986875958443E-15, 7.560779664488942560E-35 ) ) ;
#22339 = EDGE_LOOP ( 'NONE', ( #25083, #15020, #21780, #18855 ) ) ;
#22340 = VECTOR ( 'NONE', #14250, 1000.000000000000000 ) ;
#22341 = CARTESIAN_POINT ( 'NONE',  ( 3.175426480543072749, 5.499999999999865885, -148.6250000000000284 ) ) ;
#22342 = CARTESIAN_POINT ( 'NONE',  ( -5.412658773652684552, -3.125000000000099920, -48.56698729810781856 ) ) ;
#22343 = CARTESIAN_POINT ( 'NONE',  ( 15.93749999999996980, 2.000000000000091926, -0.8284271247462955401 ) ) ;
#22344 = ORIENTED_EDGE ( 'NONE', *, *, #29597, .T. ) ;
#22345 = CARTESIAN_POINT ( 'NONE',  ( 7.216878364870455975, -6.409875621278545621E-14, -146.9419872981078470 ) ) ;
#22346 = CARTESIAN_POINT ( 'NONE',  ( 3.175426480543072749, 5.499999999999865885, -75.12500000000001421 ) ) ;
#22347 = CARTESIAN_POINT ( 'NONE',  ( 15.31250000000006928, 2.649519052838478661, -1.097466725451679892 ) ) ;
#22348 = CARTESIAN_POINT ( 'NONE',  ( 2.775557561562891351E-14, -6.250000000000061284, -92.68301270189222407 ) ) ;
#22349 = ORIENTED_EDGE ( 'NONE', *, *, #24634, .F. ) ;
#22350 = LINE ( 'NONE', #27237, #27512 ) ;
#22351 = EDGE_CURVE ( 'NONE', #13456, #8510, #21256, .T. ) ;
#22352 = CYLINDRICAL_SURFACE ( 'NONE', #4770, 6.000000000000000888 ) ;
#22353 = CYLINDRICAL_SURFACE ( 'NONE', #472, 6.000000000000000888 ) ;
#22354 = CARTESIAN_POINT ( 'NONE',  ( -4.763139720814407951, -2.750000000000016431, -152.5000000000000284 ) ) ;
#22355 = CARTESIAN_POINT ( 'NONE',  ( 0.000000000000000000, 0.000000000000000000, 0.000000000000000000 ) ) ;
#22356 = CARTESIAN_POINT ( 'NONE',  ( 4.763139720814407951, -2.749999999999988454, -149.0000000000000284 ) ) ;
#22357 = CARTESIAN_POINT ( 'NONE',  ( -2.308094007022951200, 5.188356418780102786, -180.0000000000000568 ) ) ;
#22358 = PRESENTATION_LAYER_ASSIGNMENT (  '', '', ( #274 ) ) ;
#22359 = UNCERTAINTY_MEASURE_WITH_UNIT (LENGTH_MEASURE( 1.000000000000000082E-05 ), #2079, 'distance_accuracy_value', 'NONE');
#22360 = CARTESIAN_POINT ( 'NONE',  ( 3.175426480543072749, -5.500000000000105693, -83.12500000000004263 ) ) ;
#22361 = DIRECTION ( 'NONE',  ( -7.147005652999508048E-36, 5.642372883946980038E-36, 1.000000000000000000 ) ) ;
#22362 = CARTESIAN_POINT ( 'NONE',  ( -4.763139720814407951, 2.749999999999946709, -83.74999999999998579 ) ) ;
#22363 = EDGE_CURVE ( 'NONE', #29150, #651, #5149, .T. ) ;
#22364 = LINE ( 'NONE', #15481, #27053 ) ;
#22365 = CARTESIAN_POINT ( 'NONE',  ( 154.4211002691896510, -4.999999999999989342, -2.071067811865468400 ) ) ;
#22366 = CARTESIAN_POINT ( 'NONE',  ( 6.000000000000000888, -3.330669073875464691E-16, -7.560779664488942560E-35 ) ) ;
#22367 = DIRECTION ( 'NONE',  ( 1.000000000000000000, -5.551115123125773458E-17, -1.260129944081490338E-35 ) ) ;
#22368 = CARTESIAN_POINT ( 'NONE',  ( 144.5550748654052029, -5.500000000000012434, -2.278174593052012309 ) ) ;
#22369 = CARTESIAN_POINT ( 'NONE',  ( 0.000000000000000000, -9.500000000000008882, -5.000000000000004441 ) ) ;
#22370 = CARTESIAN_POINT ( 'NONE',  ( 120.3122167782375413, -0.7662911109077686911, -1.849990392679411677 ) ) ;
#22371 = LINE ( 'NONE', #29409, #5166 ) ;
#22372 = VERTEX_POINT ( 'NONE', #26948 ) ;
#22373 = CARTESIAN_POINT ( 'NONE',  ( -3.464101615137725076, 5.999999999999979572, -73.08632486540520290 ) ) ;
#22374 = CARTESIAN_POINT ( 'NONE',  ( -5.999999999999963585, 1.780251999655701777E-13, -79.41367513459482552 ) ) ;
#22375 = VECTOR ( 'NONE', #18907, 1000.000000000000000 ) ;
#22376 = CARTESIAN_POINT ( 'NONE',  ( 24.91299458739716854, 1.355376207975084402, -1.592815096892554516 ) ) ;
#22377 = EDGE_LOOP ( 'NONE', ( #20021, #27753, #26412, #5341 ) ) ;
#22378 = VERTEX_POINT ( 'NONE', #5907 ) ;
#22379 = CARTESIAN_POINT ( 'NONE',  ( 3.175426480543072749, -5.500000000000105693, -98.12500000000004263 ) ) ;
#22380 = FACE_OUTER_BOUND ( 'NONE', #16417, .T. ) ;
#22381 = CARTESIAN_POINT ( 'NONE',  ( 5.412658773652712085, -3.125000000000086153, -113.4330127018922099 ) ) ;
#22382 = VERTEX_POINT ( 'NONE', #15334 ) ;
#22383 = CARTESIAN_POINT ( 'NONE',  ( 0.000000000000000000, 5.999999999999977796, -94.21132486540523132 ) ) ;
#22384 = CARTESIAN_POINT ( 'NONE',  ( -5.999999999999963585, 1.780251999655701777E-13, -49.41367513459484684 ) ) ;
#22385 = EDGE_CURVE ( 'NONE', #12702, #22602, #24655, .T. ) ;
#22386 = CARTESIAN_POINT ( 'NONE',  ( 21.53867513459484329, 0.000000000000000000, 2.500000000000002220 ) ) ;
#22387 = EDGE_CURVE ( 'NONE', #24608, #15772, #2998, .T. ) ;
#22388 = CARTESIAN_POINT ( 'NONE',  ( -5.412658773652684552, -3.125000000000099920, -49.43301270189226670 ) ) ;
#22389 = ORIENTED_EDGE ( 'NONE', *, *, #907, .T. ) ;
#22390 = DIRECTION ( 'NONE',  ( -0.000000000000000000, -0.000000000000000000, -1.000000000000000000 ) ) ;
#22391 = CARTESIAN_POINT ( 'NONE',  ( -6.000000000000000888, 1.067854986875958443E-15, 7.560779664488942560E-35 ) ) ;
#22392 = DIRECTION ( 'NONE',  ( -7.147005652999508048E-36, 5.642372883946980038E-36, 1.000000000000000000 ) ) ;
#22393 = CARTESIAN_POINT ( 'NONE',  ( 3.175426480543072749, 5.499999999999865885, -172.6250000000000000 ) ) ;
#22394 = CARTESIAN_POINT ( 'NONE',  ( 119.6874999999998010, -1.035533905932809473, -2.499999999999784173 ) ) ;
#22395 = PRESENTATION_STYLE_ASSIGNMENT (( #29896 ) ) ;
#22396 = CARTESIAN_POINT ( 'NONE',  ( -3.608439182435115633, 6.249999999999965361, -169.8080127018922383 ) ) ;
#22397 = CARTESIAN_POINT ( 'NONE',  ( -0.4963810631259263917, -9.251809468437068418, 4.126213593628771825 ) ) ;
#22398 = CARTESIAN_POINT ( 'NONE',  ( 0.000000000000000000, 5.499999999999991118, -107.9999999999999858 ) ) ;
#22399 = DIRECTION ( 'NONE',  ( 1.000000000000000000, -5.551115123125773458E-17, -1.260129944081490338E-35 ) ) ;
#22400 = EDGE_CURVE ( 'NONE', #3562, #23786, #20678, .T. ) ;
#22401 =( BOUNDED_CURVE ( )  B_SPLINE_CURVE ( 2, ( #7869, #21727, #23870, #10204, #5262, #17582, #19427, #24451, #17428 ),
 .UNSPECIFIED., .F., .T. ) 
 B_SPLINE_CURVE_WITH_KNOTS ( ( 3, 2, 2, 2, 3 ),
 ( 0.1805555555555554692, 0.1814814814814814659, 0.1833333333333333481, 0.1851851851851852304, 0.1861111111111111160 ),
 .UNSPECIFIED. ) 
 CURVE ( )  GEOMETRIC_REPRESENTATION_ITEM ( )  RATIONAL_B_SPLINE_CURVE ( ( 0.9330127018922194093, 0.9330127018922154125, 1.000000000000000000, 0.8660254037844388186, 1.000000000000000000, 0.8660254037844388186, 1.000000000000000000, 0.9330127018922194093, 0.9330127018922194093 ) ) 
 REPRESENTATION_ITEM ( '' )  );
#22402 = CARTESIAN_POINT ( 'NONE',  ( -6.350852961085760029, -1.281975124255709124E-13, -101.6250000000000000 ) ) ;
#22403 = EDGE_CURVE ( 'NONE', #19367, #12929, #15950, .T. ) ;
#22404 = DIRECTION ( 'NONE',  ( 1.000000000000000000, -5.551115123125773458E-17, -1.260129944081490338E-35 ) ) ;
#22405 = CARTESIAN_POINT ( 'NONE',  ( -5.196152422706573404, -3.000000000000002665, -112.2886751345948397 ) ) ;
#22406 = CARTESIAN_POINT ( 'NONE',  ( 135.0000000000000284, -8.789428240781155921, 7.941267209061672716 ) ) ;
#22407 = CARTESIAN_POINT ( 'NONE',  ( 16.43750000000011013, 1.097466725451619718, -2.649519052838298805 ) ) ;
#22408 = CARTESIAN_POINT ( 'NONE',  ( -3.464101615137757051, -5.999999999999979572, -90.58632486540521711 ) ) ;
#22409 = CARTESIAN_POINT ( 'NONE',  ( 109.3127832217620607, 1.849990392679591977, -0.7662911109076485650 ) ) ;
#22410 = CARTESIAN_POINT ( 'NONE',  ( 6.000000000000000888, -1.859271017917181981E-14, -80.16367513459481131 ) ) ;
#22411 =( BOUNDED_CURVE ( )  B_SPLINE_CURVE ( 2, ( #25908, #16587, #256, #9639, #7467, #20863, #2418, #16879, #26199 ),
 .UNSPECIFIED., .F., .T. ) 
 B_SPLINE_CURVE_WITH_KNOTS ( ( 3, 2, 2, 2, 3 ),
 ( 0.6718750000000000000, 0.6796875000000000000, 0.6875000000000000000, 0.6953125000000000000, 0.7031250000000000000 ),
 .UNSPECIFIED. ) 
 CURVE ( )  GEOMETRIC_REPRESENTATION_ITEM ( )  RATIONAL_B_SPLINE_CURVE ( ( 1.000000000000000000, 0.9238795325112867385, 1.000000000000000000, 0.9238795325112867385, 1.000000000000000000, 0.9238795325112867385, 1.000000000000000000, 0.9238795325112867385, 1.000000000000000000 ) ) 
 REPRESENTATION_ITEM ( '' )  );
#22412 = ORIENTED_EDGE ( 'NONE', *, *, #12673, .T. ) ;
#22413 = CARTESIAN_POINT ( 'NONE',  ( -3.175426480542816510, -5.500000000000057732, -158.3750000000000284 ) ) ;
#22414 = CARTESIAN_POINT ( 'NONE',  ( 108.6872167782374277, 1.849990392679591977, 0.7662911109078888172 ) ) ;
#22415 = CARTESIAN_POINT ( 'NONE',  ( -3.608439182435052128, -6.250000000000110134, -79.94198729810779014 ) ) ;
#22416 = VERTEX_POINT ( 'NONE', #15799 ) ;
#22417 = AXIS2_PLACEMENT_3D ( 'NONE', #22791, #24775, #10831 ) ;
#22418 = CARTESIAN_POINT ( 'NONE',  ( 24.63750948478215363, 1.344396243822401082, -1.946671111007823862 ) ) ;
#22419 = VERTEX_POINT ( 'NONE', #27706 ) ;
#22420 = CARTESIAN_POINT ( 'NONE',  ( 159.0937500000000284, 6.000000000000005329, 2.485281374238585972 ) ) ;
#22421 = CARTESIAN_POINT ( 'NONE',  ( -4.763139720814407951, 2.749999999999946709, -119.7500000000000284 ) ) ;
#22422 = CARTESIAN_POINT ( 'NONE',  ( 2.775557561562891351E-14, 6.250000000000033751, -141.4330127018922383 ) ) ;
#22423 = ORIENTED_EDGE ( 'NONE', *, *, #6007, .F. ) ;
#22424 = CARTESIAN_POINT ( 'NONE',  ( 161.1037658773653050, -2.857005778783127844E-13, 5.603765877365280090 ) ) ;
#22425 = CARTESIAN_POINT ( 'NONE',  ( 3.608439182435180470, 6.249999999999982236, -125.6919872981078186 ) ) ;
#22426 = CARTESIAN_POINT ( 'NONE',  ( 116.0000000000000142, 0.000000000000000000, 0.000000000000000000 ) ) ;
#22427 = AXIS2_PLACEMENT_3D ( 'NONE', #22532, #17477, #15649 ) ;
#22428 = CARTESIAN_POINT ( 'NONE',  ( 4.763139720814407951, 2.750000000000002665, -172.7500000000000284 ) ) ;
#22429 = CARTESIAN_POINT ( 'NONE',  ( 159.3361461291012517, -11.35074521425119620, 3.948316470164734415 ) ) ;
#22430 = CARTESIAN_POINT ( 'NONE',  ( 107.4761751345946550, 0.8284271247461753029, 2.000000000000212275 ) ) ;
#22431 = EDGE_CURVE ( 'NONE', #28690, #3077, #14790, .T. ) ;
#22432 = ORIENTED_EDGE ( 'NONE', *, *, #28854, .T. ) ;
#22433 = CARTESIAN_POINT ( 'NONE',  ( 16.81250000000007816, 0.8284271247462955401, -2.000000000000091926 ) ) ;
#22434 = CARTESIAN_POINT ( 'NONE',  ( 140.5835741348633690, -11.79178706743166494, 4.000000000000005329 ) ) ;
#22435 = CARTESIAN_POINT ( 'NONE',  ( 0.000000000000000000, -5.999999999999991118, -117.4613248654052313 ) ) ;
#22436 = CARTESIAN_POINT ( 'NONE',  ( 5.196152422706629359, 3.000000000000002665, -92.96132486540520290 ) ) ;
#22437 = DIRECTION ( 'NONE',  ( 0.000000000000000000, -1.000000000000000000, -8.881784197001262184E-16 ) ) ;
#22438 = CARTESIAN_POINT ( 'NONE',  ( 115.5002832217623308, 1.308140751793640533, 1.308140751793640533 ) ) ;
#22439 = CARTESIAN_POINT ( 'NONE',  ( 3.608439182435180470, -6.249999999999997335, -67.69198729810779014 ) ) ;
#22440 = CARTESIAN_POINT ( 'NONE',  ( -7.216878364870328078, 0.000000000000000000, -53.19198729810779724 ) ) ;
#22441 = CARTESIAN_POINT ( 'NONE',  ( 0.7669223171414760731, -15.58766199952932396, 7.954545454545463912 ) ) ;
#22442 = CYLINDRICAL_SURFACE ( 'NONE', #2205, 6.000000000000000888 ) ;
#22443 = DIRECTION ( 'NONE',  ( -0.000000000000000000, -0.000000000000000000, -1.000000000000000000 ) ) ;
#22444 = CARTESIAN_POINT ( 'NONE',  ( 0.000000000000000000, 5.999999999999977796, -74.71132486540521711 ) ) ;
#22445 = EDGE_CURVE ( 'NONE', #15054, #566, #30030, .T. ) ;
#22446 = CARTESIAN_POINT ( 'NONE',  ( -4.763139720814407951, 2.749999999999946709, -130.2500000000000284 ) ) ;
#22447 = ADVANCED_FACE ( 'NONE', ( #27866 ), #2244, .F. ) ;
#22448 = CARTESIAN_POINT ( 'NONE',  ( 5.196152422706629359, 3.000000000000002665, -138.5386751345948255 ) ) ;
#22449 = ORIENTED_EDGE ( 'NONE', *, *, #27396, .T. ) ;
#22450 = CARTESIAN_POINT ( 'NONE',  ( 23.37500000000011724, 1.665334536937734811E-13, -2.649519052838333888 ) ) ;
#22451 = DIRECTION ( 'NONE',  ( -1.000000000000000000, -1.665334536937736783E-16, -2.220446049250315546E-16 ) ) ;
#22452 = CARTESIAN_POINT ( 'NONE',  ( 104.7401757384973280, -1.849990392679412565, 2.220446049250313081E-13 ) ) ;
#22453 = CARTESIAN_POINT ( 'NONE',  ( -5.196152422706601826, 2.999999999999975131, -129.9613248654052313 ) ) ;
#22454 = ORIENTED_EDGE ( 'NONE', *, *, #12141, .F. ) ;
#22455 = AXIS2_PLACEMENT_3D ( 'NONE', #16909, #587, #9974 ) ;
#22456 = CARTESIAN_POINT ( 'NONE',  ( 114.9997167782375698, -1.308140751793612777, 1.308140751793862577 ) ) ;
#22457 = CARTESIAN_POINT ( 'NONE',  ( 6.000000000000000888, 1.607695154586715303, -72.01933756729744118 ) ) ;
#22458 = CARTESIAN_POINT ( 'NONE',  ( -3.608439182435052128, -6.250000000000110134, -114.4419872981078186 ) ) ;
#22459 = CARTESIAN_POINT ( 'NONE',  ( 5.196152422706629359, -2.999999999999988898, -173.2886751345948255 ) ) ;
#22460 = CARTESIAN_POINT ( 'NONE',  ( 113.4999999999999147, -2.499999999999919176, 0.000000000000000000 ) ) ;
#22461 = ORIENTED_EDGE ( 'NONE', *, *, #27420, .T. ) ;
#22462 = FACE_OUTER_BOUND ( 'NONE', #15067, .T. ) ;
#22463 = CARTESIAN_POINT ( 'NONE',  ( 143.2500000000000568, -6.000000000000005329, 0.000000000000000000 ) ) ;
#22464 = CARTESIAN_POINT ( 'NONE',  ( -5.999999999999963585, -1.487416814333745711E-14, -138.8363248654052597 ) ) ;
#22465 = CARTESIAN_POINT ( 'NONE',  ( -4.763139720814407951, 2.749999999999946709, -47.75000000000001421 ) ) ;
#22466 = EDGE_CURVE ( 'NONE', #11750, #25219, #17753, .T. ) ;
#22467 = CARTESIAN_POINT ( 'NONE',  ( 5.196152422706629359, 3.000000000000002665, -69.53867513459482552 ) ) ;
#22468 = CARTESIAN_POINT ( 'NONE',  ( 6.000000000000000888, 7.762456499804234384E-14, -134.1636751345948539 ) ) ;
#22469 = CARTESIAN_POINT ( 'NONE',  ( -3.464101615137757051, -5.999999999999979572, -80.08632486540513185 ) ) ;
#22470 = CARTESIAN_POINT ( 'NONE',  ( 5.412658773652712085, -3.125000000000086153, -78.93301270189223828 ) ) ;
#22471 = CARTESIAN_POINT ( 'NONE',  ( 135.8344003793655190, -8.798545317545935163, -8.160000018081550621 ) ) ;
#22472 = CARTESIAN_POINT ( 'NONE',  ( 152.3288997308104058, 4.999999999999989342, -2.071067811865468400 ) ) ;
#22473 = FACE_OUTER_BOUND ( 'NONE', #30143, .T. ) ;
#22474 =( GEOMETRIC_REPRESENTATION_CONTEXT ( 3 ) GLOBAL_UNCERTAINTY_ASSIGNED_CONTEXT ( ( #8201 ) ) GLOBAL_UNIT_ASSIGNED_CONTEXT ( ( #28461, #6980, #360 ) ) REPRESENTATION_CONTEXT ( 'NONE', 'WORKASPACE' ) );
#22475 = DIRECTION ( 'NONE',  ( 0.000000000000000000, 1.000000000000000000, -0.000000000000000000 ) ) ;
#22476 = CARTESIAN_POINT ( 'NONE',  ( 24.53037769546397584, -0.1516104150550960927, 2.469622304536084112 ) ) ;
#22477 = DIRECTION ( 'NONE',  ( -7.147005652999508048E-36, 5.642372883946980038E-36, 1.000000000000000000 ) ) ;
#22478 = CARTESIAN_POINT ( 'NONE',  ( 6.000000000000000888, -1.859271017917181981E-14, -105.0863248654052313 ) ) ;
#22479 = EDGE_CURVE ( 'NONE', #18033, #27766, #20881, .T. ) ;
#22480 = CARTESIAN_POINT ( 'NONE',  ( 0.000000000000000000, 5.499999999999991118, -129.0000000000000000 ) ) ;
#22481 = CARTESIAN_POINT ( 'NONE',  ( 2.000000000000003109, -1.110223024625156540E-16, -200.0000000000000000 ) ) ;
#22482 = CARTESIAN_POINT ( 'NONE',  ( 2.775557561562891351E-14, -6.250000000000061284, -149.6830127018922099 ) ) ;
#22483 = DIRECTION ( 'NONE',  ( 1.000000000000000000, -5.551115123125773458E-17, -1.260129944081490338E-35 ) ) ;
#22484 = STYLED_ITEM ( 'NONE', ( #19356 ), #3263 ) ;
#22485 = CARTESIAN_POINT ( 'NONE',  ( 116.0000000000000142, 0.000000000000000000, 0.000000000000000000 ) ) ;
#22486 = ORIENTED_EDGE ( 'NONE', *, *, #13379, .T. ) ;
#22487 = CARTESIAN_POINT ( 'NONE',  ( -2.775557561562891351E-14, -5.500000000000115463, -63.75000000000002842 ) ) ;
#22488 = CARTESIAN_POINT ( 'NONE',  ( -4.999999999999990230, -24.99999999999999289, 4.000000000000003553 ) ) ;
#22489 = CARTESIAN_POINT ( 'NONE',  ( -6.000000000000023093, 1.607695154586625819, -170.4033121635129930 ) ) ;
#22490 = ORIENTED_EDGE ( 'NONE', *, *, #4699, .F. ) ;
#22491 = CARTESIAN_POINT ( 'NONE',  ( 108.1249999999999574, 1.767766952966293159, 1.767766952966431937 ) ) ;
#22492 = CARTESIAN_POINT ( 'NONE',  ( 148.3125000000000284, 4.242640687119298093, -4.242640687119298093 ) ) ;
#22493 = CARTESIAN_POINT ( 'NONE',  ( 6.000000000000000888, 7.762456499804234384E-14, -117.6636751345948255 ) ) ;
#22494 = CARTESIAN_POINT ( 'NONE',  ( 16.18750000000014566, 0.8284271247462955401, 2.000000000000031530 ) ) ;
#22495 = CARTESIAN_POINT ( 'NONE',  ( -6.000000000000000888, 1.067854986875958443E-15, 7.560779664488942560E-35 ) ) ;
#22496 = ORIENTED_EDGE ( 'NONE', *, *, #6846, .F. ) ;
#22497 = CARTESIAN_POINT ( 'NONE',  ( 138.3750000000000284, 0.000000000000000000, 6.000000000000005329 ) ) ;
#22498 = CARTESIAN_POINT ( 'NONE',  ( 161.3624454948340485, -5.811493806601979450, -0.8339435799521033310 ) ) ;
#22499 = EDGE_LOOP ( 'NONE', ( #14908, #6502, #12462, #12070 ) ) ;
#22500 = CARTESIAN_POINT ( 'NONE',  ( 0.000000000000000000, 5.499999999999991118, -142.5000000000000284 ) ) ;
#22501 =( BOUNDED_CURVE ( )  B_SPLINE_CURVE ( 2, ( #3291, #14431, #17165, #12717, #12125, #7464, #5294, #22056, #21469 ),
 .UNSPECIFIED., .F., .T. ) 
 B_SPLINE_CURVE_WITH_KNOTS ( ( 3, 2, 2, 2, 3 ),
 ( 0.6375000000000001776, 0.6437500000000004885, 0.6500000000000006883, 0.6562500000000008882, 0.6625000000000010880 ),
 .UNSPECIFIED. ) 
 CURVE ( )  GEOMETRIC_REPRESENTATION_ITEM ( )  RATIONAL_B_SPLINE_CURVE ( ( 0.9999999999999973355, 0.9238795325112894030, 1.000000000000000000, 0.9238795325112867385, 1.000000000000000000, 0.9238795325112867385, 1.000000000000000000, 0.9238795325112731938, 1.000000000000013545 ) ) 
 REPRESENTATION_ITEM ( '' )  );
#22502 = EDGE_LOOP ( 'NONE', ( #24619, #26073, #1271, #11547 ) ) ;
#22503 = CARTESIAN_POINT ( 'NONE',  ( -5.412658773652739619, 3.124999999999975131, -48.81698729810779724 ) ) ;
#22504 = CARTESIAN_POINT ( 'NONE',  ( 18.93750000000016698, 2.000000000000091926, -0.8284271247462354770 ) ) ;
#22505 = ORIENTED_EDGE ( 'NONE', *, *, #11654, .F. ) ;
#22506 = CARTESIAN_POINT ( 'NONE',  ( 0.000000000000000000, 5.499999999999991118, -76.50000000000001421 ) ) ;
#22507 = EDGE_CURVE ( 'NONE', #20198, #24855, #16606, .T. ) ;
#22508 = ADVANCED_FACE ( 'NONE', ( #29870 ), #6528, .F. ) ;
#22509 = CARTESIAN_POINT ( 'NONE',  ( -5.412658773652684552, -3.125000000000099920, -97.43301270189225249 ) ) ;
#22510 = ORIENTED_EDGE ( 'NONE', *, *, #5378, .F. ) ;
#22511 = CIRCLE ( 'NONE', #26407, 16.00000000000000000 ) ;
#22512 = CARTESIAN_POINT ( 'NONE',  ( -3.682280293032447194, -10.37087330740123825, -29.75307074678473640 ) ) ;
#22513 = CARTESIAN_POINT ( 'NONE',  ( 6.000000000000052403, -1.607695154586662678, -83.23066243270257303 ) ) ;
#22514 = CARTESIAN_POINT ( 'NONE',  ( 148.4925748654052313, 2.278174593051996322, 5.500000000000026645 ) ) ;
#22515 = CARTESIAN_POINT ( 'NONE',  ( -3.464101615137757051, -5.999999999999979572, -86.66367513459481131 ) ) ;
#22516 = DIRECTION ( 'NONE',  ( -7.147005652999508048E-36, 5.642372883946980038E-36, 1.000000000000000000 ) ) ;
#22517 = SHAPE_DEFINITION_REPRESENTATION ( #13898, #4035 ) ;
#22518 = CARTESIAN_POINT ( 'NONE',  ( 4.763139720814407951, -2.749999999999988454, -159.5000000000000284 ) ) ;
#22519 = CARTESIAN_POINT ( 'NONE',  ( 117.9613248654051318, 5.551115123125782702E-14, 2.000000000000001776 ) ) ;
#22520 = FACE_OUTER_BOUND ( 'NONE', #20844, .T. ) ;
#22521 = CARTESIAN_POINT ( 'NONE',  ( -6.350852961085760029, -1.281975124255709124E-13, -88.12500000000000000 ) ) ;
#22522 = DIRECTION ( 'NONE',  ( -7.147005652999508048E-36, 5.642372883946980038E-36, 1.000000000000000000 ) ) ;
#22523 = CARTESIAN_POINT ( 'NONE',  ( 24.41367513459491434, 1.767766952966431937, 1.767766952966320915 ) ) ;
#22524 = CARTESIAN_POINT ( 'NONE',  ( -2.775557561562891351E-14, -5.500000000000115463, -83.25000000000004263 ) ) ;
#22525 = LINE ( 'NONE', #6222, #29519 ) ;
#22526 = CARTESIAN_POINT ( 'NONE',  ( 161.0438449402356866, -5.397155697456622825, -1.336872040267217177 ) ) ;
#22527 = CARTESIAN_POINT ( 'NONE',  ( -5.999999999999968026, -1.607695154586722186, -149.8466878364870354 ) ) ;
#22528 = DIRECTION ( 'NONE',  ( 1.000000000000000000, -5.551115123125773458E-17, -1.260129944081490338E-35 ) ) ;
#22529 = CARTESIAN_POINT ( 'NONE',  ( 119.9997167782376124, -1.308140751793529510, 1.308140751793973600 ) ) ;
#22530 = CARTESIAN_POINT ( 'NONE',  ( -3.464101615137725076, 5.999999999999979572, -75.16367513459483973 ) ) ;
#22531 = ORIENTED_EDGE ( 'NONE', *, *, #7373, .F. ) ;
#22532 = CARTESIAN_POINT ( 'NONE',  ( 0.000000000000000000, 0.000000000000000000, 0.000000000000000000 ) ) ;
#22533 = CARTESIAN_POINT ( 'NONE',  ( -5.999999999999956479, -1.607695154586745057, -172.3466878364870922 ) ) ;
#22534 = CARTESIAN_POINT ( 'NONE',  ( 117.0627832217621318, -0.7662911109077686911, -1.849990392679231599 ) ) ;
#22535 = VERTEX_POINT ( 'NONE', #25730 ) ;
#22536 = VERTEX_POINT ( 'NONE', #18997 ) ;
#22537 = CARTESIAN_POINT ( 'NONE',  ( -2.775557561562891351E-14, -5.500000000000115463, -98.25000000000000000 ) ) ;
#22538 = CARTESIAN_POINT ( 'NONE',  ( -5.999999999999919176, 1.607695154586804565, -70.48066243270261566 ) ) ;
#22539 = EDGE_CURVE ( 'NONE', #10886, #26998, #7141, .T. ) ;
#22540 = CARTESIAN_POINT ( 'NONE',  ( -5.412658773652739619, 3.124999999999975131, -117.1830127018922383 ) ) ;
#22541 = ORIENTED_EDGE ( 'NONE', *, *, #22677, .T. ) ;
#22542 = CARTESIAN_POINT ( 'NONE',  ( 17.96132486540527751, 1.110223024625156540E-13, 2.499999999999946709 ) ) ;
#22543 =( LENGTH_UNIT ( ) NAMED_UNIT ( * ) SI_UNIT ( .MILLI., .METRE. ) );
#22544 = CARTESIAN_POINT ( 'NONE',  ( 6.000000000000000888, -3.330669073875464691E-16, -7.560779664488942560E-35 ) ) ;
#22545 = CARTESIAN_POINT ( 'NONE',  ( -5.412658773652739619, 3.124999999999975131, -51.18301270189223828 ) ) ;
#22546 = VECTOR ( 'NONE', #26296, 1000.000000000000000 ) ;
#22547 = ORIENTED_EDGE ( 'NONE', *, *, #14228, .T. ) ;
#22548 = CARTESIAN_POINT ( 'NONE',  ( -3.464101615137725076, 5.999999999999979572, -160.0863248654052313 ) ) ;
#22549 = CARTESIAN_POINT ( 'NONE',  ( 108.7886751345946834, -1.999999999999946265, 1.110223024625156540E-13 ) ) ;
#22550 = AXIS2_PLACEMENT_3D ( 'NONE', #20422, #3969, #6431 ) ;
#22551 = CARTESIAN_POINT ( 'NONE',  ( 146.7261751345948539, -3.889087296526011706, -3.889087296526011706 ) ) ;
#22552 = CARTESIAN_POINT ( 'NONE',  ( 119.0863248654051461, -1.414213562373145550, 1.414213562373145550 ) ) ;
#22553 = CARTESIAN_POINT ( 'NONE',  ( -3.175426480542816510, -5.500000000000057732, -171.8750000000000284 ) ) ;
#22554 = CARTESIAN_POINT ( 'NONE',  ( 114.6249999999999574, -1.767766952966431937, -1.767766952966431937 ) ) ;
#22555 = SURFACE_STYLE_FILL_AREA ( #29745 ) ;
#22556 = CARTESIAN_POINT ( 'NONE',  ( -0.6927266194436426661, -9.614546761112704232, 4.200333198739607532 ) ) ;
#22557 = CARTESIAN_POINT ( 'NONE',  ( 3.175426480543072749, 5.499999999999865885, -111.1249999999999858 ) ) ;
#22558 = CARTESIAN_POINT ( 'NONE',  ( -6.000000000000000888, 1.067854986875958443E-15, 7.560779664488942560E-35 ) ) ;
#22559 = CARTESIAN_POINT ( 'NONE',  ( -3.175426480542816510, -5.500000000000057732, -107.3750000000000284 ) ) ;
#22560 = SURFACE_STYLE_FILL_AREA ( #10753 ) ;
#22561 = CARTESIAN_POINT ( 'NONE',  ( 24.50000000000010658, 5.551115123125782702E-14, -5.551115123125782702E-14 ) ) ;
#22562 = DIRECTION ( 'NONE',  ( -0.000000000000000000, -0.000000000000000000, -1.000000000000000000 ) ) ;
#22563 = EDGE_LOOP ( 'NONE', ( #24693, #17381, #20476, #13508 ) ) ;
#22564 = CARTESIAN_POINT ( 'NONE',  ( 15.93750000000009059, -1.097466725451439196, 2.649519052838178457 ) ) ;
#22565 = CARTESIAN_POINT ( 'NONE',  ( 116.1874999999999005, 1.035533905932839449, 2.500000000000205169 ) ) ;
#22566 = CARTESIAN_POINT ( 'NONE',  ( 110.2502832217623165, 1.308140751793640533, -1.308140751793640533 ) ) ;
#22567 = ORIENTED_EDGE ( 'NONE', *, *, #22789, .T. ) ;
#22568 = CARTESIAN_POINT ( 'NONE',  ( 0.000000000000000000, 5.499999999999991118, -159.0000000000000284 ) ) ;
#22569 = DIRECTION ( 'NONE',  ( 0.000000000000000000, 0.000000000000000000, -1.000000000000000000 ) ) ;
#22570 = EDGE_CURVE ( 'NONE', #27492, #11541, #23592, .T. ) ;
#22571 = CARTESIAN_POINT ( 'NONE',  ( 3.608439182435180470, -6.249999999999997335, -81.19198729810786119 ) ) ;
#22572 = VECTOR ( 'NONE', #21536, 1000.000000000000000 ) ;
#22573 = LINE ( 'NONE', #6410, #2359 ) ;
#22574 = ORIENTED_EDGE ( 'NONE', *, *, #21327, .F. ) ;
#22575 = CARTESIAN_POINT ( 'NONE',  ( -3.464101615137757051, -5.999999999999979572, -75.58632486540521711 ) ) ;
#22576 = AXIS2_PLACEMENT_3D ( 'NONE', #8765, #15405, #27463 ) ;
#22577 = ORIENTED_EDGE ( 'NONE', *, *, #13022, .F. ) ;
#22578 = ORIENTED_EDGE ( 'NONE', *, *, #9223, .F. ) ;
#22579 = CARTESIAN_POINT ( 'NONE',  ( 154.2187500000000284, 2.485281374238555774, -6.000000000000005329 ) ) ;
#22580 = CARTESIAN_POINT ( 'NONE',  ( -4.763139720814407951, 2.749999999999946709, -121.2500000000000284 ) ) ;
#22581 = EDGE_CURVE ( 'NONE', #8028, #4636, #4782, .T. ) ;
#22582 = CARTESIAN_POINT ( 'NONE',  ( -7.216878364870328078, 0.000000000000000000, -136.5580127018922099 ) ) ;
#22583 = CARTESIAN_POINT ( 'NONE',  ( 3.464101615137852974, 5.999999999999884537, -57.41367513459481842 ) ) ;
#22584 = CARTESIAN_POINT ( 'NONE',  ( 2.775557561562891351E-14, 6.250000000000033751, -127.0669872981078328 ) ) ;
#22585 = CARTESIAN_POINT ( 'NONE',  ( -3.608439182435115633, 6.249999999999965361, -177.9419872981078186 ) ) ;
#22586 = CARTESIAN_POINT ( 'NONE',  ( 3.175426480543072749, 5.499999999999865885, -174.1250000000000284 ) ) ;
#22587 = DIRECTION ( 'NONE',  ( -0.000000000000000000, -0.000000000000000000, -1.000000000000000000 ) ) ;
#22588 = EDGE_LOOP ( 'NONE', ( #29551, #23775, #5493, #16155 ) ) ;
#22589 = CYLINDRICAL_SURFACE ( 'NONE', #25983, 2.000000000000012879 ) ;
#22590 =( BOUNDED_CURVE ( )  B_SPLINE_CURVE ( 2, ( #13518, #21016, #22856, #18570, #6865, #15977, #2270, #28047, #11674 ),
 .UNSPECIFIED., .F., .T. ) 
 B_SPLINE_CURVE_WITH_KNOTS ( ( 3, 2, 2, 2, 3 ),
 ( 0.6972222222222222987, 0.6981481481481481843, 0.6999999999999999556, 0.7018518518518518379, 0.7027777777777777235 ),
 .UNSPECIFIED. ) 
 CURVE ( )  GEOMETRIC_REPRESENTATION_ITEM ( )  RATIONAL_B_SPLINE_CURVE ( ( 0.9330127018922194093, 0.9330127018922234061, 1.000000000000000000, 0.8660254037844388186, 1.000000000000000000, 0.8660254037844388186, 1.000000000000000000, 0.9330127018922234061, 0.9330127018922194093 ) ) 
 REPRESENTATION_ITEM ( '' )  );
#22591 = CARTESIAN_POINT ( 'NONE',  ( 159.8945522408903344, -11.49011212213293831, -3.498496789343953139 ) ) ;
#22592 = CARTESIAN_POINT ( 'NONE',  ( 6.000000000000000888, 1.607695154586715303, -171.5966878364870638 ) ) ;
#22593 = CARTESIAN_POINT ( 'NONE',  ( 5.196152422706629359, -2.999999999999988898, -46.71132486540518869 ) ) ;
#22594 = CARTESIAN_POINT ( 'NONE',  ( 112.0627832217620750, -0.7662911109077388261, -1.849990392679231599 ) ) ;
#22595 = CARTESIAN_POINT ( 'NONE',  ( -5.412658773652684552, -3.125000000000099920, -66.56698729810783277 ) ) ;
#22596 = CARTESIAN_POINT ( 'NONE',  ( 119.2113248654050466, -1.999999999999946265, 2.220446049250313081E-13 ) ) ;
#22597 = CARTESIAN_POINT ( 'NONE',  ( 4.763139720814407951, 2.750000000000002665, -52.75000000000002132 ) ) ;
#22598 = CARTESIAN_POINT ( 'NONE',  ( 5.196152422706629359, 3.000000000000002665, -56.03867513459481842 ) ) ;
#22599 = CARTESIAN_POINT ( 'NONE',  ( 5.999999999999999112, 2.951592740943527306E-14, -153.0863248654052313 ) ) ;
#22600 = CARTESIAN_POINT ( 'NONE',  ( 4.763139720814407951, 2.750000000000002665, -129.2500000000000284 ) ) ;
#22601 = CARTESIAN_POINT ( 'NONE',  ( 3.464101615137852974, 5.999999999999884537, -138.4136751345947971 ) ) ;
#22602 = VERTEX_POINT ( 'NONE', #11593 ) ;
#22603 = CARTESIAN_POINT ( 'NONE',  ( 23.31250000000007461, -1.097466725451379244, -2.649519052838478661 ) ) ;
#22604 = AXIS2_PLACEMENT_3D ( 'NONE', #11088, #1690, #15874 ) ;
#22605 = DIRECTION ( 'NONE',  ( 5.551115123125785167E-17, -1.000000000000000000, -8.881784197001256268E-16 ) ) ;
#22606 = DIRECTION ( 'NONE',  ( -7.147005652999508048E-36, 5.642372883946980038E-36, 1.000000000000000000 ) ) ;
#22607 = CARTESIAN_POINT ( 'NONE',  ( 140.7336002691896795, -4.999999999999989342, 2.071067811865468400 ) ) ;
#22608 = ORIENTED_EDGE ( 'NONE', *, *, #3574, .F. ) ;
#22609 = CARTESIAN_POINT ( 'NONE',  ( 114.2497167782375698, -1.308140751793557266, -1.308140751793640533 ) ) ;
#22610 = CARTESIAN_POINT ( 'NONE',  ( 10.60117513459496408, -1.035533905932629173, 2.499999999999964473 ) ) ;
#22611 = CARTESIAN_POINT ( 'NONE',  ( -11.00000000000001599, 1.957734142605926671E-15, 1.386142938489641429E-34 ) ) ;
#22612 = EDGE_CURVE ( 'NONE', #14180, #2929, #25358, .T. ) ;
#22613 = CARTESIAN_POINT ( 'NONE',  ( -3.608439182435115633, 6.249999999999965361, -119.4419872981078612 ) ) ;
#22614 = CARTESIAN_POINT ( 'NONE',  ( -3.464101615137757051, -5.999999999999979572, -110.0863248654051887 ) ) ;
#22615 = CARTESIAN_POINT ( 'NONE',  ( 10.00000000000009237, 2.022486306914408782, 0.1720805556212724186 ) ) ;
#22616 = VERTEX_POINT ( 'NONE', #2343 ) ;
#22617 = DIRECTION ( 'NONE',  ( -1.000000000000000000, -0.000000000000000000, -0.000000000000000000 ) ) ;
#22618 = CARTESIAN_POINT ( 'NONE',  ( 141.1875000000000284, 4.242640687119269671, 4.242640687119298093 ) ) ;
#22619 = COLOUR_RGB ( '', 0.08235294, 0.09019608, 0.10196078) ;
#22620 = EDGE_CURVE ( 'NONE', #6123, #3196, #24006, .T. ) ;
#22621 = VECTOR ( 'NONE', #15832, 1000.000000000000000 ) ;
#22622 = ORIENTED_EDGE ( 'NONE', *, *, #29407, .F. ) ;
#22623 = VERTEX_POINT ( 'NONE', #13592 ) ;
#22624 = DIRECTION ( 'NONE',  ( -7.147005652999508048E-36, 5.642372883946980038E-36, 1.000000000000000000 ) ) ;
#22625 = CARTESIAN_POINT ( 'NONE',  ( 24.12500000000009237, 1.414213562373201061, 1.414213562373034527 ) ) ;
#22626 =( NAMED_UNIT ( * ) PLANE_ANGLE_UNIT ( ) SI_UNIT ( $, .RADIAN. ) );
#22627 = DIRECTION ( 'NONE',  ( -0.000000000000000000, 0.000000000000000000, 1.000000000000000000 ) ) ;
#22628 = CARTESIAN_POINT ( 'NONE',  ( -3.608439182435115633, 6.249999999999965361, -69.30801270189220986 ) ) ;
#22629 = CARTESIAN_POINT ( 'NONE',  ( 151.1101497308104058, 3.535533905932725318, 3.535533905932725318 ) ) ;
#22630 = CARTESIAN_POINT ( 'NONE',  ( 5.196152422706629359, 3.000000000000002665, -102.5386751345948539 ) ) ;
#22631 = DIRECTION ( 'NONE',  ( 1.000000000000000000, -5.551115123125773458E-17, -1.260129944081490338E-35 ) ) ;
#22632 = CARTESIAN_POINT ( 'NONE',  ( 0.000000000000000000, 5.499999999999991118, -130.5000000000000000 ) ) ;
#22633 = CARTESIAN_POINT ( 'NONE',  ( 14.16367513459490546, 1.767766952966487448, -1.767766952966487448 ) ) ;
#22634 = EDGE_LOOP ( 'NONE', ( #22486, #20232, #27285, #26682 ) ) ;
#22635 = APPLICATION_CONTEXT ( 'automotive_design' ) ;
#22636 = CARTESIAN_POINT ( 'NONE',  ( -3.175426480542816066, -5.500000000000057732, -62.37500000000001421 ) ) ;
#22637 = CARTESIAN_POINT ( 'NONE',  ( 1.000000000000000888, 0.000000000000000000, 0.000000000000000000 ) ) ;
#22638 = CARTESIAN_POINT ( 'NONE',  ( 0.000000000000000000, 5.999999999999977796, -70.21132486540521711 ) ) ;
#22639 = PRESENTATION_STYLE_ASSIGNMENT (( #13297 ) ) ;
#22640 = ORIENTED_EDGE ( 'NONE', *, *, #27092, .T. ) ;
#22641 = CARTESIAN_POINT ( 'NONE',  ( 109.1249999999999289, 1.767766952966265404, 1.767766952966431937 ) ) ;
#22642 = CARTESIAN_POINT ( 'NONE',  ( 148.5000000000000284, 6.000000000000005329, 0.000000000000000000 ) ) ;
#22643 = CARTESIAN_POINT ( 'NONE',  ( -4.999999999999886313, -9.000000000000007105, 4.000000000000003553 ) ) ;
#22644 = CIRCLE ( 'NONE', #2024, 14.49999999999998579 ) ;
#22645 = EDGE_CURVE ( 'NONE', #9814, #8182, #3568, .T. ) ;
#22646 = CARTESIAN_POINT ( 'NONE',  ( 140.0769230769231228, -11.53846153846155254, -4.615384615384604317 ) ) ;
#22647 = VERTEX_POINT ( 'NONE', #8800 ) ;
#22648 = CARTESIAN_POINT ( 'NONE',  ( 139.5937500000000284, 6.000000000000005329, 2.485281374238585972 ) ) ;
#22649 = CARTESIAN_POINT ( 'NONE',  ( 161.1633582548628567, -2.175497436150891417, 5.238395570785098876 ) ) ;
#22650 = ORIENTED_EDGE ( 'NONE', *, *, #26065, .F. ) ;
#22651 = EDGE_CURVE ( 'NONE', #20198, #22270, #18795, .T. ) ;
#22652 = CARTESIAN_POINT ( 'NONE',  ( 4.763139720814407951, 2.750000000000002665, -148.7500000000000568 ) ) ;
#22653 = CARTESIAN_POINT ( 'NONE',  ( 14.12500000000013678, 1.414213562373201061, 1.414213562373034527 ) ) ;
#22654 = ORIENTED_EDGE ( 'NONE', *, *, #6677, .F. ) ;
#22655 = CARTESIAN_POINT ( 'NONE',  ( -4.763139720814407951, -2.750000000000016431, -77.50000000000001421 ) ) ;
#22656 = AXIS2_PLACEMENT_3D ( 'NONE', #4479, #11275, #16504 ) ;
#22657 = CARTESIAN_POINT ( 'NONE',  ( 14.31250000000002132, 2.649519052838298805, -1.097466725451559322 ) ) ;
#22658 = CARTESIAN_POINT ( 'NONE',  ( 3.608439182435180470, -6.249999999999997335, -95.55801270189226670 ) ) ;
#22659 = CARTESIAN_POINT ( 'NONE',  ( -5.197786390520544586, -9.697480688945354643, -28.02189831943639220 ) ) ;
#22660 = DIRECTION ( 'NONE',  ( -7.147005652999508048E-36, 5.642372883946980038E-36, 1.000000000000000000 ) ) ;
#22661 = CARTESIAN_POINT ( 'NONE',  ( 5.999999999999949374, 1.607695154586804565, -99.01933756729741276 ) ) ;
#22662 = CARTESIAN_POINT ( 'NONE',  ( -5.999999999999963585, 1.780251999655701777E-13, -65.33632486540521711 ) ) ;
#22663 = CARTESIAN_POINT ( 'NONE',  ( 4.763139720814407951, -2.749999999999988454, -156.5000000000000284 ) ) ;
#22664 = CARTESIAN_POINT ( 'NONE',  ( 0.000000000000000000, -14.14213562373095634, -8.500000000000007105 ) ) ;
#22665 = AXIS2_PLACEMENT_3D ( 'NONE', #26306, #9748, #23868 ) ;
#22666 = CARTESIAN_POINT ( 'NONE',  ( 3.175426480543072749, -5.500000000000105693, -84.62499999999997158 ) ) ;
#22667 = CARTESIAN_POINT ( 'NONE',  ( -5.999999999999963585, -1.487416814333745711E-14, -154.4136751345947971 ) ) ;
#22668 = CARTESIAN_POINT ( 'NONE',  ( 117.0238248654050324, -0.8284271247462354770, 2.000000000000212275 ) ) ;
#22669 = CARTESIAN_POINT ( 'NONE',  ( -6.350852961085760029, -1.281975124255709124E-13, -74.62500000000000000 ) ) ;
#22670 = DIRECTION ( 'NONE',  ( 1.000000000000000000, -0.000000000000000000, -0.000000000000000000 ) ) ;
#22671 = CARTESIAN_POINT ( 'NONE',  ( 154.1398502691896510, -3.535533905932752852, 3.535533905932725318 ) ) ;
#22672 = CARTESIAN_POINT ( 'NONE',  ( -5.999999999999963585, 8.134310703387671600E-14, -140.3363248654052313 ) ) ;
#22673 = DIRECTION ( 'NONE',  ( 5.551115123125785167E-17, -1.000000000000000000, -8.881784197001256268E-16 ) ) ;
#22674 = CARTESIAN_POINT ( 'NONE',  ( 20.93750000000008171, 2.000000000000212275, -0.8284271247463557142 ) ) ;
#22675 = CARTESIAN_POINT ( 'NONE',  ( 140.7917870674316987, -11.58357413486331566, -4.000000000000005329 ) ) ;
#22676 = AXIS2_PLACEMENT_3D ( 'NONE', #4394, #4089, #27886 ) ;
#22677 = EDGE_CURVE ( 'NONE', #20342, #16115, #22779, .T. ) ;
#22678 = CYLINDRICAL_SURFACE ( 'NONE', #9731, 6.000000000000000888 ) ;
#22679 = CARTESIAN_POINT ( 'NONE',  ( -5.196152422706601826, 2.999999999999975131, -174.0386751345948255 ) ) ;
#22680 = EDGE_CURVE ( 'NONE', #899, #25744, #4173, .T. ) ;
#22681 =( BOUNDED_CURVE ( )  B_SPLINE_CURVE ( 2, ( #27298, #9191, #18430, #8577, #18585, #22575, #3804, #13232, #22873 ),
 .UNSPECIFIED., .F., .T. ) 
 B_SPLINE_CURVE_WITH_KNOTS ( ( 3, 2, 2, 2, 3 ),
 ( 0.2138888888888887951, 0.2148148148148147918, 0.2166666666666666741, 0.2185185185185185563, 0.2194444444444444420 ),
 .UNSPECIFIED. ) 
 CURVE ( )  GEOMETRIC_REPRESENTATION_ITEM ( )  RATIONAL_B_SPLINE_CURVE ( ( 0.9330127018922194093, 0.9330127018922154125, 1.000000000000000000, 0.8660254037844388186, 1.000000000000000000, 0.8660254037844388186, 1.000000000000000000, 0.9330127018922194093, 0.9330127018922194093 ) ) 
 REPRESENTATION_ITEM ( '' )  );
#22682 = EDGE_LOOP ( 'NONE', ( #24027, #14619, #6771, #22275 ) ) ;
#22683 = PRODUCT_DEFINITION ( 'UNKNOWN', '', #15911, #14383 ) ;
#22684 = CARTESIAN_POINT ( 'NONE',  ( 156.4687500000000284, -2.485281374238585972, 6.000000000000005329 ) ) ;
#22685 = DIRECTION ( 'NONE',  ( -0.000000000000000000, -0.4000000000000005773, -0.9165151389911678770 ) ) ;
#22686 = CARTESIAN_POINT ( 'NONE',  ( 116.1877832217621886, 0.7662911109078888172, -1.849990392679291551 ) ) ;
#22687 = CARTESIAN_POINT ( 'NONE',  ( 6.000000000000052403, -1.607695154586662678, -115.6533121635129930 ) ) ;
#22688 = EDGE_LOOP ( 'NONE', ( #19001, #22724, #17185, #17534 ) ) ;
#22689 = EDGE_LOOP ( 'NONE', ( #16901, #12301, #9544 ) ) ;
#22690 = CARTESIAN_POINT ( 'NONE',  ( 3.175426480543072749, -5.500000000000105693, -93.62500000000002842 ) ) ;
#22691 = DIRECTION ( 'NONE',  ( 5.551115123125785167E-17, -1.000000000000000000, -8.881784197001256268E-16 ) ) ;
#22692 = CARTESIAN_POINT ( 'NONE',  ( -7.216878364870328078, 0.000000000000000000, -118.5580127018922525 ) ) ;
#22693 = VERTEX_POINT ( 'NONE', #18344 ) ;
#22694 = CARTESIAN_POINT ( 'NONE',  ( 6.000000000000000888, 7.762456499804234384E-14, -123.6636751345948255 ) ) ;
#22695 = CARTESIAN_POINT ( 'NONE',  ( 139.7945697293052660, -8.829120115006070080, -8.127272355818778493 ) ) ;
#22696 = CARTESIAN_POINT ( 'NONE',  ( -3.464101615137725076, 5.999999999999979572, -52.08632486540516737 ) ) ;
#22697 = CARTESIAN_POINT ( 'NONE',  ( -7.216878364870328078, 0.000000000000000000, -55.55801270189220986 ) ) ;
#22698 = ORIENTED_EDGE ( 'NONE', *, *, #19693, .F. ) ;
#22699 = B_SPLINE_CURVE_WITH_KNOTS ( 'NONE', 3,
 ( #12676, #3708, #22169, #15439, #8323, #1103, #10501, #19854, #10977, #27210, #5554, #8163 ),
 .UNSPECIFIED., .F., .F.,
 ( 4, 2, 2, 2, 2, 4 ),
 ( 0.000000000000000000, 0.0002753300403215867896, 0.0005506600806431735792, 0.001101320161286347158, 0.001651980241929520629, 0.002202640322572694317 ),
 .UNSPECIFIED. ) ;
#22700 = SURFACE_SIDE_STYLE ('',( #30207 ) ) ;
#22701 = CARTESIAN_POINT ( 'NONE',  ( 0.000000000000000000, -5.999999999999991118, -166.9613248654052029 ) ) ;
#22702 = CARTESIAN_POINT ( 'NONE',  ( -4.763139720814407951, -2.750000000000016431, -160.0000000000000284 ) ) ;
#22703 = CARTESIAN_POINT ( 'NONE',  ( 117.8124999999998579, 1.035533905932869425, -2.499999999999784173 ) ) ;
#22704 = CARTESIAN_POINT ( 'NONE',  ( 0.000000000000000000, 0.000000000000000000, 0.000000000000000000 ) ) ;
#22705 = CARTESIAN_POINT ( 'NONE',  ( -3.175426480542816066, 5.499999999999865885, -109.3750000000000426 ) ) ;
#22706 = CARTESIAN_POINT ( 'NONE',  ( 106.2886751345948255, 2.000000000000029310, 1.110223024625156540E-13 ) ) ;
#22707 = CARTESIAN_POINT ( 'NONE',  ( 145.5863248654052313, 0.000000000000000000, 5.500000000000005329 ) ) ;
#22708 = CARTESIAN_POINT ( 'NONE',  ( -4.763139720814407951, -2.750000000000016431, -100.0000000000000284 ) ) ;
#22709 = PRESENTATION_LAYER_ASSIGNMENT (  '', '', ( #30058 ) ) ;
#22710 = CARTESIAN_POINT ( 'NONE',  ( -3.464101615137725076, 5.999999999999979572, -118.0863248654052029 ) ) ;
#22711 = ORIENTED_EDGE ( 'NONE', *, *, #18246, .F. ) ;
#22712 = CARTESIAN_POINT ( 'NONE',  ( 15.43750000000003730, 1.097466725451559322, -2.649519052838298805 ) ) ;
#22713 = CARTESIAN_POINT ( 'NONE',  ( 109.0002832217621034, -1.308140751793640533, -1.308140751793640533 ) ) ;
#22714 = DIRECTION ( 'NONE',  ( 1.000000000000000000, -0.000000000000000000, -0.000000000000000000 ) ) ;
#22715 = EDGE_CURVE ( 'NONE', #9072, #10931, #12647, .T. ) ;
#22716 = VERTEX_POINT ( 'NONE', #27659 ) ;
#22717 = CARTESIAN_POINT ( 'NONE',  ( -5.196152422706573404, -3.000000000000002665, -170.2113248654052313 ) ) ;
#22718 = CARTESIAN_POINT ( 'NONE',  ( 3.608439182435180470, 6.249999999999982236, -88.19198729810783277 ) ) ;
#22719 = CARTESIAN_POINT ( 'NONE',  ( 135.6566535407617948, -9.123793365789319765, 8.000000000000007105 ) ) ;
#22720 = ORIENTED_EDGE ( 'NONE', *, *, #3779, .F. ) ;
#22721 = DIRECTION ( 'NONE',  ( 1.000000000000000000, -5.551115123125773458E-17, -1.260129944081490338E-35 ) ) ;
#22722 = VECTOR ( 'NONE', #19967, 1000.000000000000000 ) ;
#22723 = EDGE_LOOP ( 'NONE', ( #13720, #28808, #25595, #23191 ) ) ;
#22724 = ORIENTED_EDGE ( 'NONE', *, *, #12067, .F. ) ;
#22725 = CARTESIAN_POINT ( 'NONE',  ( 157.2187500000000284, 2.485281374238555774, -6.000000000000005329 ) ) ;
#22726 =( BOUNDED_CURVE ( )  B_SPLINE_CURVE ( 2, ( #667, #19571, #951, #28600, #16838, #5560, #15119, #8024, #7568 ),
 .UNSPECIFIED., .F., .F. ) 
 B_SPLINE_CURVE_WITH_KNOTS ( ( 3, 2, 2, 2, 3 ),
 ( 0.9638888888888889062, 0.9648148148148147918, 0.9666666666666666741, 0.9685185185185185563, 0.9694444444444444420 ),
 .UNSPECIFIED. ) 
 CURVE ( )  GEOMETRIC_REPRESENTATION_ITEM ( )  RATIONAL_B_SPLINE_CURVE ( ( 0.9330127018922194093, 0.9330127018922234061, 1.000000000000000000, 0.8660254037844388186, 1.000000000000000000, 0.8660254037844388186, 1.000000000000000000, 0.9330127018922194093, 0.9330127018922194093 ) ) 
 REPRESENTATION_ITEM ( '' )  );
#22727 = CARTESIAN_POINT ( 'NONE',  ( 6.350852961086080661, -9.614813431917819062E-14, -118.8750000000000142 ) ) ;
#22728 = CARTESIAN_POINT ( 'NONE',  ( 3.608439182435180470, 6.249999999999982236, -141.5580127018922099 ) ) ;
#22729 = VERTEX_POINT ( 'NONE', #23091 ) ;
#22730 = CARTESIAN_POINT ( 'NONE',  ( 151.3199251345948255, -2.278174593051950136, -5.500000000000074607 ) ) ;
#22731 = CARTESIAN_POINT ( 'NONE',  ( 2.775557561562891351E-14, -6.250000000000061284, -120.3169872981078043 ) ) ;
#22732 = CARTESIAN_POINT ( 'NONE',  ( 3.608439182435180470, -6.249999999999997335, -174.1919872981077901 ) ) ;
#22733 = CARTESIAN_POINT ( 'NONE',  ( -4.763139720814407951, -2.750000000000016431, -172.0000000000000284 ) ) ;
#22734 = CARTESIAN_POINT ( 'NONE',  ( 159.6227035152770668, -12.16574911538731740, 3.793091317978431576 ) ) ;
#22735 = CARTESIAN_POINT ( 'NONE',  ( 20.27382486540532014, -2.499999999999844569, -1.035533905932809473 ) ) ;
#22736 = ORIENTED_EDGE ( 'NONE', *, *, #24418, .F. ) ;
#22737 = CARTESIAN_POINT ( 'NONE',  ( 12.06249999999996447, 2.000000000000091926, 0.8284271247461753029 ) ) ;
#22738 = CARTESIAN_POINT ( 'NONE',  ( 3.464101615137852974, 5.999999999999884537, -163.9136751345947971 ) ) ;
#22739 = CARTESIAN_POINT ( 'NONE',  ( 159.5364582854214746, -11.09853219182770090, -4.564322074144446795 ) ) ;
#22740 = DIRECTION ( 'NONE',  ( -0.000000000000000000, -0.000000000000000000, -1.000000000000000000 ) ) ;
#22741 = CARTESIAN_POINT ( 'NONE',  ( 0.000000000000000000, 0.000000000000000000, -180.0000000000000568 ) ) ;
#22742 = CARTESIAN_POINT ( 'NONE',  ( 110.0627832217622313, -0.7662911109076785410, -1.849990392679171425 ) ) ;
#22743 = CARTESIAN_POINT ( 'NONE',  ( -5.412658773652684552, -3.125000000000099920, -77.06698729810779014 ) ) ;
#22744 = CARTESIAN_POINT ( 'NONE',  ( 3.608439182435180470, -6.249999999999997335, -55.69198729810780435 ) ) ;
#22745 = EDGE_CURVE ( 'NONE', #25700, #24608, #20786, .T. ) ;
#22746 = CARTESIAN_POINT ( 'NONE',  ( 119.5863248654052029, 1.414213562373145550, -1.414213562373034527 ) ) ;
#22747 = CARTESIAN_POINT ( 'NONE',  ( 3.175426480543072749, -5.500000000000105693, -53.12500000000002842 ) ) ;
#22748 = CARTESIAN_POINT ( 'NONE',  ( 119.9999999999998579, 0.6961469067503631702, -2.048720570868077573 ) ) ;
#22749 = FACE_OUTER_BOUND ( 'NONE', #717, .T. ) ;
#22750 = CARTESIAN_POINT ( 'NONE',  ( -4.763139720814407951, 2.749999999999946709, -128.7500000000000284 ) ) ;
#22751 = AXIS2_PLACEMENT_3D ( 'NONE', #21550, #4933, #25529 ) ;
#22752 = AXIS2_PLACEMENT_3D ( 'NONE', #6330, #3717, #13148 ) ;
#22753 = ORIENTED_EDGE ( 'NONE', *, *, #1551, .F. ) ;
#22754 = CARTESIAN_POINT ( 'NONE',  ( 6.000000000000000888, 7.762456499804234384E-14, -118.5863248654052313 ) ) ;
#22755 = CARTESIAN_POINT ( 'NONE',  ( 17.60117513459492500, -1.035533905932629173, 2.499999999999784173 ) ) ;
#22756 = CARTESIAN_POINT ( 'NONE',  ( 140.2648502691896795, 3.535533905932725318, 3.535533905932752852 ) ) ;
#22757 = EDGE_CURVE ( 'NONE', #17555, #27766, #18492, .T. ) ;
#22758 = VERTEX_POINT ( 'NONE', #4480 ) ;
#22759 = CARTESIAN_POINT ( 'NONE',  ( 109.3747167782375556, -1.665334536937734811E-13, -1.849990392679523588 ) ) ;
#22760 = CARTESIAN_POINT ( 'NONE',  ( 9.812500000000115463, 0.8284271247462955401, -2.000000000000091926 ) ) ;
#22761 = CARTESIAN_POINT ( 'NONE',  ( -5.412658773652739619, 3.124999999999975131, -117.8169872981078612 ) ) ;
#22762 = CARTESIAN_POINT ( 'NONE',  ( 104.7401757384974559, 1.799749494549046203, 0.4423533583444329009 ) ) ;
#22763 = ORIENTED_EDGE ( 'NONE', *, *, #25836, .F. ) ;
#22764 = CARTESIAN_POINT ( 'NONE',  ( 6.000000000000000888, -3.330669073875464691E-16, -7.560779664488942560E-35 ) ) ;
#22765 = CARTESIAN_POINT ( 'NONE',  ( 139.2187500000000000, 2.485281374238555774, -6.000000000000005329 ) ) ;
#22766 =( BOUNDED_CURVE ( )  B_SPLINE_CURVE ( 2, ( #23583, #214, #29795, #15879, #11092, #17550, #15722, #3525, #3677 ),
 .UNSPECIFIED., .F., .T. ) 
 B_SPLINE_CURVE_WITH_KNOTS ( ( 3, 2, 2, 2, 3 ),
 ( 0.3638888888888889284, 0.3648148148148148140, 0.3666666666666666408, 0.3685185185185185230, 0.3694444444444444087 ),
 .UNSPECIFIED. ) 
 CURVE ( )  GEOMETRIC_REPRESENTATION_ITEM ( )  RATIONAL_B_SPLINE_CURVE ( ( 0.9330127018922194093, 0.9330127018922214077, 1.000000000000000000, 0.8660254037844388186, 1.000000000000000000, 0.8660254037844388186, 1.000000000000000000, 0.9330127018922214077, 0.9330127018922194093 ) ) 
 REPRESENTATION_ITEM ( '' )  );
#22767 = EDGE_LOOP ( 'NONE', ( #7184, #6949 ) ) ;
#22768 = ORIENTED_EDGE ( 'NONE', *, *, #9855, .T. ) ;
#22769 = CARTESIAN_POINT ( 'NONE',  ( -4.763139720814407951, 2.749999999999946709, -50.75000000000001421 ) ) ;
#22770 = CARTESIAN_POINT ( 'NONE',  ( 24.62500000000012079, -1.414213562372923505, -1.414213562373145550 ) ) ;
#22771 = CARTESIAN_POINT ( 'NONE',  ( 117.4761751345945839, 0.8284271247463257382, 2.000000000000151879 ) ) ;
#22772 = CARTESIAN_POINT ( 'NONE',  ( 105.1488248654049329, -1.999999999999941602, 0.8284271247463557142 ) ) ;
#22773 = CARTESIAN_POINT ( 'NONE',  ( -3.608439182435115633, 6.249999999999965361, -64.80801270189225249 ) ) ;
#22774 = CARTESIAN_POINT ( 'NONE',  ( 135.1084928141376054, -8.790281914029968391, -8.000000000000007105 ) ) ;
#22775 =( BOUNDED_CURVE ( )  B_SPLINE_CURVE ( 2, ( #21394, #25982, #9867, #4926, #7535, #5225, #2925, #3074, #19390 ),
 .UNSPECIFIED., .F., .T. ) 
 B_SPLINE_CURVE_WITH_KNOTS ( ( 3, 2, 2, 2, 3 ),
 ( 0.7138888888888887951, 0.7148148148148147918, 0.7166666666666666741, 0.7185185185185185563, 0.7194444444444444420 ),
 .UNSPECIFIED. ) 
 CURVE ( )  GEOMETRIC_REPRESENTATION_ITEM ( )  RATIONAL_B_SPLINE_CURVE ( ( 0.9330127018922194093, 0.9330127018922114157, 1.000000000000000000, 0.8660254037844388186, 1.000000000000000000, 0.8660254037844388186, 1.000000000000000000, 0.9330127018922194093, 0.9330127018922194093 ) ) 
 REPRESENTATION_ITEM ( '' )  );
#22776 = CARTESIAN_POINT ( 'NONE',  ( 149.6101497308104058, 3.535533905932725318, 3.535533905932725318 ) ) ;
#22777 = CYLINDRICAL_SURFACE ( 'NONE', #11931, 6.000000000000000888 ) ;
#22778 = CARTESIAN_POINT ( 'NONE',  ( -5.999999999999963585, 1.780251999655701777E-13, -107.3363248654052455 ) ) ;
#22779 = LINE ( 'NONE', #1720, #7485 ) ;
#22780 = ADVANCED_FACE ( 'NONE', ( #2187 ), #1612, .T. ) ;
#22781 = CARTESIAN_POINT ( 'NONE',  ( -5.999999999999963585, -1.487416814333745711E-14, -67.41367513459481131 ) ) ;
#22782 = CARTESIAN_POINT ( 'NONE',  ( -3.175426480542816066, -5.500000000000057732, -125.3749999999999858 ) ) ;
#22783 = CARTESIAN_POINT ( 'NONE',  ( 137.6324251345948255, -5.500000000000012434, -2.278174593052012309 ) ) ;
#22784 = CARTESIAN_POINT ( 'NONE',  ( 5.412658773652712085, -3.125000000000086153, -146.4330127018922383 ) ) ;
#22785 = CARTESIAN_POINT ( 'NONE',  ( 14.10117513459491612, 1.035533905932929599, -2.500000000000024425 ) ) ;
#22786 = ORIENTED_EDGE ( 'NONE', *, *, #1788, .T. ) ;
#22787 = CARTESIAN_POINT ( 'NONE',  ( -3.175426480542816066, -5.500000000000057732, -65.37500000000001421 ) ) ;
#22788 = CARTESIAN_POINT ( 'NONE',  ( -5.196152422706601826, 2.999999999999975131, -123.9613248654052313 ) ) ;
#22789 = EDGE_CURVE ( 'NONE', #3881, #16950, #30286, .T. ) ;
#22790 = LINE ( 'NONE', #25217, #1739 ) ;
#22791 = CARTESIAN_POINT ( 'NONE',  ( 0.000000000000000000, 0.000000000000000000, 0.000000000000000000 ) ) ;
#22792 = ORIENTED_EDGE ( 'NONE', *, *, #3431, .F. ) ;
#22793 = EDGE_CURVE ( 'NONE', #27302, #15456, #9304, .T. ) ;
#22794 = CARTESIAN_POINT ( 'NONE',  ( 107.4374999999997868, -2.499999999999964473, 1.035533905932989551 ) ) ;
#22795 = CARTESIAN_POINT ( 'NONE',  ( 144.1875000000000284, 4.242640687119269671, 4.242640687119298093 ) ) ;
#22796 = LINE ( 'NONE', #3725, #16821 ) ;
#22797 = CARTESIAN_POINT ( 'NONE',  ( 13.37500000000019185, -1.414213562372979016, 1.414213562372979016 ) ) ;
#22798 = CARTESIAN_POINT ( 'NONE',  ( -5.999999999999963585, 1.780251999655701777E-13, -49.41367513459484684 ) ) ;
#22799 = CARTESIAN_POINT ( 'NONE',  ( 136.0312500000000000, -2.485281374238555774, -6.000000000000005329 ) ) ;
#22800 = CARTESIAN_POINT ( 'NONE',  ( 14.02382486540528816, -1.035533905932568999, 2.499999999999784173 ) ) ;
#22801 = VERTEX_POINT ( 'NONE', #12048 ) ;
#22802 = CARTESIAN_POINT ( 'NONE',  ( -6.350852961085760029, -1.281975124255709124E-13, -146.6250000000000284 ) ) ;
#22803 = CARTESIAN_POINT ( 'NONE',  ( 12.06249999999996447, 2.000000000000091926, 0.8284271247461753029 ) ) ;
#22804 = ORIENTED_EDGE ( 'NONE', *, *, #21365, .T. ) ;
#22805 = CARTESIAN_POINT ( 'NONE',  ( 4.763139720814407951, -2.749999999999988454, -74.00000000000001421 ) ) ;
#22806 = CARTESIAN_POINT ( 'NONE',  ( 10.00000000000014921, 0.7338214498545042597, -2.235074556132228274 ) ) ;
#22807 = CARTESIAN_POINT ( 'NONE',  ( 5.412658773652712085, -3.125000000000086153, -87.93301270189223828 ) ) ;
#22808 = CARTESIAN_POINT ( 'NONE',  ( -5.681812044562425612, -9.420575401947244742, -23.03339967402432720 ) ) ;
#22809 = EDGE_CURVE ( 'NONE', #29768, #13111, #28563, .T. ) ;
#22810 = FACE_OUTER_BOUND ( 'NONE', #17226, .T. ) ;
#22811 = CARTESIAN_POINT ( 'NONE',  ( 114.7113248654050750, 2.000000000000057288, 0.000000000000000000 ) ) ;
#22812 = SHAPE_DEFINITION_REPRESENTATION ( #11157, #103 ) ;
#22813 = CARTESIAN_POINT ( 'NONE',  ( -4.763139720814407951, -2.750000000000016431, -155.5000000000000284 ) ) ;
#22814 = CARTESIAN_POINT ( 'NONE',  ( 19.16367513459482552, 1.767766952966376426, -1.767766952966431937 ) ) ;
#22815 = CARTESIAN_POINT ( 'NONE',  ( -5.999999999999963585, 1.780251999655701777E-13, -82.41367513459481131 ) ) ;
#22816 = CARTESIAN_POINT ( 'NONE',  ( -4.763139720814407951, 2.749999999999946709, -89.75000000000000000 ) ) ;
#22817 = FACE_OUTER_BOUND ( 'NONE', #6775, .T. ) ;
#22818 = EDGE_CURVE ( 'NONE', #7192, #11887, #2278, .T. ) ;
#22819 = CARTESIAN_POINT ( 'NONE',  ( 3.175426480543072749, -5.500000000000105693, -77.12500000000001421 ) ) ;
#22820 = EDGE_CURVE ( 'NONE', #11247, #6328, #19534, .T. ) ;
#22821 = CARTESIAN_POINT ( 'NONE',  ( 148.8898502691896510, 3.535533905932725318, -3.535533905932725318 ) ) ;
#22822 = CARTESIAN_POINT ( 'NONE',  ( 6.000000000000000888, 5.577813053751546416E-15, -165.0863248654052029 ) ) ;
#22823 = CARTESIAN_POINT ( 'NONE',  ( 6.000000000000001776, 5.345404176511898156E-15, -174.6636751345948539 ) ) ;
#22824 = DIRECTION ( 'NONE',  ( 0.000000000000000000, -5.551115123125768527E-17, 1.000000000000000000 ) ) ;
#22825 = CARTESIAN_POINT ( 'NONE',  ( 0.000000000000000000, 0.000000000000000000, 0.000000000000000000 ) ) ;
#22826 = AXIS2_PLACEMENT_3D ( 'NONE', #13997, #6725, #29909 ) ;
#22827 = CARTESIAN_POINT ( 'NONE',  ( -5.999999999999963585, -1.487416814333745711E-14, -54.83632486540523132 ) ) ;
#22828 = CARTESIAN_POINT ( 'NONE',  ( -5.999999999999963585, -1.487416814333745711E-14, -134.3363248654052313 ) ) ;
#22829 = CARTESIAN_POINT ( 'NONE',  ( 6.000000000000000888, 1.607695154586715303, -170.0966878364870354 ) ) ;
#22830 = VERTEX_POINT ( 'NONE', #5221 ) ;
#22831 = CARTESIAN_POINT ( 'NONE',  ( 155.7187500000000568, 2.485281374238555774, -6.000000000000005329 ) ) ;
#22832 = CARTESIAN_POINT ( 'NONE',  ( -6.000000000000007105, -1.607695154586655129, -109.3466878364870354 ) ) ;
#22833 = CARTESIAN_POINT ( 'NONE',  ( 117.7502832217623592, -1.308140751793585022, 1.308140751793862577 ) ) ;
#22834 = CARTESIAN_POINT ( 'NONE',  ( -5.196152422706601826, 2.999999999999975131, -156.9613248654052597 ) ) ;
#22835 = EDGE_LOOP ( 'NONE', ( #5041, #24776, #3611, #20489 ) ) ;
#22836 = VECTOR ( 'NONE', #19913, 1000.000000000000000 ) ;
#22837 = ORIENTED_EDGE ( 'NONE', *, *, #3467, .F. ) ;
#22838 = ORIENTED_EDGE ( 'NONE', *, *, #14124, .T. ) ;
#22839 = CARTESIAN_POINT ( 'NONE',  ( -2.775557561562891351E-14, -5.500000000000115463, -101.2500000000000000 ) ) ;
#22840 = CARTESIAN_POINT ( 'NONE',  ( 116.0000000000000142, 0.000000000000000000, -5.500000000000000000 ) ) ;
#22841 = CARTESIAN_POINT ( 'NONE',  ( 3.608439182435180470, -6.249999999999997335, -104.5580127018922525 ) ) ;
#22842 = VERTEX_POINT ( 'NONE', #21388 ) ;
#22843 = CARTESIAN_POINT ( 'NONE',  ( 0.1999138633143864585, 11.00000000000000533, -19.00000000000001066 ) ) ;
#22844 = DIRECTION ( 'NONE',  ( -1.000000000000000000, -0.000000000000000000, -0.000000000000000000 ) ) ;
#22845 = AXIS2_PLACEMENT_3D ( 'NONE', #17474, #8534, #8696 ) ;
#22846 = CARTESIAN_POINT ( 'NONE',  ( 3.175426480543072749, 5.499999999999865885, -163.6249999999999716 ) ) ;
#22847 = EDGE_CURVE ( 'NONE', #2600, #18174, #467, .T. ) ;
#22848 = DIRECTION ( 'NONE',  ( -7.147005652999508048E-36, 5.642372883946980038E-36, 1.000000000000000000 ) ) ;
#22849 = ORIENTED_EDGE ( 'NONE', *, *, #25577, .F. ) ;
#22850 = CARTESIAN_POINT ( 'NONE',  ( -5.196152422706601826, 2.999999999999975131, -153.0386751345948539 ) ) ;
#22851 = CARTESIAN_POINT ( 'NONE',  ( 159.0000000000000284, -11.31370849898477537, 4.000000000000003553 ) ) ;
#22852 = CARTESIAN_POINT ( 'NONE',  ( -4.763139720814407951, -2.750000000000016431, -166.0000000000000284 ) ) ;
#22853 = CARTESIAN_POINT ( 'NONE',  ( 117.7499999999998721, 1.387778780781445676E-13, -2.499999999999835687 ) ) ;
#22854 = CARTESIAN_POINT ( 'NONE',  ( 3.175426480543072749, -5.500000000000105693, -105.6250000000000284 ) ) ;
#22855 = CARTESIAN_POINT ( 'NONE',  ( 23.58632486540529527, 1.767766952966431937, -1.767766952966431937 ) ) ;
#22856 = CARTESIAN_POINT ( 'NONE',  ( 5.196152422706629359, 3.000000000000002665, -87.53867513459483973 ) ) ;
#22857 = EDGE_CURVE ( 'NONE', #18615, #14907, #28124, .T. ) ;
#22858 = CARTESIAN_POINT ( 'NONE',  ( -3.175426480542816510, 5.499999999999865885, -97.37499999999998579 ) ) ;
#22859 =( BOUNDED_CURVE ( )  B_SPLINE_CURVE ( 2, ( #22828, #3763, #1769, #15336, #11172, #24656, #1149, #10549, #20062 ),
 .UNSPECIFIED., .F., .T. ) 
 B_SPLINE_CURVE_WITH_KNOTS ( ( 3, 2, 2, 2, 3 ),
 ( 0.6527777777777777901, 0.6537037037037036757, 0.6555555555555555580, 0.6574074074074074403, 0.6583333333333333259 ),
 .UNSPECIFIED. ) 
 CURVE ( )  GEOMETRIC_REPRESENTATION_ITEM ( )  RATIONAL_B_SPLINE_CURVE ( ( 0.9330127018922194093, 0.9330127018922194093, 1.000000000000000000, 0.8660254037844388186, 1.000000000000000000, 0.8660254037844388186, 1.000000000000000000, 0.9330127018922194093, 0.9330127018922194093 ) ) 
 REPRESENTATION_ITEM ( '' )  );
#22860 = CIRCLE ( 'NONE', #21399, 17.50000000000004619 ) ;
#22861 = CARTESIAN_POINT ( 'NONE',  ( 159.6711002691896510, 4.999999999999989342, 2.071067811865468400 ) ) ;
#22862 = CARTESIAN_POINT ( 'NONE',  ( -0.05509383827833347347, -14.57570334281945001, 8.269883983291466123 ) ) ;
#22863 = ORIENTED_EDGE ( 'NONE', *, *, #601, .T. ) ;
#22864 = CARTESIAN_POINT ( 'NONE',  ( 10.93750000000001066, -1.097466725451439196, 2.649519052838178457 ) ) ;
#22865 = CARTESIAN_POINT ( 'NONE',  ( 117.6874999999997726, -1.035533905932719101, -2.499999999999844569 ) ) ;
#22866 = CARTESIAN_POINT ( 'NONE',  ( 110.8127832217621318, -1.849990392679381701, 0.7662911109078888172 ) ) ;
#22867 = CARTESIAN_POINT ( 'NONE',  ( 6.000000000000000888, 7.762456499804234384E-14, -133.5863248654052029 ) ) ;
#22868 = ORIENTED_EDGE ( 'NONE', *, *, #20256, .F. ) ;
#22869 = PRESENTATION_STYLE_ASSIGNMENT (( #25450 ) ) ;
#22870 = VECTOR ( 'NONE', #22172, 1000.000000000000000 ) ;
#22871 = CARTESIAN_POINT ( 'NONE',  ( 5.412658773652712085, -3.125000000000086153, -87.06698729810780435 ) ) ;
#22872 = ORIENTED_EDGE ( 'NONE', *, *, #18669, .T. ) ;
#22873 = CARTESIAN_POINT ( 'NONE',  ( -5.999999999999963585, -1.487416814333745711E-14, -75.83632486540521711 ) ) ;
#22874 = EDGE_LOOP ( 'NONE', ( #17916, #9375, #4872, #9548 ) ) ;
#22875 = CARTESIAN_POINT ( 'NONE',  ( 157.3125000000000284, 4.242640687119298093, -4.242640687119298093 ) ) ;
#22876 = CARTESIAN_POINT ( 'NONE',  ( 0.000000000000000000, 5.499999999999991118, -121.5000000000000568 ) ) ;
#22877 = CARTESIAN_POINT ( 'NONE',  ( 24.31250000000012079, 2.649519052838419153, -1.097466725451559322 ) ) ;
#22878 = CARTESIAN_POINT ( 'NONE',  ( -3.608439182435115633, 6.249999999999965361, -129.3080127018922383 ) ) ;
#22879 = ORIENTED_EDGE ( 'NONE', *, *, #5279, .F. ) ;
#22880 = CARTESIAN_POINT ( 'NONE',  ( 5.196152422706629359, 3.000000000000002665, -57.53867513459481842 ) ) ;
#22881 = CARTESIAN_POINT ( 'NONE',  ( 2.775557561562891351E-14, 6.250000000000033751, -121.0669872981078328 ) ) ;
#22882 = CARTESIAN_POINT ( 'NONE',  ( 5.412658773652739619, 3.124999999999988898, -179.8169872981077901 ) ) ;
#22883 = CARTESIAN_POINT ( 'NONE',  ( 160.9483822453071014, -11.55409466406504748, 3.248948683749017796 ) ) ;
#22884 =( NAMED_UNIT ( * ) SI_UNIT ( $, .STERADIAN. ) SOLID_ANGLE_UNIT ( ) );
#22885 = EDGE_CURVE ( 'NONE', #4758, #6403, #9490, .T. ) ;
#22886 = ORIENTED_EDGE ( 'NONE', *, *, #27680, .T. ) ;
#22887 = CARTESIAN_POINT ( 'NONE',  ( 11.68750000000000000, -0.8284271247461753029, -1.999999999999971800 ) ) ;
#22888 = CARTESIAN_POINT ( 'NONE',  ( 140.0769230769231228, -11.53846153846155254, 4.615384615384604317 ) ) ;
#22889 = AXIS2_PLACEMENT_3D ( 'NONE', #20045, #24328, #20349 ) ;
#22890 = EDGE_CURVE ( 'NONE', #25655, #12427, #15074, .T. ) ;
#22891 = CARTESIAN_POINT ( 'NONE',  ( 159.7995982923682732, -12.30064632830203664, -3.603981859628974771 ) ) ;
#22892 = CARTESIAN_POINT ( 'NONE',  ( 5.196152422706629359, 3.000000000000002665, -133.4613248654052313 ) ) ;
#22893 = FACE_OUTER_BOUND ( 'NONE', #23343, .T. ) ;
#22894 = CARTESIAN_POINT ( 'NONE',  ( -7.216878364870328078, 0.000000000000000000, -77.19198729810784698 ) ) ;
#22895 = CARTESIAN_POINT ( 'NONE',  ( -5.412658773652684552, -3.125000000000099920, -62.06698729810783277 ) ) ;
#22896 = DIRECTION ( 'NONE',  ( 6.938893903907221278E-15, -1.000000000000000000, 0.000000000000000000 ) ) ;
#22897 = CARTESIAN_POINT ( 'NONE',  ( 4.763139720814407951, -2.749999999999988454, -47.00000000000004263 ) ) ;
#22898 = CYLINDRICAL_SURFACE ( 'NONE', #967, 6.000000000000000888 ) ;
#22899 = CARTESIAN_POINT ( 'NONE',  ( 3.175426480543072749, 5.499999999999865885, -121.6250000000000284 ) ) ;
#22900 =( GEOMETRIC_REPRESENTATION_CONTEXT ( 3 ) GLOBAL_UNCERTAINTY_ASSIGNED_CONTEXT ( ( #14288 ) ) GLOBAL_UNIT_ASSIGNED_CONTEXT ( ( #29826, #4483, #16061 ) ) REPRESENTATION_CONTEXT ( 'NONE', 'WORKASPACE' ) );
#22901 = EDGE_LOOP ( 'NONE', ( #17176, #27558, #29069, #15817 ) ) ;
#22902 = CARTESIAN_POINT ( 'NONE',  ( 22.37500000000014566, 1.665334536937734811E-13, -2.649519052838333888 ) ) ;
#22903 = CARTESIAN_POINT ( 'NONE',  ( 5.196152422706629359, 3.000000000000002665, -122.9613248654052313 ) ) ;
#22904 = CYLINDRICAL_SURFACE ( 'NONE', #15320, 0.5000000000000004441 ) ;
#22905 = CARTESIAN_POINT ( 'NONE',  ( 140.4523502691896510, 0.000000000000000000, 5.000000000000004441 ) ) ;
#22906 = EDGE_LOOP ( 'NONE', ( #8388, #4868, #26108, #10136 ) ) ;
#22907 = AXIS2_PLACEMENT_3D ( 'NONE', #17267, #26588, #937 ) ;
#22908 = CARTESIAN_POINT ( 'NONE',  ( 111.6872167782374135, 1.849990392679562001, 0.7662911109079489913 ) ) ;
#22909 = CARTESIAN_POINT ( 'NONE',  ( 118.2738248654049329, -1.999999999999971800, -0.8284271247458748766 ) ) ;
#22910 = CARTESIAN_POINT ( 'NONE',  ( 113.6872167782373850, 1.849990392679532247, 0.7662911109078888172 ) ) ;
#22911 = CARTESIAN_POINT ( 'NONE',  ( -3.608439182435115633, 6.249999999999965361, -114.9419872981078328 ) ) ;
#22912 =( BOUNDED_CURVE ( )  B_SPLINE_CURVE ( 2, ( #24485, #26633, #17015, #12562, #988, #10087, #26344, #5292, #19460 ),
 .UNSPECIFIED., .F., .F. ) 
 B_SPLINE_CURVE_WITH_KNOTS ( ( 3, 2, 2, 2, 3 ),
 ( 0.7058823529411764053, 0.7132352941176470784, 0.7205882352941176405, 0.7279411764705882026, 0.7352941176470588758 ),
 .UNSPECIFIED. ) 
 CURVE ( )  GEOMETRIC_REPRESENTATION_ITEM ( )  RATIONAL_B_SPLINE_CURVE ( ( 1.000000000000000000, 0.9238795325112867385, 1.000000000000000000, 0.9238795325112867385, 1.000000000000000000, 0.9238795325112867385, 1.000000000000000000, 0.9238795325112867385, 1.000000000000000000 ) ) 
 REPRESENTATION_ITEM ( '' )  );
#22913 = CARTESIAN_POINT ( 'NONE',  ( 5.196152422706629359, -2.999999999999988898, -109.7113248654052455 ) ) ;
#22914 = CARTESIAN_POINT ( 'NONE',  ( 10.00000000000014921, -0.4401475947494610241, 2.447530906695864150 ) ) ;
#22915 = ORIENTED_EDGE ( 'NONE', *, *, #20112, .F. ) ;
#22916 = VERTEX_POINT ( 'NONE', #24873 ) ;
#22917 = CARTESIAN_POINT ( 'NONE',  ( 21.52382486540530238, 1.035533905932929599, -2.499999999999964473 ) ) ;
#22918 = CARTESIAN_POINT ( 'NONE',  ( 143.5312500000000284, -2.485281374238555774, -6.000000000000005329 ) ) ;
#22919 = CARTESIAN_POINT ( 'NONE',  ( -3.608439182435052128, -6.250000000000110134, -145.9419872981078470 ) ) ;
#22920 = SURFACE_STYLE_USAGE ( .BOTH. , #973 ) ;
#22921 = DIRECTION ( 'NONE',  ( 1.000000000000000000, 0.000000000000000000, 0.000000000000000000 ) ) ;
#22922 = DIRECTION ( 'NONE',  ( 0.000000000000000000, 0.000000000000000000, 1.000000000000000000 ) ) ;
#22923 = CARTESIAN_POINT ( 'NONE',  ( 24.18750000000015277, 0.8284271247463557142, 2.000000000000031530 ) ) ;
#22924 = CARTESIAN_POINT ( 'NONE',  ( 136.5863248654052313, 0.000000000000000000, 5.500000000000005329 ) ) ;
#22925 = CIRCLE ( 'NONE', #27805, 0.5000000000000004441 ) ;
#22926 = CARTESIAN_POINT ( 'NONE',  ( -5.999999999999963585, 1.780251999655701777E-13, -61.41367513459483973 ) ) ;
#22927 = CARTESIAN_POINT ( 'NONE',  ( -7.216878364870328078, 0.000000000000000000, -70.55801270189220986 ) ) ;
#22928 = EDGE_CURVE ( 'NONE', #21920, #24100, #16869, .T. ) ;
#22929 = CARTESIAN_POINT ( 'NONE',  ( 135.0583403565074150, -7.808325495656168513, -8.343593232213100563 ) ) ;
#22930 = CARTESIAN_POINT ( 'NONE',  ( 145.1101497308104058, 3.535533905932725318, 3.535533905932725318 ) ) ;
#22931 = CARTESIAN_POINT ( 'NONE',  ( -3.464101615137757051, -5.999999999999979572, -178.1636751345948255 ) ) ;
#22932 = DIRECTION ( 'NONE',  ( 1.000000000000000000, -5.551115123125774690E-17, 0.000000000000000000 ) ) ;
#22933 = CARTESIAN_POINT ( 'NONE',  ( -3.464101615137757051, -5.999999999999979572, -155.6636751345947971 ) ) ;
#22934 = CARTESIAN_POINT ( 'NONE',  ( -15.49999999999999289, -24.99999999999999289, 7.500000000000007105 ) ) ;
#22935 = LINE ( 'NONE', #2036, #8662 ) ;
#22936 = CARTESIAN_POINT ( 'NONE',  ( 109.1249999999999289, 1.767766952966265404, 1.767766952966431937 ) ) ;
#22937 = CARTESIAN_POINT ( 'NONE',  ( 3.175426480543072749, -5.500000000000105693, -128.1250000000000000 ) ) ;
#22938 = CYLINDRICAL_SURFACE ( 'NONE', #11756, 6.000000000000000888 ) ;
#22939 = CARTESIAN_POINT ( 'NONE',  ( -3.608439182435115633, 6.249999999999965361, -145.8080127018922383 ) ) ;
#22940 = CARTESIAN_POINT ( 'NONE',  ( -5.999999999999963585, 1.780251999655701777E-13, -65.33632486540521711 ) ) ;
#22941 = ORIENTED_EDGE ( 'NONE', *, *, #8773, .T. ) ;
#22942 = CARTESIAN_POINT ( 'NONE',  ( -3.175426480542816066, 5.499999999999865885, -52.37500000000002842 ) ) ;
#22943 = CARTESIAN_POINT ( 'NONE',  ( 5.999999999999999112, 2.951592740943527306E-14, -153.6636751345948539 ) ) ;
#22944 = DIRECTION ( 'NONE',  ( -1.000000000000000000, 0.000000000000000000, 0.000000000000000000 ) ) ;
#22945 = DIRECTION ( 'NONE',  ( 0.000000000000000000, 0.000000000000000000, 1.000000000000000000 ) ) ;
#22946 = EDGE_LOOP ( 'NONE', ( #3171, #22505, #28952, #30231 ) ) ;
#22947 = CARTESIAN_POINT ( 'NONE',  ( 105.6249999999999005, -1.767766952966376426, -1.767766952966320915 ) ) ;
#22948 = CARTESIAN_POINT ( 'NONE',  ( 147.6562500000000568, -6.000000000000005329, 2.485281374238556218 ) ) ;
#22949 = CARTESIAN_POINT ( 'NONE',  ( 159.9005546240083788, -12.40839718913323431, -3.439547090519799788 ) ) ;
#22950 = CARTESIAN_POINT ( 'NONE',  ( 12.56250000000007638, -1.999999999999851674, -0.8284271247462354770 ) ) ;
#22951 = MECHANICAL_DESIGN_GEOMETRIC_PRESENTATION_REPRESENTATION (  '', ( #27832 ), #24897 ) ;
#22952 =( BOUNDED_SURFACE ( )  B_SPLINE_SURFACE ( 3, 2, ( 
 ( #25805, #12317, #28682 ),
 ( #23520, #28089, #7505 ),
 ( #2602, #11876, #16477 ),
 ( #21212, #17064, #9984 ),
 ( #26393, #19360, #16919 ),
 ( #21358, #28243, #7217 ) ),
 .UNSPECIFIED., .F., .F., .F. ) 
 B_SPLINE_SURFACE_WITH_KNOTS ( ( 4, 2, 4 ),
 ( 3, 3 ),
 ( 0.000000000000000000, 0.001011980645342317126, 0.002023961290684634252 ),
 ( 0.000000000000000000, 1.000000000000000000 ),
 .UNSPECIFIED. ) 
 GEOMETRIC_REPRESENTATION_ITEM ( )  RATIONAL_B_SPLINE_SURFACE ( (
 ( 1.000000000000000000, 0.8593225670956829987, 1.000000000000000000),
 ( 1.000000000000000000, 0.8348814976564934431, 1.000000000000000000),
 ( 1.000000000000000000, 0.8097437468337547184, 1.000000000000000000),
 ( 1.000000000000000000, 0.7587734595484167954, 1.000000000000000000),
 ( 1.000000000000000000, 0.7329355451685689582, 1.000000000000000000),
 ( 1.000000000000000000, 0.7071067811865475727, 1.000000000000000000) ) ) 
 REPRESENTATION_ITEM ( '' )  SURFACE ( )  );
#22953 = CARTESIAN_POINT ( 'NONE',  ( 140.8125000000000284, 4.242640687119298093, -4.242640687119298093 ) ) ;
#22954 = CARTESIAN_POINT ( 'NONE',  ( 119.7499999999998721, 1.110223024625156540E-13, -2.499999999999946709 ) ) ;
#22955 = ORIENTED_EDGE ( 'NONE', *, *, #10762, .F. ) ;
#22956 = ADVANCED_FACE ( 'NONE', ( #3517 ), #5523, .T. ) ;
#22957 = CARTESIAN_POINT ( 'NONE',  ( 4.763139720814407951, 2.750000000000002665, -136.7500000000000284 ) ) ;
#22958 = VERTEX_POINT ( 'NONE', #24725 ) ;
#22959 = CARTESIAN_POINT ( 'NONE',  ( 14.75000000000009592, 2.220446049250313081E-13, -2.000000000000057288 ) ) ;
#22960 = ORIENTED_EDGE ( 'NONE', *, *, #28099, .T. ) ;
#22961 = CARTESIAN_POINT ( 'NONE',  ( -4.763139720814407951, -2.750000000000016431, -68.50000000000000000 ) ) ;
#22962 = CARTESIAN_POINT ( 'NONE',  ( 18.83632486540531659, 1.767766952966431937, 1.767766952966320915 ) ) ;
#22963 = EDGE_CURVE ( 'NONE', #3491, #26834, #24260, .T. ) ;
#22964 = CARTESIAN_POINT ( 'NONE',  ( 2.775557561562891351E-14, -11.00000000000001066, -31.00000000000002842 ) ) ;
#22965 = CARTESIAN_POINT ( 'NONE',  ( 140.1363996827915059, -11.13639968279144732, -4.472640761300552548 ) ) ;
#22966 = DIRECTION ( 'NONE',  ( -1.000000000000000000, -1.665334536937731113E-16, 1.526556658859586792E-16 ) ) ;
#22967 = CARTESIAN_POINT ( 'NONE',  ( 120.5002832217621886, 1.308140751793723799, 1.308140751793751555 ) ) ;
#22968 = VECTOR ( 'NONE', #26303, 1000.000000000000000 ) ;
#22969 = VECTOR ( 'NONE', #5908, 1000.000000000000000 ) ;
#22970 = DIRECTION ( 'NONE',  ( -0.9579811153107213872, 0.2635057997273862473, 0.1132999391794057009 ) ) ;
#22971 = TOROIDAL_SURFACE ( 'NONE', #9732, 11.00000000000000355, 1.000000000000000000 ) ;
#22972 = CARTESIAN_POINT ( 'NONE',  ( 6.350852961086080661, -9.614813431917819062E-14, -145.8750000000000284 ) ) ;
#22973 = CARTESIAN_POINT ( 'NONE',  ( -2.081668171172168020E-16, -5.204170427930420051E-17, 2.499999999999999112 ) ) ;
#22974 = CARTESIAN_POINT ( 'NONE',  ( -5.412658773652739619, 3.124999999999975131, -157.6830127018922099 ) ) ;
#22975 = DIRECTION ( 'NONE',  ( -1.000000000000000000, -3.330669073875465184E-16, 6.770847460736368028E-36 ) ) ;
#22976 = CARTESIAN_POINT ( 'NONE',  ( -4.763139720814407951, 2.749999999999946709, -86.75000000000000000 ) ) ;
#22977 = DIRECTION ( 'NONE',  ( -1.040834085586083310E-14, -1.000000000000000000, 0.000000000000000000 ) ) ;
#22978 = CARTESIAN_POINT ( 'NONE',  ( 4.763139720814407951, 2.750000000000002665, -73.75000000000004263 ) ) ;
#22979 = FACE_OUTER_BOUND ( 'NONE', #2783, .T. ) ;
#22980 = CARTESIAN_POINT ( 'NONE',  ( 148.9836002691896795, 4.999999999999989342, -2.071067811865468400 ) ) ;
#22981 = CARTESIAN_POINT ( 'NONE',  ( 6.000000000000000888, -3.330669073875464691E-16, -7.560779664488942560E-35 ) ) ;
#22982 = CARTESIAN_POINT ( 'NONE',  ( 0.000000000000000000, 0.000000000000000000, 0.000000000000000000 ) ) ;
#22983 = CARTESIAN_POINT ( 'NONE',  ( 21.25000000000015632, 0.000000000000000000, 2.000000000000057288 ) ) ;
#22984 = CARTESIAN_POINT ( 'NONE',  ( -5.196152422706601826, 2.999999999999975131, -118.5386751345948113 ) ) ;
#22985 = CARTESIAN_POINT ( 'NONE',  ( -5.999999999999963585, 8.134310703387671600E-14, -146.3363248654052313 ) ) ;
#22986 = CARTESIAN_POINT ( 'NONE',  ( 117.0622167782374561, -1.849990392679472073, 0.7662911109078888172 ) ) ;
#22987 = DIRECTION ( 'NONE',  ( -1.000000000000000000, 0.000000000000000000, 0.000000000000000000 ) ) ;
#22988 = VERTEX_POINT ( 'NONE', #5666 ) ;
#22989 = CARTESIAN_POINT ( 'NONE',  ( 153.4687500000000853, -2.485281374238585972, 6.000000000000005329 ) ) ;
#22990 = CARTESIAN_POINT ( 'NONE',  ( -0.5000000000000004441, -10.00000000000000888, -5.000000000000004441 ) ) ;
#22991 = EDGE_CURVE ( 'NONE', #21072, #23786, #13457, .T. ) ;
#22992 = CARTESIAN_POINT ( 'NONE',  ( 0.000000000000000000, -5.999999999999991118, -85.03867513459483973 ) ) ;
#22993 = ORIENTED_EDGE ( 'NONE', *, *, #30161, .T. ) ;
#22994 = ORIENTED_EDGE ( 'NONE', *, *, #1648, .F. ) ;
#22995 = ORIENTED_EDGE ( 'NONE', *, *, #10478, .F. ) ;
#22996 = CARTESIAN_POINT ( 'NONE',  ( -4.763139720814407951, 2.749999999999946709, -98.75000000000000000 ) ) ;
#22997 = EDGE_CURVE ( 'NONE', #6403, #25123, #8483, .T. ) ;
#22998 = CARTESIAN_POINT ( 'NONE',  ( -3.608439182435052128, -6.250000000000110134, -110.8080127018922099 ) ) ;
#22999 = ADVANCED_FACE ( 'NONE', ( #13101 ), #11675, .T. ) ;
#23000 = DIRECTION ( 'NONE',  ( -7.147005652999508048E-36, 5.642372883946980038E-36, 1.000000000000000000 ) ) ;
#23001 = DIRECTION ( 'NONE',  ( -7.147005652999508048E-36, 5.642372883946980038E-36, 1.000000000000000000 ) ) ;
#23002 = B_SPLINE_CURVE_WITH_KNOTS ( 'NONE', 3,
 ( #20771, #8307, #25190, #24752, #13274, #15891, #29655, #4000, #13419, #27040, #1858, #27347 ),
 .UNSPECIFIED., .F., .F.,
 ( 4, 2, 2, 2, 2, 4 ),
 ( 0.000000000000000000, 0.0002134524463634672269, 0.0004269048927269344538, 0.0008538097854538677150, 0.001280714678180800868, 0.001707619570907734346 ),
 .UNSPECIFIED. ) ;
#23003 = CARTESIAN_POINT ( 'NONE',  ( -5.999999999999956479, -1.607695154586745057, -106.3466878364870354 ) ) ;
#23004 = ORIENTED_EDGE ( 'NONE', *, *, #21290, .T. ) ;
#23005 = FACE_OUTER_BOUND ( 'NONE', #19954, .T. ) ;
#23006 =( NAMED_UNIT ( * ) SI_UNIT ( $, .STERADIAN. ) SOLID_ANGLE_UNIT ( ) );
#23007 = CARTESIAN_POINT ( 'NONE',  ( 0.000000000000000000, 5.499999999999991118, -171.0000000000000284 ) ) ;
#23008 = CARTESIAN_POINT ( 'NONE',  ( 139.6491219074057710, -8.798545334315207356, 8.159999999999998366 ) ) ;
#23009 = CARTESIAN_POINT ( 'NONE',  ( -3.175426480542816510, 5.499999999999865885, -160.3750000000000000 ) ) ;
#23010 = CARTESIAN_POINT ( 'NONE',  ( 114.8124999999998010, 1.035533905932749299, -2.499999999999844569 ) ) ;
#23011 = CARTESIAN_POINT ( 'NONE',  ( 0.000000000000000000, 5.499999999999991118, -109.5000000000000426 ) ) ;
#23012 = PRESENTATION_STYLE_ASSIGNMENT (( #23478 ) ) ;
#23013 = CARTESIAN_POINT ( 'NONE',  ( 6.000000000000000888, -3.330669073875464691E-16, -7.560779664488942560E-35 ) ) ;
#23014 = CARTESIAN_POINT ( 'NONE',  ( 6.350852961086080661, -9.614813431917819062E-14, -97.87499999999998579 ) ) ;
#23015 = CARTESIAN_POINT ( 'NONE',  ( 0.2066684337268677174, -15.46624955645880561, 8.188921300829465011 ) ) ;
#23016 = ORIENTED_EDGE ( 'NONE', *, *, #13974, .T. ) ;
#23017 = CARTESIAN_POINT ( 'NONE',  ( 10.62500000000016165, 2.649519052838555933, 1.110223024625156540E-13 ) ) ;
#23018 = CARTESIAN_POINT ( 'NONE',  ( 117.9999999999997868, 2.500000000000002220, 2.220446049250313081E-13 ) ) ;
#23019 = CARTESIAN_POINT ( 'NONE',  ( 12.52382486540527751, 1.035533905932809473, -2.499999999999904521 ) ) ;
#23020 = CARTESIAN_POINT ( 'NONE',  ( 112.2502832217622739, 1.308140751793640533, -1.308140751793640533 ) ) ;
#23021 = CARTESIAN_POINT ( 'NONE',  ( 157.6949251345948539, 5.500000000000012434, -2.278174593052012309 ) ) ;
#23022 = ORIENTED_EDGE ( 'NONE', *, *, #12364, .T. ) ;
#23023 = CARTESIAN_POINT ( 'NONE',  ( 107.8122167782374135, 0.7662911109078888172, 1.849990392679712103 ) ) ;
#23024 = CARTESIAN_POINT ( 'NONE',  ( -3.608439182435052128, -6.250000000000110134, -87.44198729810781856 ) ) ;
#23025 = EDGE_CURVE ( 'NONE', #12881, #12934, #3686, .T. ) ;
#23026 = CARTESIAN_POINT ( 'NONE',  ( 110.9613248654051176, -5.551115123125782702E-14, 2.000000000000112799 ) ) ;
#23027 = ORIENTED_EDGE ( 'NONE', *, *, #25722, .F. ) ;
#23028 = CARTESIAN_POINT ( 'NONE',  ( 107.0238248654051176, -0.8284271247461153509, 2.000000000000212275 ) ) ;
#23029 = ORIENTED_EDGE ( 'NONE', *, *, #21101, .T. ) ;
#23030 = ORIENTED_EDGE ( 'NONE', *, *, #6659, .F. ) ;
#23031 = CARTESIAN_POINT ( 'NONE',  ( 148.5000000000000284, 6.000000000000005329, 0.000000000000000000 ) ) ;
#23032 = ORIENTED_EDGE ( 'NONE', *, *, #22857, .T. ) ;
#23033 = CARTESIAN_POINT ( 'NONE',  ( -3.175426480542816510, 5.499999999999865885, -121.3750000000000284 ) ) ;
#23034 = CARTESIAN_POINT ( 'NONE',  ( 22.93750000000013856, -2.649519052838178457, -1.097466725451559322 ) ) ;
#23035 = ADVANCED_FACE ( 'NONE', ( #1833 ), #23049, .T. ) ;
#23036 =( BOUNDED_CURVE ( )  B_SPLINE_CURVE ( 2, ( #7733, #14409, #16994, #17141, #14681, #14258, #7437, #5421, #21437 ),
 .UNSPECIFIED., .F., .T. ) 
 B_SPLINE_CURVE_WITH_KNOTS ( ( 3, 2, 2, 2, 3 ),
 ( 0.2638888888888889506, 0.2648148148148148362, 0.2666666666666667185, 0.2685185185185184897, 0.2694444444444443754 ),
 .UNSPECIFIED. ) 
 CURVE ( )  GEOMETRIC_REPRESENTATION_ITEM ( )  RATIONAL_B_SPLINE_CURVE ( ( 0.9330127018922194093, 0.9330127018922234061, 1.000000000000000000, 0.8660254037844388186, 1.000000000000000000, 0.8660254037844388186, 1.000000000000000000, 0.9330127018922234061, 0.9330127018922194093 ) ) 
 REPRESENTATION_ITEM ( '' )  );
#23037 = CARTESIAN_POINT ( 'NONE',  ( 5.412658773652712085, -3.125000000000086153, -128.4330127018922099 ) ) ;
#23038 = ORIENTED_EDGE ( 'NONE', *, *, #24396, .F. ) ;
#23039 = AXIS2_PLACEMENT_3D ( 'NONE', #3367, #12345, #3215 ) ;
#23040 = CARTESIAN_POINT ( 'NONE',  ( -5.412658773652739619, 3.124999999999975131, -165.8169872981077901 ) ) ;
#23041 = CARTESIAN_POINT ( 'NONE',  ( 5.412658773652739619, 3.124999999999988898, -173.8169872981077901 ) ) ;
#23042 =( NAMED_UNIT ( * ) PLANE_ANGLE_UNIT ( ) SI_UNIT ( $, .RADIAN. ) );
#23043 = CARTESIAN_POINT ( 'NONE',  ( -5.999999999999944933, 1.607695154586759934, -146.9806624327026157 ) ) ;
#23044 = ORIENTED_EDGE ( 'NONE', *, *, #6430, .T. ) ;
#23045 = CARTESIAN_POINT ( 'NONE',  ( 0.7669223171414829565, -15.58766199952930620, -7.954545454545462135 ) ) ;
#23046 = CARTESIAN_POINT ( 'NONE',  ( 110.9761751345946266, -0.8284271247460852639, -1.999999999999791278 ) ) ;
#23047 =( BOUNDED_CURVE ( )  B_SPLINE_CURVE ( 2, ( #30045, #17958, #6547, #15663, #11190, #1634, #3923, #29887, #18407 ),
 .UNSPECIFIED., .F., .T. ) 
 B_SPLINE_CURVE_WITH_KNOTS ( ( 3, 2, 2, 2, 3 ),
 ( 0.2805555555555555580, 0.2814814814814814992, 0.2833333333333333259, 0.2851851851851852082, 0.2861111111111111494 ),
 .UNSPECIFIED. ) 
 CURVE ( )  GEOMETRIC_REPRESENTATION_ITEM ( )  RATIONAL_B_SPLINE_CURVE ( ( 0.9330127018922194093, 0.9330127018922194093, 1.000000000000000000, 0.8660254037844388186, 1.000000000000000000, 0.8660254037844388186, 1.000000000000000000, 0.9330127018922174109, 0.9330127018922194093 ) ) 
 REPRESENTATION_ITEM ( '' )  );
#23048 = CARTESIAN_POINT ( 'NONE',  ( -6.000000000000023093, 1.607695154586625819, -132.9033121635129930 ) ) ;
#23049 = CYLINDRICAL_SURFACE ( 'NONE', #13429, 0.5000000000000004441 ) ;
#23050 = CARTESIAN_POINT ( 'NONE',  ( 110.3127832217620323, 1.849990392679501827, -0.7662911109075883909 ) ) ;
#23051 = CARTESIAN_POINT ( 'NONE',  ( 5.412658773652739619, 3.124999999999988898, -76.31698729810781856 ) ) ;
#23052 = CARTESIAN_POINT ( 'NONE',  ( 2.775557561562891351E-14, -6.250000000000061284, -58.81698729810780435 ) ) ;
#23053 = CARTESIAN_POINT ( 'NONE',  ( 3.175426480543072749, 5.499999999999865885, -52.62500000000002842 ) ) ;
#23054 = FACE_OUTER_BOUND ( 'NONE', #4843, .T. ) ;
#23055 = CARTESIAN_POINT ( 'NONE',  ( 6.000000000000000888, -1.859271017917181981E-14, -47.16367513459483263 ) ) ;
#23056 = CARTESIAN_POINT ( 'NONE',  ( 10.41367513459478999, 1.767766952966376426, 1.767766952966376426 ) ) ;
#23057 = CARTESIAN_POINT ( 'NONE',  ( -3.175426480542816510, 5.499999999999865885, -118.3750000000000142 ) ) ;
#23058 = CARTESIAN_POINT ( 'NONE',  ( 3.175426480543072749, 5.499999999999865885, -156.1250000000000000 ) ) ;
#23059 = DIRECTION ( 'NONE',  ( -1.000000000000000000, -1.067522139062651904E-16, 0.000000000000000000 ) ) ;
#23060 = ORIENTED_EDGE ( 'NONE', *, *, #26796, .F. ) ;
#23061 = CARTESIAN_POINT ( 'NONE',  ( 19.75000000000012790, 1.873492889145123019, 1.873492889144845464 ) ) ;
#23062 = CIRCLE ( 'NONE', #4897, 6.499999999999977796 ) ;
#23063 = LINE ( 'NONE', #7066, #13631 ) ;
#23064 = DIRECTION ( 'NONE',  ( 0.000000000000000000, 0.000000000000000000, -1.000000000000000000 ) ) ;
#23065 = CARTESIAN_POINT ( 'NONE',  ( 136.5148502691896510, -3.535533905932725318, -3.535533905932725318 ) ) ;
#23066 = PRESENTATION_LAYER_ASSIGNMENT (  '', '', ( #17673 ) ) ;
#23067 = ORIENTED_EDGE ( 'NONE', *, *, #10270, .T. ) ;
#23068 = CARTESIAN_POINT ( 'NONE',  ( 108.2497167782376266, -1.308140751793585022, -1.308140751793640533 ) ) ;
#23069 = CARTESIAN_POINT ( 'NONE',  ( 151.1175748654052313, 5.500000000000012434, -2.278174593052012309 ) ) ;
#23070 = CARTESIAN_POINT ( 'NONE',  ( 112.4372167782373708, 0.7662911109079189043, -1.849990392679231599 ) ) ;
#23071 = CARTESIAN_POINT ( 'NONE',  ( 7.216878364870455975, -6.409875621278545621E-14, -116.9419872981078328 ) ) ;
#23072 = EDGE_CURVE ( 'NONE', #28223, #4728, #17940, .T. ) ;
#23073 = CARTESIAN_POINT ( 'NONE',  ( 17.14882486540524553, -2.499999999999904521, 1.035533905932749299 ) ) ;
#23074 = EDGE_CURVE ( 'NONE', #23261, #7272, #11237, .T. ) ;
#23075 = DIRECTION ( 'NONE',  ( -7.147005652999508048E-36, 5.642372883946980038E-36, 1.000000000000000000 ) ) ;
#23076 = ORIENTED_EDGE ( 'NONE', *, *, #24941, .T. ) ;
#23077 = ORIENTED_EDGE ( 'NONE', *, *, #20343, .F. ) ;
#23078 = CARTESIAN_POINT ( 'NONE',  ( 138.5699251345948255, 2.278174593052352925, 5.499999999999671374 ) ) ;
#23079 = CARTESIAN_POINT ( 'NONE',  ( 137.7187500000000284, 2.485281374238555774, -6.000000000000005329 ) ) ;
#23080 = CARTESIAN_POINT ( 'NONE',  ( 7.216878364870455975, -6.409875621278545621E-14, -151.4419872981078186 ) ) ;
#23081 = FACE_OUTER_BOUND ( 'NONE', #1238, .T. ) ;
#23082 = CARTESIAN_POINT ( 'NONE',  ( 0.000000000000000000, -5.999999999999991118, -93.46132486540520290 ) ) ;
#23083 = PRESENTATION_LAYER_ASSIGNMENT (  '', '', ( #27467 ) ) ;
#23084 = CARTESIAN_POINT ( 'NONE',  ( 23.25000000000004974, 5.551115123125782702E-14, 1.999999999999946265 ) ) ;
#23085 = DIRECTION ( 'NONE',  ( 0.000000000000000000, 0.000000000000000000, -1.000000000000000000 ) ) ;
#23086 = CARTESIAN_POINT ( 'NONE',  ( -5.999999999999963585, -1.487416814333745711E-14, -137.9136751345947971 ) ) ;
#23087 = CARTESIAN_POINT ( 'NONE',  ( 5.412658773652739619, 3.124999999999988898, -65.18301270189225249 ) ) ;
#23088 = CARTESIAN_POINT ( 'NONE',  ( 135.2991173618539165, -8.337648098108042305, -8.244751738008236686 ) ) ;
#23089 = CARTESIAN_POINT ( 'NONE',  ( 145.0163997308104058, 4.999999999999989342, 2.071067811865468400 ) ) ;
#23090 = CARTESIAN_POINT ( 'NONE',  ( -5.999999999999971578, 1.607695154586715303, -101.9806624327026441 ) ) ;
#23091 = CARTESIAN_POINT ( 'NONE',  ( 6.000000000000000888, -1.859271017917181981E-14, -89.16367513459483973 ) ) ;
#23092 = CARTESIAN_POINT ( 'NONE',  ( 144.0863248654052313, 0.000000000000000000, 5.500000000000005329 ) ) ;
#23093 = CARTESIAN_POINT ( 'NONE',  ( 3.464101615137852974, 5.999999999999884537, -115.3363248654052029 ) ) ;
#23094 = CARTESIAN_POINT ( 'NONE',  ( 109.6249999999999858, -1.767766952966376426, -1.767766952966320915 ) ) ;
#23095 = LINE ( 'NONE', #23401, #41 ) ;
#23096 = CARTESIAN_POINT ( 'NONE',  ( -3.175426480542816066, -5.500000000000057732, -120.8750000000000284 ) ) ;
#23097 = CARTESIAN_POINT ( 'NONE',  ( 5.412658773652712085, -3.125000000000086153, -143.4330127018922383 ) ) ;
#23098 = CARTESIAN_POINT ( 'NONE',  ( 5.196152422706629359, 3.000000000000002665, -113.0386751345948682 ) ) ;
#23099 = CARTESIAN_POINT ( 'NONE',  ( 116.0000000000000142, 0.000000000000000000, 0.000000000000000000 ) ) ;
#23100 = ORIENTED_EDGE ( 'NONE', *, *, #26482, .F. ) ;
#23101 = CARTESIAN_POINT ( 'NONE',  ( -6.350852961085760029, -1.281975124255709124E-13, -53.62500000000002842 ) ) ;
#23102 = CARTESIAN_POINT ( 'NONE',  ( 162.0000000000000284, 0.000000000000000000, 0.000000000000000000 ) ) ;
#23103 = CARTESIAN_POINT ( 'NONE',  ( 17.53867513459494987, 1.665334536937734811E-13, 2.499999999999946709 ) ) ;
#23104 = CARTESIAN_POINT ( 'NONE',  ( -5.999999999999963585, 0.000000000000000000, -179.3363248654052313 ) ) ;
#23105 = EDGE_LOOP ( 'NONE', ( #13118, #17434 ) ) ;
#23106 = CARTESIAN_POINT ( 'NONE',  ( 104.4999999999998863, -2.499999999999919176, 0.000000000000000000 ) ) ;
#23107 = CARTESIAN_POINT ( 'NONE',  ( 140.8125000000000284, 4.242640687119298093, -4.242640687119298093 ) ) ;
#23108 = STYLED_ITEM ( 'NONE', ( #20579 ), #27917 ) ;
#23109 = CARTESIAN_POINT ( 'NONE',  ( 0.000000000000000000, 0.000000000000000000, 0.000000000000000000 ) ) ;
#23110 = ADVANCED_FACE ( 'NONE', ( #22893 ), #27923, .F. ) ;
#23111 = CARTESIAN_POINT ( 'NONE',  ( 139.8750000000000284, 0.000000000000000000, 6.000000000000005329 ) ) ;
#23112 = DIRECTION ( 'NONE',  ( 5.551115123125785167E-17, -1.000000000000000000, -8.881784197001256268E-16 ) ) ;
#23113 = CARTESIAN_POINT ( 'NONE',  ( -6.350852961085760029, -1.281975124255709124E-13, -137.6250000000000568 ) ) ;
#23114 = TOROIDAL_SURFACE ( 'NONE', #26514, 16.50000000000000355, 1.000000000000000000 ) ;
#23115 = ORIENTED_EDGE ( 'NONE', *, *, #5088, .T. ) ;
#23116 = CARTESIAN_POINT ( 'NONE',  ( 14.00000000000006750, 2.000000000000112799, 0.000000000000000000 ) ) ;
#23117 = VERTEX_POINT ( 'NONE', #13708 ) ;
#23118 = CARTESIAN_POINT ( 'NONE',  ( -3.175426480542816510, 5.499999999999865885, -67.37500000000002842 ) ) ;
#23119 = CARTESIAN_POINT ( 'NONE',  ( -3.464101615137757051, -5.999999999999979572, -164.6636751345947687 ) ) ;
#23120 = CARTESIAN_POINT ( 'NONE',  ( 155.1636751345948255, 0.000000000000000000, 5.500000000000005329 ) ) ;
#23121 = CYLINDRICAL_SURFACE ( 'NONE', #28937, 6.000000000000000888 ) ;
#23122 = DIRECTION ( 'NONE',  ( 1.000000000000000000, 0.000000000000000000, -0.000000000000000000 ) ) ;
#23123 = AXIS2_PLACEMENT_3D ( 'NONE', #15907, #22475, #12982 ) ;
#23124 = CARTESIAN_POINT ( 'NONE',  ( 136.0000000000000284, -9.165151389911669000, 8.500000000000007105 ) ) ;
#23125 = CARTESIAN_POINT ( 'NONE',  ( 117.8752832217622881, -1.849990392679551343, 0.000000000000000000 ) ) ;
#23126 = CARTESIAN_POINT ( 'NONE',  ( 175.7502279533881619, 169.4434689287003266, 137.3135186622286597 ) ) ;
#23127 = CARTESIAN_POINT ( 'NONE',  ( 6.350852961086080661, -9.614813431917819062E-14, -147.3750000000000284 ) ) ;
#23128 = CARTESIAN_POINT ( 'NONE',  ( 19.28867513459494987, 2.500000000000057732, -5.551115123125782702E-14 ) ) ;
#23129 = CARTESIAN_POINT ( 'NONE',  ( 4.763139720814407951, -2.749999999999988454, -141.5000000000000284 ) ) ;
#23130 = COLOUR_RGB ( '', 0.66274510, 0.83137255, 0.94901961) ;
#23131 = CARTESIAN_POINT ( 'NONE',  ( 5.412658773652712085, -3.125000000000086153, -158.4330127018922383 ) ) ;
#23132 = CARTESIAN_POINT ( 'NONE',  ( 155.1488248654052029, -3.889087296526011706, -3.889087296526011706 ) ) ;
#23133 = EDGE_CURVE ( 'NONE', #26392, #25470, #17339, .T. ) ;
#23134 = CARTESIAN_POINT ( 'NONE',  ( -3.175426480542816066, -5.500000000000057732, -78.87500000000002842 ) ) ;
#23135 = FACE_OUTER_BOUND ( 'NONE', #22901, .T. ) ;
#23136 = CARTESIAN_POINT ( 'NONE',  ( -6.350852961085760029, -1.281975124255709124E-13, -70.12500000000005684 ) ) ;
#23137 =( BOUNDED_CURVE ( )  B_SPLINE_CURVE ( 2, ( #4486, #5896, #25365, #26935, #8805, #11448, #10390, #10540, #11283 ),
 .UNSPECIFIED., .F., .T. ) 
 B_SPLINE_CURVE_WITH_KNOTS ( ( 3, 2, 2, 2, 3 ),
 ( 0.6583333333333333259, 0.6592592592592592116, 0.6611111111111110938, 0.6629629629629629761, 0.6638888888888889728 ),
 .UNSPECIFIED. ) 
 CURVE ( )  GEOMETRIC_REPRESENTATION_ITEM ( )  RATIONAL_B_SPLINE_CURVE ( ( 0.9330127018922194093, 0.9330127018922194093, 1.000000000000000000, 0.8660254037844388186, 1.000000000000000000, 0.8660254037844388186, 1.000000000000000000, 0.9330127018922154125, 0.9330127018922194093 ) ) 
 REPRESENTATION_ITEM ( '' )  );
#23138 = CARTESIAN_POINT ( 'NONE',  ( 160.7738248654052029, -3.889087296526011706, 3.889087296526011706 ) ) ;
#23139 = CARTESIAN_POINT ( 'NONE',  ( 138.6636751345948255, 0.000000000000000000, 5.500000000000005329 ) ) ;
#23140 = MECHANICAL_DESIGN_GEOMETRIC_PRESENTATION_REPRESENTATION (  '', ( #15297 ), #13848 ) ;
#23141 = CARTESIAN_POINT ( 'NONE',  ( 157.1250000000000284, 0.000000000000000000, -6.000000000000005329 ) ) ;
#23142 = CARTESIAN_POINT ( 'NONE',  ( -27.00000000000002487, 0.000000000000000000, 0.000000000000000000 ) ) ;
#23143 = CARTESIAN_POINT ( 'NONE',  ( 20.68750000000011369, -0.8284271247459952248, -1.999999999999971800 ) ) ;
#23144 = CARTESIAN_POINT ( 'NONE',  ( 2.081668171172167281E-16, 3.582034040661430693E-16, -2.499999999999999112 ) ) ;
#23145 = CARTESIAN_POINT ( 'NONE',  ( 119.3747167782375413, -5.551115123125782702E-14, -1.849990392679523588 ) ) ;
#23146 = FILL_AREA_STYLE ('',( #4374 ) ) ;
#23147 = EDGE_CURVE ( 'NONE', #3410, #4566, #24973, .T. ) ;
#23148 = VERTEX_POINT ( 'NONE', #4591 ) ;
#23149 = CARTESIAN_POINT ( 'NONE',  ( 158.0625000000000284, -4.242640687119298093, 4.242640687119298093 ) ) ;
#23150 = CARTESIAN_POINT ( 'NONE',  ( -5.196152422706573404, -3.000000000000002665, -109.2886751345948397 ) ) ;
#23151 = CARTESIAN_POINT ( 'NONE',  ( 115.1252832217622881, -2.220446049250313081E-13, -1.849990392679523588 ) ) ;
#23152 = CIRCLE ( 'NONE', #9897, 14.49999999999999822 ) ;
#23153 = CARTESIAN_POINT ( 'NONE',  ( -5.196152422706573404, -3.000000000000002665, -85.28867513459481131 ) ) ;
#23154 = ORIENTED_EDGE ( 'NONE', *, *, #9843, .F. ) ;
#23155 = ORIENTED_EDGE ( 'NONE', *, *, #24746, .T. ) ;
#23156 = CIRCLE ( 'NONE', #3484, 1.000000000000000000 ) ;
#23157 = ORIENTED_EDGE ( 'NONE', *, *, #10974, .F. ) ;
#23158 = CARTESIAN_POINT ( 'NONE',  ( 0.000000000000000000, 5.499999999999991118, -90.00000000000002842 ) ) ;
#23159 = CARTESIAN_POINT ( 'NONE',  ( 7.216878364870455975, -6.409875621278545621E-14, -110.3080127018922099 ) ) ;
#23160 = CARTESIAN_POINT ( 'NONE',  ( -0.4142135623730956451, -9.292893218813460976, -4.000000000000004441 ) ) ;
#23161 = LINE ( 'NONE', #16122, #8114 ) ;
#23162 = AXIS2_PLACEMENT_3D ( 'NONE', #10350, #17281, #1106 ) ;
#23163 = CARTESIAN_POINT ( 'NONE',  ( 5.197562551122876684, -9.697615191485738251, -28.02238803416290480 ) ) ;
#23164 = EDGE_LOOP ( 'NONE', ( #22349, #14043, #19370, #5652, #26904 ) ) ;
#23165 = FACE_OUTER_BOUND ( 'NONE', #11343, .T. ) ;
#23166 = CARTESIAN_POINT ( 'NONE',  ( 4.763139720814407951, 2.750000000000002665, -172.7500000000000284 ) ) ;
#23167 = CARTESIAN_POINT ( 'NONE',  ( -0.5000000000000004441, -10.50000000000000888, 7.500000000000007105 ) ) ;
#23168 = CARTESIAN_POINT ( 'NONE',  ( -6.350852961085760029, -1.281975124255709124E-13, -166.1249999999999716 ) ) ;
#23169 = CARTESIAN_POINT ( 'NONE',  ( 112.5624999999998010, -2.499999999999994671, -1.035533905932689347 ) ) ;
#23170 = EDGE_CURVE ( 'NONE', #29809, #1806, #23360, .T. ) ;
#23171 = AXIS2_PLACEMENT_3D ( 'NONE', #24600, #3550, #27205 ) ;
#23172 = CARTESIAN_POINT ( 'NONE',  ( -4.763139720814407951, 2.749999999999946709, -100.2500000000000000 ) ) ;
#23173 = CARTESIAN_POINT ( 'NONE',  ( 0.000000000000000000, -5.999999999999991118, -159.4613248654052029 ) ) ;
#23174 = PLANE ( 'NONE',  #5917 ) ;
#23175 = CARTESIAN_POINT ( 'NONE',  ( 3.175426480543072749, 5.499999999999865885, -97.62500000000004263 ) ) ;
#23176 = CARTESIAN_POINT ( 'NONE',  ( 0.1950436299885377478, -15.42103240523036334, 8.274747089234001152 ) ) ;
#23177 = ORIENTED_EDGE ( 'NONE', *, *, #16372, .F. ) ;
#23178 = CARTESIAN_POINT ( 'NONE',  ( 11.31250000000009592, -1.097466725451379244, -2.649519052838478661 ) ) ;
#23179 = CARTESIAN_POINT ( 'NONE',  ( 118.4374999999998863, -2.499999999999964473, 1.035533905932929599 ) ) ;
#23180 = CARTESIAN_POINT ( 'NONE',  ( 15.66367513459493388, -1.767766952966154381, 1.767766952966376426 ) ) ;
#23181 = CARTESIAN_POINT ( 'NONE',  ( 106.3752832217622171, 1.849990392679523588, 0.000000000000000000 ) ) ;
#23182 = EDGE_CURVE ( 'NONE', #6843, #5319, #29533, .T. ) ;
#23183 = DIRECTION ( 'NONE',  ( 0.000000000000000000, 1.000000000000000000, 0.000000000000000000 ) ) ;
#23184 = ORIENTED_EDGE ( 'NONE', *, *, #11549, .T. ) ;
#23185 = CARTESIAN_POINT ( 'NONE',  ( 109.8363248654051603, 1.414213562373090038, 1.414213562373034527 ) ) ;
#23186 = CARTESIAN_POINT ( 'NONE',  ( 107.1872167782375840, -1.849990392679441875, -0.7662911109076485650 ) ) ;
#23187 =( BOUNDED_CURVE ( )  B_SPLINE_CURVE ( 2, ( #10078, #19450, #5432, #7895, #5886, #15145, #24476, #17308, #2840 ),
 .UNSPECIFIED., .F., .F. ) 
 B_SPLINE_CURVE_WITH_KNOTS ( ( 3, 2, 2, 2, 3 ),
 ( 0.6027777777777777457, 0.6037037037037036313, 0.6055555555555556246, 0.6074074074074073959, 0.6083333333333333925 ),
 .UNSPECIFIED. ) 
 CURVE ( )  GEOMETRIC_REPRESENTATION_ITEM ( )  RATIONAL_B_SPLINE_CURVE ( ( 0.9330127018922194093, 0.9330127018922194093, 1.000000000000000000, 0.8660254037844388186, 1.000000000000000000, 0.8660254037844388186, 1.000000000000000000, 0.9330127018922154125, 0.9330127018922194093 ) ) 
 REPRESENTATION_ITEM ( '' )  );
#23188 = ORIENTED_EDGE ( 'NONE', *, *, #7096, .T. ) ;
#23189 = DIRECTION ( 'NONE',  ( 0.3589790793088772358, -0.3589790793088664111, -0.8615497903412833169 ) ) ;
#23190 = CARTESIAN_POINT ( 'NONE',  ( 151.1250000000000284, 0.000000000000000000, -6.000000000000005329 ) ) ;
#23191 = ORIENTED_EDGE ( 'NONE', *, *, #1289, .F. ) ;
#23192 = CARTESIAN_POINT ( 'NONE',  ( -6.350852961085760029, -1.281975124255709124E-13, -113.6249999999999858 ) ) ;
#23193 = CARTESIAN_POINT ( 'NONE',  ( 21.56250000000010303, 1.097466725451739622, 2.649519052838358757 ) ) ;
#23194 = CARTESIAN_POINT ( 'NONE',  ( 5.412658773652739619, 3.124999999999988898, -131.1830127018922667 ) ) ;
#23195 = ORIENTED_EDGE ( 'NONE', *, *, #6322, .F. ) ;
#23196 = CARTESIAN_POINT ( 'NONE',  ( 3.608439182435180470, -6.249999999999997335, -166.6919872981078186 ) ) ;
#23197 = CARTESIAN_POINT ( 'NONE',  ( 5.412658773652712085, -3.125000000000086153, -175.5669872981078186 ) ) ;
#23198 = CARTESIAN_POINT ( 'NONE',  ( 161.0000000000000284, -11.67610212985248275, 2.769230769230770939 ) ) ;
#23199 =( NAMED_UNIT ( * ) PLANE_ANGLE_UNIT ( ) SI_UNIT ( $, .RADIAN. ) );
#23200 = ORIENTED_EDGE ( 'NONE', *, *, #14847, .T. ) ;
#23201 = CARTESIAN_POINT ( 'NONE',  ( 11.00000000000014921, 2.000000000000112799, 0.000000000000000000 ) ) ;
#23202 = CARTESIAN_POINT ( 'NONE',  ( 110.9136751345947260, -1.414213562373090038, -1.414213562373145550 ) ) ;
#23203 = CARTESIAN_POINT ( 'NONE',  ( 152.9136751345948539, 0.000000000000000000, -5.500000000000005329 ) ) ;
#23204 = CYLINDRICAL_SURFACE ( 'NONE', #15307, 2.000000000000012879 ) ;
#23205 = CARTESIAN_POINT ( 'NONE',  ( -3.464101615137757051, -5.999999999999979572, -150.5863248654051461 ) ) ;
#23206 = CARTESIAN_POINT ( 'NONE',  ( 112.3752832217621176, 1.849990392679551343, 0.000000000000000000 ) ) ;
#23207 = CARTESIAN_POINT ( 'NONE',  ( 2.775557561562891351E-14, 6.250000000000033751, -74.56698729810784698 ) ) ;
#23208 = CARTESIAN_POINT ( 'NONE',  ( 3.608439182435180470, 6.249999999999982236, -59.69198729810782567 ) ) ;
#23209 = CARTESIAN_POINT ( 'NONE',  ( -3.175426480542816510, -5.500000000000057732, -53.37500000000002842 ) ) ;
#23210 = CARTESIAN_POINT ( 'NONE',  ( -0.1262135825162392921, -9.436893208741910399, -4.496381089953947807 ) ) ;
#23211 = EDGE_CURVE ( 'NONE', #24771, #14641, #19503, .T. ) ;
#23212 = DIRECTION ( 'NONE',  ( -0.000000000000000000, -1.000000000000000000, -0.000000000000000000 ) ) ;
#23213 = CARTESIAN_POINT ( 'NONE',  ( -5.196152422706601826, 2.999999999999975131, -159.0386751345948539 ) ) ;
#23214 = CARTESIAN_POINT ( 'NONE',  ( 4.763139720814407951, 2.750000000000002665, -120.2500000000000284 ) ) ;
#23215 = CARTESIAN_POINT ( 'NONE',  ( 135.0000000000000284, -7.637914190097514933, -8.088422893840236938 ) ) ;
#23216 = CARTESIAN_POINT ( 'NONE',  ( 0.000000000000000000, 5.999999999999977796, -154.2113248654052313 ) ) ;
#23217 = VERTEX_POINT ( 'NONE', #11081 ) ;
#23218 = CARTESIAN_POINT ( 'NONE',  ( 22.87500000000019895, 5.551115123125782702E-14, 2.649519052838333888 ) ) ;
#23219 = DIRECTION ( 'NONE',  ( -0.000000000000000000, -0.000000000000000000, -1.000000000000000000 ) ) ;
#23220 = EDGE_CURVE ( 'NONE', #4196, #14683, #846, .T. ) ;
#23221 = AXIS2_PLACEMENT_3D ( 'NONE', #13639, #16108, #30338 ) ;
#23222 = ORIENTED_EDGE ( 'NONE', *, *, #28211, .T. ) ;
#23223 = CARTESIAN_POINT ( 'NONE',  ( 108.6872167782374277, 1.849990392679591977, 0.7662911109078888172 ) ) ;
#23224 = CARTESIAN_POINT ( 'NONE',  ( 151.3988248654052313, 3.889087296526011706, 3.889087296526011706 ) ) ;
#23225 = CARTESIAN_POINT ( 'NONE',  ( 112.9372167782374987, -0.7662911109076785410, 1.849990392679591977 ) ) ;
#23226 = CARTESIAN_POINT ( 'NONE',  ( 3.608439182435180470, 6.249999999999982236, -110.6919872981078043 ) ) ;
#23227 = CARTESIAN_POINT ( 'NONE',  ( 3.464101615137852974, 5.999999999999884537, -108.4136751345947971 ) ) ;
#23228 =( BOUNDED_CURVE ( )  B_SPLINE_CURVE ( 2, ( #10550, #1150, #15337, #27108, #10401, #13337, #22679, #24814, #20231 ),
 .UNSPECIFIED., .F., .T. ) 
 B_SPLINE_CURVE_WITH_KNOTS ( ( 3, 2, 2, 2, 3 ),
 ( 0.05277777777777778456, 0.05370370370370370489, 0.05555555555555555247, 0.05740740740740740700, 0.05833333333333332732 ),
 .UNSPECIFIED. ) 
 CURVE ( )  GEOMETRIC_REPRESENTATION_ITEM ( )  RATIONAL_B_SPLINE_CURVE ( ( 0.9330127018922194093, 0.9330127018922198534, 1.000000000000000000, 0.8660254037844388186, 1.000000000000000000, 0.8660254037844388186, 1.000000000000000000, 0.9330127018922199644, 0.9330127018922194093 ) ) 
 REPRESENTATION_ITEM ( '' )  );
#23229 = PRESENTATION_LAYER_ASSIGNMENT (  '', '', ( #15387 ) ) ;
#23230 = CARTESIAN_POINT ( 'NONE',  ( 10.00000000000014744, 1.983323942878633561, 0.6855453763663131861 ) ) ;
#23231 = ORIENTED_EDGE ( 'NONE', *, *, #24477, .T. ) ;
#23232 = VERTEX_POINT ( 'NONE', #24082 ) ;
#23233 = DIRECTION ( 'NONE',  ( -1.000000000000000000, 0.000000000000000000, 0.000000000000000000 ) ) ;
#23234 = CARTESIAN_POINT ( 'NONE',  ( 137.6250000000000284, 0.000000000000000000, -6.000000000000005329 ) ) ;
#23235 =( BOUNDED_CURVE ( )  B_SPLINE_CURVE ( 2, ( #25812, #9078, #2609, #23227, #16039, #21366, #18325, #11422, #27639 ),
 .UNSPECIFIED., .F., .F. ) 
 B_SPLINE_CURVE_WITH_KNOTS ( ( 3, 2, 2, 2, 3 ),
 ( 0.5416666666666667407, 0.5425925925925926263, 0.5444444444444443976, 0.5462962962962962798, 0.5472222222222221655 ),
 .UNSPECIFIED. ) 
 CURVE ( )  GEOMETRIC_REPRESENTATION_ITEM ( )  RATIONAL_B_SPLINE_CURVE ( ( 0.9330127018922194093, 0.9330127018922234061, 1.000000000000000000, 0.8660254037844388186, 1.000000000000000000, 0.8660254037844388186, 1.000000000000000000, 0.9330127018922234061, 0.9330127018922194093 ) ) 
 REPRESENTATION_ITEM ( '' )  );
#23236 = CARTESIAN_POINT ( 'NONE',  ( -3.608439182435052128, -6.250000000000110134, -138.4419872981078186 ) ) ;
#23237 = CARTESIAN_POINT ( 'NONE',  ( -4.999999999999886313, -10.00000000000000888, 5.000000000000004441 ) ) ;
#23238 = CARTESIAN_POINT ( 'NONE',  ( -5.999999999999963585, 1.780251999655701777E-13, -93.83632486540518869 ) ) ;
#23239 = CARTESIAN_POINT ( 'NONE',  ( 23.37500000000000711, -1.414213562373090038, 1.414213562373034527 ) ) ;
#23240 = CYLINDRICAL_SURFACE ( 'NONE', #29889, 6.000000000000000888 ) ;
#23241 = CARTESIAN_POINT ( 'NONE',  ( -5.412658773652684552, -3.125000000000099920, -67.43301270189222407 ) ) ;
#23242 = VECTOR ( 'NONE', #28644, 1000.000000000000000 ) ;
#23243 = CARTESIAN_POINT ( 'NONE',  ( 141.1726497308104342, -5.000000000000004441, 0.000000000000000000 ) ) ;
#23244 = DIRECTION ( 'NONE',  ( 0.000000000000000000, -1.000000000000000000, -8.881784197001262184E-16 ) ) ;
#23245 = CARTESIAN_POINT ( 'NONE',  ( 0.000000000000000000, 5.999999999999977796, -73.78867513459485394 ) ) ;
#23246 = CARTESIAN_POINT ( 'NONE',  ( 135.0000000000000284, -11.07692307692306777, -4.615384615384604317 ) ) ;
#23247 = TOROIDAL_SURFACE ( 'NONE', #9989, 16.50000000000000355, 1.000000000000000000 ) ;
#23248 = CARTESIAN_POINT ( 'NONE',  ( 24.83473542850078530, -0.1527816007967785494, -2.165264571499343482 ) ) ;
#23249 = DIRECTION ( 'NONE',  ( -7.147005652999508048E-36, 5.642372883946980038E-36, 1.000000000000000000 ) ) ;
#23250 = CARTESIAN_POINT ( 'NONE',  ( 110.0624999999998437, 2.499999999999994671, 1.035533905932809473 ) ) ;
#23251 = ADVANCED_FACE ( 'NONE', ( #25937 ), #5328, .T. ) ;
#23252 = CARTESIAN_POINT ( 'NONE',  ( -5.999999999999963585, 1.780251999655701777E-13, -95.33632486540520290 ) ) ;
#23253 = ADVANCED_FACE ( 'NONE', ( #740 ), #8540, .T. ) ;
#23254 = CARTESIAN_POINT ( 'NONE',  ( -2.775557561562891351E-14, -5.500000000000115463, -120.7500000000000284 ) ) ;
#23255 = FACE_OUTER_BOUND ( 'NONE', #29457, .T. ) ;
#23256 = CARTESIAN_POINT ( 'NONE',  ( 3.608439182435180470, 6.249999999999982236, -144.5580127018922383 ) ) ;
#23257 =( NAMED_UNIT ( * ) SI_UNIT ( $, .STERADIAN. ) SOLID_ANGLE_UNIT ( ) );
#23258 = ORIENTED_EDGE ( 'NONE', *, *, #15356, .T. ) ;
#23259 = CARTESIAN_POINT ( 'NONE',  ( -2.775557561562891351E-14, -5.500000000000115463, -57.75000000000002132 ) ) ;
#23260 = DIRECTION ( 'NONE',  ( 0.000000000000000000, 0.000000000000000000, -1.000000000000000000 ) ) ;
#23261 = VERTEX_POINT ( 'NONE', #18256 ) ;
#23262 = CARTESIAN_POINT ( 'NONE',  ( 119.9372167782374277, -0.7662911109077388261, 1.849990392679652151 ) ) ;
#23263 = CARTESIAN_POINT ( 'NONE',  ( 137.7187500000000284, 2.485281374238556218, -6.000000000000005329 ) ) ;
#23264 = CARTESIAN_POINT ( 'NONE',  ( -5.412658773652739619, 3.124999999999975131, -104.3169872981078470 ) ) ;
#23265 = CARTESIAN_POINT ( 'NONE',  ( 138.7425748654052313, -2.278174593052352925, -5.499999999999671374 ) ) ;
#23266 = CARTESIAN_POINT ( 'NONE',  ( 133.4062500000000568, 6.000000000000005329, -2.485281374238555774 ) ) ;
#23267 = CARTESIAN_POINT ( 'NONE',  ( 6.000000000000000888, -1.859271017917181981E-14, -84.08632486540520290 ) ) ;
#23268 = AXIS2_PLACEMENT_3D ( 'NONE', #19542, #12055, #185 ) ;
#23269 = CARTESIAN_POINT ( 'NONE',  ( 4.763139720814407951, -2.749999999999988454, -140.0000000000000000 ) ) ;
#23270 = ORIENTED_EDGE ( 'NONE', *, *, #30014, .T. ) ;
#23271 = CARTESIAN_POINT ( 'NONE',  ( 12.00000000000012079, 2.000000000000112799, -1.665334536937734811E-13 ) ) ;
#23272 = ORIENTED_EDGE ( 'NONE', *, *, #20991, .T. ) ;
#23273 =( BOUNDED_CURVE ( )  B_SPLINE_CURVE ( 2, ( #9969, #12596, #19347, #7640, #24081, #12449, #21792, #17648, #8236 ),
 .UNSPECIFIED., .F., .F. ) 
 B_SPLINE_CURVE_WITH_KNOTS ( ( 3, 2, 2, 2, 3 ),
 ( 0.6625000000000010880, 0.6687500000000008438, 0.6750000000000007105, 0.6812500000000004663, 0.6875000000000002220 ),
 .UNSPECIFIED. ) 
 CURVE ( )  GEOMETRIC_REPRESENTATION_ITEM ( )  RATIONAL_B_SPLINE_CURVE ( ( 0.9999999999999864553, 0.9238795325113002832, 1.000000000000000000, 0.9238795325112867385, 1.000000000000000000, 0.9238795325112867385, 1.000000000000000000, 0.9238795325112840739, 1.000000000000002665 ) ) 
 REPRESENTATION_ITEM ( '' )  );
#23274 = CARTESIAN_POINT ( 'NONE',  ( 3.175426480543072749, 5.499999999999865885, -63.12500000000001421 ) ) ;
#23275 = CARTESIAN_POINT ( 'NONE',  ( 10.00000000000015277, 1.172446178180804210, -1.967641972052887933 ) ) ;
#23276 = CARTESIAN_POINT ( 'NONE',  ( -5.999999999999919176, 1.607695154586804565, -93.90331216351297883 ) ) ;
#23277 = ORIENTED_EDGE ( 'NONE', *, *, #17077, .T. ) ;
#23278 = CARTESIAN_POINT ( 'NONE',  ( -4.999999999999990230, -55.00000000000002132, -8.000000000000007105 ) ) ;
#23279 = CARTESIAN_POINT ( 'NONE',  ( 107.0622167782373708, -1.849990392679381701, 0.7662911109079489913 ) ) ;
#23280 = CYLINDRICAL_SURFACE ( 'NONE', #1777, 2.000000000000012879 ) ;
#23281 =( BOUNDED_CURVE ( )  B_SPLINE_CURVE ( 2, ( #4024, #27515, #20798, #20475, #1577, #8491, #25372, #6493, #13757 ),
 .UNSPECIFIED., .F., .T. ) 
 B_SPLINE_CURVE_WITH_KNOTS ( ( 3, 2, 2, 2, 3 ),
 ( 0.2249999999999999778, 0.2259259259259259744, 0.2277777777777777457, 0.2296296296296296280, 0.2305555555555556246 ),
 .UNSPECIFIED. ) 
 CURVE ( )  GEOMETRIC_REPRESENTATION_ITEM ( )  RATIONAL_B_SPLINE_CURVE ( ( 0.9330127018922194093, 0.9330127018922154125, 1.000000000000000000, 0.8660254037844388186, 1.000000000000000000, 0.8660254037844388186, 1.000000000000000000, 0.9330127018922154125, 0.9330127018922194093 ) ) 
 REPRESENTATION_ITEM ( '' )  );
#23282 = EDGE_CURVE ( 'NONE', #17182, #9697, #3987, .T. ) ;
#23283 = CYLINDRICAL_SURFACE ( 'NONE', #28470, 6.000000000000000888 ) ;
#23284 = CARTESIAN_POINT ( 'NONE',  ( 121.0002832217622739, -1.308140751793557266, -1.308140751793529510 ) ) ;
#23285 = EDGE_CURVE ( 'NONE', #10891, #8542, #21070, .T. ) ;
#23286 = CARTESIAN_POINT ( 'NONE',  ( 4.763139720814407951, 2.750000000000002665, -144.2500000000000000 ) ) ;
#23287 = CARTESIAN_POINT ( 'NONE',  ( 140.0676280679787169, -9.491795069345080549, -7.344273253287639136 ) ) ;
#23288 = CARTESIAN_POINT ( 'NONE',  ( -3.175426480542816510, 5.499999999999865885, -136.3750000000000568 ) ) ;
#23289 = CARTESIAN_POINT ( 'NONE',  ( 2.775557561562891351E-14, -6.250000000000061284, -157.1830127018922667 ) ) ;
#23290 = CARTESIAN_POINT ( 'NONE',  ( 6.000000000000000888, 7.762456499804234384E-14, -117.0863248654052171 ) ) ;
#23291 = CARTESIAN_POINT ( 'NONE',  ( 3.175426480543072749, 5.499999999999865885, -81.12500000000002842 ) ) ;
#23292 = DIRECTION ( 'NONE',  ( -0.000000000000000000, -0.000000000000000000, -1.000000000000000000 ) ) ;
#23293 = CARTESIAN_POINT ( 'NONE',  ( 3.175426480543072749, 5.499999999999865885, -75.12500000000001421 ) ) ;
#23294 = CARTESIAN_POINT ( 'NONE',  ( -5.999999999999963585, -1.487416814333745711E-14, -76.41367513459481131 ) ) ;
#23295 = DIRECTION ( 'NONE',  ( -1.000000000000000000, 3.469446951953694061E-16, 0.000000000000000000 ) ) ;
#23296 = CARTESIAN_POINT ( 'NONE',  ( 159.2812500000000284, 2.485281374238585972, 6.000000000000005329 ) ) ;
#23297 =( NAMED_UNIT ( * ) SI_UNIT ( $, .STERADIAN. ) SOLID_ANGLE_UNIT ( ) );
#23298 = CARTESIAN_POINT ( 'NONE',  ( 19.81250000000009237, 0.8284271247463557142, -2.000000000000091926 ) ) ;
#23299 = CARTESIAN_POINT ( 'NONE',  ( 138.7574251345947971, -2.278174593051671692, 5.500000000000352607 ) ) ;
#23300 = DIRECTION ( 'NONE',  ( 0.000000000000000000, 0.000000000000000000, 1.000000000000000000 ) ) ;
#23301 = CARTESIAN_POINT ( 'NONE',  ( 118.0622167782374277, -1.849990392679381701, 0.7662911109079489913 ) ) ;
#23302 = CARTESIAN_POINT ( 'NONE',  ( -3.464101615137725076, 5.999999999999979572, -139.0863248654051745 ) ) ;
#23303 = ORIENTED_EDGE ( 'NONE', *, *, #8147, .F. ) ;
#23304 = CARTESIAN_POINT ( 'NONE',  ( 158.2500000000000284, -6.000000000000005329, 0.000000000000000000 ) ) ;
#23305 = CYLINDRICAL_SURFACE ( 'NONE', #24379, 0.5000000000000004441 ) ;
#23306 = CARTESIAN_POINT ( 'NONE',  ( 114.1252832217622313, -8.326672684688674053E-14, -1.849990392679412565 ) ) ;
#23307 = CARTESIAN_POINT ( 'NONE',  ( 3.175426480543072749, 5.499999999999865885, -153.1250000000000284 ) ) ;
#23308 = ORIENTED_EDGE ( 'NONE', *, *, #29570, .T. ) ;
#23309 = ORIENTED_EDGE ( 'NONE', *, *, #24446, .T. ) ;
#23310 = EDGE_CURVE ( 'NONE', #27987, #28056, #24178, .T. ) ;
#23311 = CARTESIAN_POINT ( 'NONE',  ( -4.763139720814407951, 2.749999999999946709, -89.75000000000000000 ) ) ;
#23312 = AXIS2_PLACEMENT_3D ( 'NONE', #22299, #5999, #29499 ) ;
#23313 = CARTESIAN_POINT ( 'NONE',  ( -3.608439182435052128, -6.250000000000110134, -109.3080127018922809 ) ) ;
#23314 = ORIENTED_EDGE ( 'NONE', *, *, #12182, .F. ) ;
#23315 = CARTESIAN_POINT ( 'NONE',  ( 1.000000000000000888, 0.000000000000000000, 0.000000000000000000 ) ) ;
#23316 = CARTESIAN_POINT ( 'NONE',  ( 5.999486246981976301, -9.219878802943842544, -25.40874315777524828 ) ) ;
#23317 = ORIENTED_EDGE ( 'NONE', *, *, #10694, .F. ) ;
#23318 =( BOUNDED_CURVE ( )  B_SPLINE_CURVE ( 2, ( #15205, #24237, #26539, #29444, #13075, #22408, #1345, #8419, #10756 ),
 .UNSPECIFIED., .F., .T. ) 
 B_SPLINE_CURVE_WITH_KNOTS ( ( 3, 2, 2, 2, 3 ),
 ( 0.3249999999999999556, 0.3259259259259259522, 0.3277777777777777235, 0.3296296296296296058, 0.3305555555555556024 ),
 .UNSPECIFIED. ) 
 CURVE ( )  GEOMETRIC_REPRESENTATION_ITEM ( )  RATIONAL_B_SPLINE_CURVE ( ( 0.9330127018922194093, 0.9330127018922154125, 1.000000000000000000, 0.8660254037844388186, 1.000000000000000000, 0.8660254037844388186, 1.000000000000000000, 0.9330127018922154125, 0.9330127018922194093 ) ) 
 REPRESENTATION_ITEM ( '' )  );
#23319 = EDGE_CURVE ( 'NONE', #6844, #19684, #25274, .T. ) ;
#23320 = CARTESIAN_POINT ( 'NONE',  ( -4.763139720814407951, 2.749999999999946709, -170.7500000000000000 ) ) ;
#23321 = CARTESIAN_POINT ( 'NONE',  ( -3.464101615137757051, -5.999999999999979572, -80.66367513459479710 ) ) ;
#23322 = CARTESIAN_POINT ( 'NONE',  ( -6.350852961085760029, -1.281975124255709124E-13, -157.1250000000000284 ) ) ;
#23323 = CARTESIAN_POINT ( 'NONE',  ( 111.0624999999998295, 2.500000000000055067, 1.035533905932929599 ) ) ;
#23324 = CARTESIAN_POINT ( 'NONE',  ( 3.175426480543072749, 5.499999999999865885, -99.12500000000005684 ) ) ;
#23325 = CARTESIAN_POINT ( 'NONE',  ( 20.96132486540536277, 5.551115123125782702E-14, 2.500000000000002220 ) ) ;
#23326 = CARTESIAN_POINT ( 'NONE',  ( 146.3363248654052029, 0.000000000000000000, -5.500000000000005329 ) ) ;
#23327 = CARTESIAN_POINT ( 'NONE',  ( 4.763139720814407951, 2.750000000000002665, -96.25000000000000000 ) ) ;
#23328 = DIRECTION ( 'NONE',  ( -0.000000000000000000, 0.2307692307692307543, -0.9730085108210398959 ) ) ;
#23329 = SURFACE_STYLE_USAGE ( .BOTH. , #4405 ) ;
#23330 = CARTESIAN_POINT ( 'NONE',  ( -6.000000000000000888, 1.067854986875958443E-15, 7.560779664488942560E-35 ) ) ;
#23331 = ORIENTED_EDGE ( 'NONE', *, *, #4461, .T. ) ;
#23332 = CARTESIAN_POINT ( 'NONE',  ( 12.31250000000004974, -1.097466725451499370, -2.649519052838358757 ) ) ;
#23333 = CARTESIAN_POINT ( 'NONE',  ( 112.3749999999999289, -1.767766952966320915, 1.767766952966431937 ) ) ;
#23334 = CARTESIAN_POINT ( 'NONE',  ( -5.999999999999968026, -1.607695154586722186, -161.8466878364870354 ) ) ;
#23335 = CARTESIAN_POINT ( 'NONE',  ( 105.5627832217622597, 0.7662911109077686911, 1.849990392679772278 ) ) ;
#23336 = CARTESIAN_POINT ( 'NONE',  ( 5.196152422706629359, -2.999999999999988898, -85.71132486540523132 ) ) ;
#23337 = EDGE_LOOP ( 'NONE', ( #14211, #22389, #8736, #9430 ) ) ;
#23338 = VECTOR ( 'NONE', #8470, 1000.000000000000000 ) ;
#23339 = CARTESIAN_POINT ( 'NONE',  ( 0.000000000000000000, -15.50000000000001421, -8.000000000000007105 ) ) ;
#23340 = CARTESIAN_POINT ( 'NONE',  ( 3.464101615137757051, -5.999999999999979572, -169.8363248654052029 ) ) ;
#23341 = CARTESIAN_POINT ( 'NONE',  ( 105.5622167782374419, 1.849990392679591977, -0.7662911109075883909 ) ) ;
#23342 = DIRECTION ( 'NONE',  ( -7.147005652999508048E-36, 5.642372883946980038E-36, 1.000000000000000000 ) ) ;
#23343 = EDGE_LOOP ( 'NONE', ( #1622, #12321, #10303, #1771 ) ) ;
#23344 = DIRECTION ( 'NONE',  ( -7.147005652999508048E-36, 5.642372883946980038E-36, 1.000000000000000000 ) ) ;
#23345 = ADVANCED_FACE ( 'NONE', ( #14696 ), #26336, .F. ) ;
#23346 = CARTESIAN_POINT ( 'NONE',  ( 150.7500000000000284, -6.000000000000005329, 0.000000000000000000 ) ) ;
#23347 = ORIENTED_EDGE ( 'NONE', *, *, #1434, .F. ) ;
#23348 = TOROIDAL_SURFACE ( 'NONE', #6153, 28.99999999999999645, 1.000000000000000000 ) ;
#23349 = EDGE_CURVE ( 'NONE', #18727, #5920, #21455, .T. ) ;
#23350 = CARTESIAN_POINT ( 'NONE',  ( 0.000000000000000000, 5.499999999999991118, -112.5000000000000426 ) ) ;
#23351 = CARTESIAN_POINT ( 'NONE',  ( 20.75000000000012790, -1.873492889144789952, 1.873492889144845464 ) ) ;
#23352 = CARTESIAN_POINT ( 'NONE',  ( -5.412658773652684552, -3.125000000000099920, -128.9330127018922383 ) ) ;
#23353 = EDGE_LOOP ( 'NONE', ( #30194, #3497 ) ) ;
#23354 = CARTESIAN_POINT ( 'NONE',  ( -0.5000000000000004441, -9.500000000000008882, 7.500000000000007105 ) ) ;
#23355 = CARTESIAN_POINT ( 'NONE',  ( 7.216878364870455975, -6.409875621278545621E-14, -170.9419872981078470 ) ) ;
#23356 = CARTESIAN_POINT ( 'NONE',  ( 107.9374999999997726, 2.500000000000144773, -1.035533905932508825 ) ) ;
#23357 = ADVANCED_FACE ( 'NONE', ( #14989 ), #19595, .T. ) ;
#23358 = CARTESIAN_POINT ( 'NONE',  ( 153.6636751345948255, 0.000000000000000000, 5.500000000000005329 ) ) ;
#23359 = DIRECTION ( 'NONE',  ( -7.147005652999508048E-36, 5.642372883946980038E-36, 1.000000000000000000 ) ) ;
#23360 = LINE ( 'NONE', #9058, #23434 ) ;
#23361 = CARTESIAN_POINT ( 'NONE',  ( 108.5627832217621886, 0.7662911109077987781, 1.849990392679652151 ) ) ;
#23362 = CARTESIAN_POINT ( 'NONE',  ( -5.412658773652739619, 3.124999999999975131, -177.1830127018922383 ) ) ;
#23363 = CARTESIAN_POINT ( 'NONE',  ( 110.7886751345946834, -1.999999999999946265, 0.000000000000000000 ) ) ;
#23364 = CARTESIAN_POINT ( 'NONE',  ( 116.0000000000000142, 0.000000000000000000, 0.000000000000000000 ) ) ;
#23365 = CARTESIAN_POINT ( 'NONE',  ( 160.8919244128742605, -11.51465293479089524, -3.380337924145041750 ) ) ;
#23366 = CARTESIAN_POINT ( 'NONE',  ( 4.763139720814407951, -2.749999999999988454, -125.0000000000000000 ) ) ;
#23367 = CARTESIAN_POINT ( 'NONE',  ( -1.000000000000000888, 9.000000000000007105, 5.000000000000004441 ) ) ;
#23368 = CARTESIAN_POINT ( 'NONE',  ( 5.999999999999999112, 2.951592740943527306E-14, -154.5863248654052029 ) ) ;
#23369 = VERTEX_POINT ( 'NONE', #241 ) ;
#23370 = CARTESIAN_POINT ( 'NONE',  ( 21.74999999999999289, 1.873492889144956486, 1.873492889144734441 ) ) ;
#23371 = CARTESIAN_POINT ( 'NONE',  ( 18.03867513459492145, 1.665334536937734811E-13, -2.500000000000057732 ) ) ;
#23372 = CARTESIAN_POINT ( 'NONE',  ( 6.000000000000000888, 1.743066579297358182E-13, -83.16367513459481131 ) ) ;
#23373 = VERTEX_POINT ( 'NONE', #28778 ) ;
#23374 = CARTESIAN_POINT ( 'NONE',  ( 110.5622167782373992, 1.849990392679501827, -0.7662911109077087390 ) ) ;
#23375 = CARTESIAN_POINT ( 'NONE',  ( 116.7113248654051318, 2.000000000000057288, 0.000000000000000000 ) ) ;
#23376 = CARTESIAN_POINT ( 'NONE',  ( 110.1872167782374703, -1.849990392679501827, -0.7662911109076485650 ) ) ;
#23377 = CARTESIAN_POINT ( 'NONE',  ( 2.775557561562891351E-14, 6.250000000000033751, -109.0669872981078186 ) ) ;
#23378 = FILL_AREA_STYLE ('',( #14040 ) ) ;
#23379 = FACE_OUTER_BOUND ( 'NONE', #24136, .T. ) ;
#23380 = EDGE_LOOP ( 'NONE', ( #29617, #28140, #12477, #8860 ) ) ;
#23381 = ORIENTED_EDGE ( 'NONE', *, *, #22991, .F. ) ;
#23382 = CARTESIAN_POINT ( 'NONE',  ( 20.97617513459490723, -1.035533905932689347, -2.500000000000024425 ) ) ;
#23383 = CARTESIAN_POINT ( 'NONE',  ( 133.2187500000000568, 2.485281374238555774, -6.000000000000005329 ) ) ;
#23384 = ADVANCED_FACE ( 'NONE', ( #17157 ), #386, .F. ) ;
#23385 = CARTESIAN_POINT ( 'NONE',  ( 2.775557561562891351E-14, -6.250000000000061284, -138.3169872981078186 ) ) ;
#23386 = CARTESIAN_POINT ( 'NONE',  ( 11.06250000000009948, -1.097466725451439196, -2.649519052838478661 ) ) ;
#23387 = DIRECTION ( 'NONE',  ( -1.000000000000000000, 0.000000000000000000, 0.000000000000000000 ) ) ;
#23388 = CARTESIAN_POINT ( 'NONE',  ( 19.00000000000020961, 2.000000000000223821, -5.551115123125782702E-14 ) ) ;
#23389 = CARTESIAN_POINT ( 'NONE',  ( 6.000000000000000888, -1.859271017917181981E-14, -171.0863248654052029 ) ) ;
#23390 = EDGE_CURVE ( 'NONE', #9852, #7029, #6233, .T. ) ;
#23391 = CARTESIAN_POINT ( 'NONE',  ( -5.412658773652739619, 3.124999999999975131, -61.68301270189224539 ) ) ;
#23392 = EDGE_CURVE ( 'NONE', #11534, #17549, #27305, .T. ) ;
#23393 = CARTESIAN_POINT ( 'NONE',  ( 146.5163997308104058, 4.999999999999989342, 2.071067811865468400 ) ) ;
#23394 = CARTESIAN_POINT ( 'NONE',  ( 11.72617513459494809, -2.499999999999964473, 1.035533905932749299 ) ) ;
#23395 = CARTESIAN_POINT ( 'NONE',  ( 0.000000000000000000, -5.999999999999991118, -160.9613248654052597 ) ) ;
#23396 = CARTESIAN_POINT ( 'NONE',  ( -3.464101615137757051, -5.999999999999979572, -146.6636751345948255 ) ) ;
#23397 = B_SPLINE_CURVE_WITH_KNOTS ( 'NONE', 3,
 ( #12475, #17522, #13086, #21813, #3194, #12620, #5799, #5497, #22418, #29304, #17223, #8259 ),
 .UNSPECIFIED., .F., .F.,
 ( 4, 2, 2, 2, 2, 4 ),
 ( 1.086937293533992048E-16, 0.0007621846814068694662, 0.001524369362813630079, 0.001905461703517011361, 0.002286554044220393076, 0.003048738725627156941 ),
 .UNSPECIFIED. ) ;
#23398 = CARTESIAN_POINT ( 'NONE',  ( 156.2886751345948255, 5.500000000000005329, 0.000000000000000000 ) ) ;
#23399 = CARTESIAN_POINT ( 'NONE',  ( -5.999999999999963585, 8.134310703387671600E-14, -114.8363248654052171 ) ) ;
#23400 = CARTESIAN_POINT ( 'NONE',  ( 108.2499999999998863, 5.551115123125782702E-14, 2.499999999999946709 ) ) ;
#23401 = CARTESIAN_POINT ( 'NONE',  ( 1.110223024625164183E-16, -2.000000000000012879, -1.776356839400262692E-15 ) ) ;
#23402 = CARTESIAN_POINT ( 'NONE',  ( -4.999999999999886313, -15.00000000000001421, 7.500000000000007105 ) ) ;
#23403 = ORIENTED_EDGE ( 'NONE', *, *, #12845, .F. ) ;
#23404 = COLOUR_RGB ( '', 0.31764706, 0.68627451, 0.89019608) ;
#23405 = CARTESIAN_POINT ( 'NONE',  ( -6.350852961085760029, -1.281975124255709124E-13, -56.62500000000003553 ) ) ;
#23406 = FACE_OUTER_BOUND ( 'NONE', #20115, .T. ) ;
#23407 = CARTESIAN_POINT ( 'NONE',  ( 5.196152422706629359, 3.000000000000002665, -62.96132486540523132 ) ) ;
#23408 =( BOUNDED_CURVE ( )  B_SPLINE_CURVE ( 2, ( #3250, #17131, #507, #9903, #14821, #950, #24164, #3106, #24303 ),
 .UNSPECIFIED., .F., .T. ) 
 B_SPLINE_CURVE_WITH_KNOTS ( ( 3, 2, 2, 2, 3 ),
 ( 0.2374999999999997391, 0.2437499999999995226, 0.2499999999999992784, 0.2562499999999990896, 0.2624999999999988454 ),
 .UNSPECIFIED. ) 
 CURVE ( )  GEOMETRIC_REPRESENTATION_ITEM ( )  RATIONAL_B_SPLINE_CURVE ( ( 1.000000000000003775, 0.9238795325112830747, 1.000000000000000000, 0.9238795325112867385, 1.000000000000000000, 0.9238795325112867385, 1.000000000000000000, 0.9238795325113002832, 0.9999999999999864553 ) ) 
 REPRESENTATION_ITEM ( '' )  );
#23409 = ORIENTED_EDGE ( 'NONE', *, *, #2385, .T. ) ;
#23410 = CARTESIAN_POINT ( 'NONE',  ( 106.9374999999997868, 2.500000000000055067, -1.035533905932568777 ) ) ;
#23411 = CARTESIAN_POINT ( 'NONE',  ( 140.2500000000000284, -6.000000000000005329, 0.000000000000000000 ) ) ;
#23412 = CARTESIAN_POINT ( 'NONE',  ( -3.608439182435052128, -6.250000000000110134, -105.4419872981078612 ) ) ;
#23413 = CARTESIAN_POINT ( 'NONE',  ( -5.999999999999963585, -1.487416814333745711E-14, -153.8363248654052313 ) ) ;
#23414 =( BOUNDED_CURVE ( )  B_SPLINE_CURVE ( 2, ( #19510, #21957, #10286, #28841, #890, #28991, #16778, #14476, #2748 ),
 .UNSPECIFIED., .F., .T. ) 
 B_SPLINE_CURVE_WITH_KNOTS ( ( 3, 2, 2, 2, 3 ),
 ( 0.2972222222222222765, 0.2981481481481481621, 0.3000000000000000444, 0.3018518518518518157, 0.3027777777777777013 ),
 .UNSPECIFIED. ) 
 CURVE ( )  GEOMETRIC_REPRESENTATION_ITEM ( )  RATIONAL_B_SPLINE_CURVE ( ( 0.9330127018922194093, 0.9330127018922234061, 1.000000000000000000, 0.8660254037844388186, 1.000000000000000000, 0.8660254037844388186, 1.000000000000000000, 0.9330127018922234061, 0.9330127018922194093 ) ) 
 REPRESENTATION_ITEM ( '' )  );
#23415 = CARTESIAN_POINT ( 'NONE',  ( 132.7500000000000284, -6.000000000000005329, 0.000000000000000000 ) ) ;
#23416 = FACE_OUTER_BOUND ( 'NONE', #8078, .T. ) ;
#23417 = VERTEX_POINT ( 'NONE', #9778 ) ;
#23418 = ADVANCED_FACE ( 'NONE', ( #19155 ), #5287, .T. ) ;
#23419 = CARTESIAN_POINT ( 'NONE',  ( -4.763139720814407951, -2.750000000000016431, -134.5000000000000000 ) ) ;
#23420 = ORIENTED_EDGE ( 'NONE', *, *, #2385, .F. ) ;
#23421 = ORIENTED_EDGE ( 'NONE', *, *, #19695, .F. ) ;
#23422 = CARTESIAN_POINT ( 'NONE',  ( 3.175426480543072749, 5.499999999999865885, -61.62500000000000000 ) ) ;
#23423 = CARTESIAN_POINT ( 'NONE',  ( 3.464101615137757051, -5.999999999999979572, -164.4136751345947971 ) ) ;
#23424 = FACE_OUTER_BOUND ( 'NONE', #21006, .T. ) ;
#23425 = EDGE_CURVE ( 'NONE', #18908, #6908, #18934, .T. ) ;
#23426 = CARTESIAN_POINT ( 'NONE',  ( 2.775557561562891351E-14, 6.250000000000033751, -81.43301270189223828 ) ) ;
#23427 = CARTESIAN_POINT ( 'NONE',  ( 3.464101615137852974, 5.999999999999884537, -139.9136751345948255 ) ) ;
#23428 = CARTESIAN_POINT ( 'NONE',  ( 107.2497167782375129, -1.308140751793585022, -1.308140751793640533 ) ) ;
#23429 = CYLINDRICAL_SURFACE ( 'NONE', #16621, 6.000000000000000888 ) ;
#23430 = CARTESIAN_POINT ( 'NONE',  ( 119.8752832217623450, -1.849990392679523588, 0.000000000000000000 ) ) ;
#23431 = CONTEXT_DEPENDENT_SHAPE_REPRESENTATION ( #6920, #10650 ) ;
#23432 = CARTESIAN_POINT ( 'NONE',  ( 6.350852961086080661, -9.614813431917819062E-14, -148.8750000000000284 ) ) ;
#23433 = CARTESIAN_POINT ( 'NONE',  ( 0.000000000000000000, 0.000000000000000000, 0.000000000000000000 ) ) ;
#23434 = VECTOR ( 'NONE', #4129, 1000.000000000000000 ) ;
#23435 = CARTESIAN_POINT ( 'NONE',  ( -2.775557561562891351E-14, -5.500000000000115463, -134.2500000000000284 ) ) ;
#23436 = CARTESIAN_POINT ( 'NONE',  ( 7.216878364870455975, -6.409875621278545621E-14, -161.3080127018922667 ) ) ;
#23437 = CARTESIAN_POINT ( 'NONE',  ( 0.000000000000000000, 0.000000000000000000, 0.000000000000000000 ) ) ;
#23438 = CARTESIAN_POINT ( 'NONE',  ( 4.763139720814407951, 2.750000000000002665, -75.25000000000004263 ) ) ;
#23439 = AXIS2_PLACEMENT_3D ( 'NONE', #26026, #13959, #23742 ) ;
#23440 = FILL_AREA_STYLE_COLOUR ( '', #29330 ) ;
#23441 = CARTESIAN_POINT ( 'NONE',  ( -2.775557561562891351E-14, -5.500000000000115463, -65.25000000000002842 ) ) ;
#23442 = CARTESIAN_POINT ( 'NONE',  ( 5.196152422706629359, 3.000000000000002665, -155.0386751345948539 ) ) ;
#23443 = DIRECTION ( 'NONE',  ( 1.000000000000000000, -0.000000000000000000, -0.000000000000000000 ) ) ;
#23444 = CARTESIAN_POINT ( 'NONE',  ( 0.000000000000000000, 0.000000000000000000, 0.000000000000000000 ) ) ;
#23445 = CARTESIAN_POINT ( 'NONE',  ( 156.2812500000000284, 2.485281374238585972, 6.000000000000005329 ) ) ;
#23446 = CARTESIAN_POINT ( 'NONE',  ( 18.25000000000009948, 1.110223024625156540E-13, 1.999999999999946265 ) ) ;
#23447 = VECTOR ( 'NONE', #13700, 1000.000000000000000 ) ;
#23448 = DIRECTION ( 'NONE',  ( -7.147005652999508048E-36, 5.642372883946980038E-36, 1.000000000000000000 ) ) ;
#23449 = CARTESIAN_POINT ( 'NONE',  ( 118.4997167782374135, 1.308140751793696044, -1.308140751793640533 ) ) ;
#23450 = DIRECTION ( 'NONE',  ( 0.000000000000000000, 0.000000000000000000, -1.000000000000000000 ) ) ;
#23451 = ORIENTED_EDGE ( 'NONE', *, *, #7915, .F. ) ;
#23452 = CARTESIAN_POINT ( 'NONE',  ( 150.1875000000000284, 4.242640687119269671, 4.242640687119298093 ) ) ;
#23453 = CARTESIAN_POINT ( 'NONE',  ( 5.999999999999999112, 2.951592740943527306E-14, -156.6636751345948255 ) ) ;
#23454 = VECTOR ( 'NONE', #18986, 1000.000000000000000 ) ;
#23455 =( BOUNDED_CURVE ( )  B_SPLINE_CURVE ( 2, ( #26809, #10271, #19092, #29274, #15357, #28415, #27127, #24520, #13057 ),
 .UNSPECIFIED., .F., .F. ) 
 B_SPLINE_CURVE_WITH_KNOTS ( ( 3, 2, 2, 2, 3 ),
 ( 0.4583333333333333148, 0.4592592592592592560, 0.4611111111111111382, 0.4629629629629629650, 0.4638888888888889062 ),
 .UNSPECIFIED. ) 
 CURVE ( )  GEOMETRIC_REPRESENTATION_ITEM ( )  RATIONAL_B_SPLINE_CURVE ( ( 0.9330127018922194093, 0.9330127018922174109, 1.000000000000000000, 0.8660254037844388186, 1.000000000000000000, 0.8660254037844388186, 1.000000000000000000, 0.9330127018922174109, 0.9330127018922194093 ) ) 
 REPRESENTATION_ITEM ( '' )  );
#23456 = ADVANCED_FACE ( 'NONE', ( #29391 ), #22352, .T. ) ;
#23457 = CARTESIAN_POINT ( 'NONE',  ( 6.000000000000000888, -1.607695154586752384, -84.73066243270260145 ) ) ;
#23458 = EDGE_LOOP ( 'NONE', ( #25428, #2874, #327, #25150 ) ) ;
#23459 = VERTEX_POINT ( 'NONE', #29703 ) ;
#23460 = ADVANCED_FACE ( 'NONE', ( #22199 ), #15629, .F. ) ;
#23461 = CARTESIAN_POINT ( 'NONE',  ( 22.50000000000010303, -1.999999999999835243, 0.000000000000000000 ) ) ;
#23462 = CARTESIAN_POINT ( 'NONE',  ( -3.175426480542816510, 5.499999999999865885, -91.37500000000001421 ) ) ;
#23463 = VECTOR ( 'NONE', #7119, 1000.000000000000000 ) ;
#23464 = CIRCLE ( 'NONE', #9706, 12.00000000000000178 ) ;
#23465 = CARTESIAN_POINT ( 'NONE',  ( -3.608439182435115633, 6.249999999999965361, -108.3080127018922667 ) ) ;
#23466 = CARTESIAN_POINT ( 'NONE',  ( 3.031145847945201588, 10.57562584360013780, -30.18173774084347727 ) ) ;
#23467 = CARTESIAN_POINT ( 'NONE',  ( 157.7663997308104626, -4.999999999999989342, -2.071067811865468400 ) ) ;
#23468 = CARTESIAN_POINT ( 'NONE',  ( -4.763139720814407951, 2.749999999999946709, -163.2500000000000000 ) ) ;
#23469 = CARTESIAN_POINT ( 'NONE',  ( -7.216878364870328078, 0.000000000000000000, -48.05801270189223118 ) ) ;
#23470 = CARTESIAN_POINT ( 'NONE',  ( 135.7516005668334742, -9.165151352139671914, 8.000000000000007105 ) ) ;
#23471 = FILL_AREA_STYLE_COLOUR ( '', #27580 ) ;
#23472 = CARTESIAN_POINT ( 'NONE',  ( 4.763139720814407951, -2.749999999999988454, -170.0000000000000284 ) ) ;
#23473 = DIRECTION ( 'NONE',  ( 1.000000000000000000, 1.665334536937731113E-16, -1.526556658859586792E-16 ) ) ;
#23474 = AXIS2_PLACEMENT_3D ( 'NONE', #9452, #18833, #7129 ) ;
#23475 = CARTESIAN_POINT ( 'NONE',  ( 4.763139720814407951, -2.749999999999988454, -155.0000000000000284 ) ) ;
#23476 = CARTESIAN_POINT ( 'NONE',  ( 112.9999999999998579, 2.500000000000057732, 0.000000000000000000 ) ) ;
#23477 = CARTESIAN_POINT ( 'NONE',  ( -4.763139720814407951, 2.749999999999946709, -98.75000000000000000 ) ) ;
#23478 = SURFACE_STYLE_USAGE ( .BOTH. , #9026 ) ;
#23479 = CARTESIAN_POINT ( 'NONE',  ( 0.000000000000000000, 5.999999999999977796, 0.000000000000000000 ) ) ;
#23480 = CARTESIAN_POINT ( 'NONE',  ( 3.175426480543072749, -5.500000000000105693, -87.62500000000000000 ) ) ;
#23481 = CARTESIAN_POINT ( 'NONE',  ( 24.46132486540536632, 1.665334536937734811E-13, -2.500000000000002220 ) ) ;
#23482 = CARTESIAN_POINT ( 'NONE',  ( 135.0000000000000284, -7.344328791152317848, 8.346722065162424542 ) ) ;
#23483 = ORIENTED_EDGE ( 'NONE', *, *, #1400, .F. ) ;
#23484 = CARTESIAN_POINT ( 'NONE',  ( 11.25000000000009237, -1.873492889144900975, -1.873492889145011997 ) ) ;
#23485 = CARTESIAN_POINT ( 'NONE',  ( 114.6249999999999574, -1.767766952966431937, -1.767766952966431937 ) ) ;
#23486 = CARTESIAN_POINT ( 'NONE',  ( 9.999999999999841904, 2.000000000000057288, -4.274358644806852681E-12 ) ) ;
#23487 = CARTESIAN_POINT ( 'NONE',  ( -5.196152422706573404, -3.000000000000002665, -86.21132486540523132 ) ) ;
#23488 = ORIENTED_EDGE ( 'NONE', *, *, #10064, .T. ) ;
#23489 = CYLINDRICAL_SURFACE ( 'NONE', #6436, 6.000000000000000888 ) ;
#23490 = CARTESIAN_POINT ( 'NONE',  ( 105.8122167782375129, 0.7662911109077987781, 1.849990392679652151 ) ) ;
#23491 = ORIENTED_EDGE ( 'NONE', *, *, #25251, .F. ) ;
#23492 = EDGE_CURVE ( 'NONE', #3683, #14517, #1132, .T. ) ;
#23493 = CARTESIAN_POINT ( 'NONE',  ( 150.0000000000000284, 6.000000000000005329, 0.000000000000000000 ) ) ;
#23494 = VERTEX_POINT ( 'NONE', #13176 ) ;
#23495 = CARTESIAN_POINT ( 'NONE',  ( -4.763139720814407951, -2.750000000000016431, -113.5000000000000426 ) ) ;
#23496 = CARTESIAN_POINT ( 'NONE',  ( 24.25000000000021672, 1.873492889145067508, -1.873492889144956486 ) ) ;
#23497 =( BOUNDED_CURVE ( )  B_SPLINE_CURVE ( 2, ( #24885, #19687, #17400, #26576, #15413, #15087, #22141, #21989, #26715 ),
 .UNSPECIFIED., .F., .F. ) 
 B_SPLINE_CURVE_WITH_KNOTS ( ( 3, 2, 2, 2, 3 ),
 ( 0.1583333333333333259, 0.1592592592592592671, 0.1611111111111111216, 0.1629629629629629761, 0.1638888888888888895 ),
 .UNSPECIFIED. ) 
 CURVE ( )  GEOMETRIC_REPRESENTATION_ITEM ( )  RATIONAL_B_SPLINE_CURVE ( ( 0.9330127018922196314, 0.9330127018922185211, 1.000000000000000000, 0.8660254037844388186, 1.000000000000000000, 0.8660254037844388186, 1.000000000000000000, 0.9330127018922194093, 0.9330127018922194093 ) ) 
 REPRESENTATION_ITEM ( '' )  );
#23498 = CARTESIAN_POINT ( 'NONE',  ( 2.775557561562891351E-14, 6.250000000000033751, -133.9330127018922383 ) ) ;
#23499 = ORIENTED_EDGE ( 'NONE', *, *, #19209, .T. ) ;
#23500 = CARTESIAN_POINT ( 'NONE',  ( -4.999999999999990230, -55.00000000000002132, 7.500000000000007105 ) ) ;
#23501 = CARTESIAN_POINT ( 'NONE',  ( -3.608439182435052128, -6.250000000000110134, -171.4419872981078470 ) ) ;
#23502 = CARTESIAN_POINT ( 'NONE',  ( 107.1874999999997584, 1.035533905932779275, 2.500000000000205169 ) ) ;
#23503 = ORIENTED_EDGE ( 'NONE', *, *, #2815, .T. ) ;
#23504 = CARTESIAN_POINT ( 'NONE',  ( 0.7522227795206197776, -15.54366488976627636, -8.040203489970597417 ) ) ;
#23505 = COLOUR_RGB ( '', 0.08235294, 0.09019608, 0.10196078) ;
#23506 = CARTESIAN_POINT ( 'NONE',  ( 0.000000000000000000, 5.999999999999977796, -95.71132486540523132 ) ) ;
#23507 = CARTESIAN_POINT ( 'NONE',  ( 6.000000000000000888, -1.859271017917181981E-14, -137.1636751345948255 ) ) ;
#23508 = CARTESIAN_POINT ( 'NONE',  ( 4.763139720814407951, -2.749999999999988454, -177.5000000000000000 ) ) ;
#23509 = CARTESIAN_POINT ( 'NONE',  ( 106.4377832217622029, 1.849990392679562001, 0.7662911109078287542 ) ) ;
#23510 = CARTESIAN_POINT ( 'NONE',  ( -3.608439182435115633, 6.249999999999965361, -174.3080127018922667 ) ) ;
#23511 = CARTESIAN_POINT ( 'NONE',  ( -0.7382520721438933231, -9.130873963928037185, -4.026027341348664912 ) ) ;
#23512 = DIRECTION ( 'NONE',  ( -1.000000000000000000, -1.665334536937736783E-16, -2.220446049250315546E-16 ) ) ;
#23513 = CARTESIAN_POINT ( 'NONE',  ( 5.196152422706629359, 3.000000000000002665, -123.5386751345948255 ) ) ;
#23514 = CARTESIAN_POINT ( 'NONE',  ( 3.175426480543072749, 5.499999999999865885, -123.1250000000000426 ) ) ;
#23515 = CARTESIAN_POINT ( 'NONE',  ( 134.9999999999992895, -7.177887245073663713, -8.449849189508016778 ) ) ;
#23516 = CARTESIAN_POINT ( 'NONE',  ( 114.3511751345946408, 2.000000000000031530, 0.8284271247462955401 ) ) ;
#23517 = ORIENTED_EDGE ( 'NONE', *, *, #18079, .F. ) ;
#23518 = CARTESIAN_POINT ( 'NONE',  ( 22.62500000000008882, 2.649519052838444910, 0.000000000000000000 ) ) ;
#23519 = EDGE_CURVE ( 'NONE', #30356, #11342, #22031, .T. ) ;
#23520 = CARTESIAN_POINT ( 'NONE',  ( -0.04607149862261590567, -15.28219869613047521, 7.206732114352344176 ) ) ;
#23521 = DIRECTION ( 'NONE',  ( -1.000000000000000000, -1.067522139062651411E-16, 0.000000000000000000 ) ) ;
#23522 = CARTESIAN_POINT ( 'NONE',  ( 116.4136751345946834, 1.414213562373145550, 1.414213562373034527 ) ) ;
#23523 = ORIENTED_EDGE ( 'NONE', *, *, #9012, .T. ) ;
#23524 = CARTESIAN_POINT ( 'NONE',  ( 118.2113248654050466, -1.999999999999946265, 2.220446049250313081E-13 ) ) ;
#23525 = FACE_OUTER_BOUND ( 'NONE', #20399, .T. ) ;
#23526 = EDGE_CURVE ( 'NONE', #25268, #23117, #28258, .T. ) ;
#23527 = DIRECTION ( 'NONE',  ( -7.147005652999508048E-36, 5.642372883946980038E-36, 1.000000000000000000 ) ) ;
#23528 = ORIENTED_EDGE ( 'NONE', *, *, #9149, .T. ) ;
#23529 = ORIENTED_EDGE ( 'NONE', *, *, #17395, .F. ) ;
#23530 = CARTESIAN_POINT ( 'NONE',  ( -9.999999999999793943, 10.00000000000000888, 3.000000000000002665 ) ) ;
#23531 = CARTESIAN_POINT ( 'NONE',  ( 138.6562500000000568, -6.000000000000005329, 2.485281374238555774 ) ) ;
#23532 = ORIENTED_EDGE ( 'NONE', *, *, #26434, .T. ) ;
#23533 = CARTESIAN_POINT ( 'NONE',  ( 3.608439182435180470, -6.249999999999997335, -138.1919872981077901 ) ) ;
#23534 = LINE ( 'NONE', #9550, #27951 ) ;
#23535 = CARTESIAN_POINT ( 'NONE',  ( 12.00000000000012079, -1.873492889144789952, -1.873492889145011997 ) ) ;
#23536 = PRESENTATION_STYLE_ASSIGNMENT (( #18631 ) ) ;
#23537 = CARTESIAN_POINT ( 'NONE',  ( 20.81250000000014211, 0.8284271247461753029, -2.000000000000091926 ) ) ;
#23538 = CARTESIAN_POINT ( 'NONE',  ( -6.000000000000007105, -1.607695154586655129, -171.7693375672974128 ) ) ;
#23539 = CARTESIAN_POINT ( 'NONE',  ( 117.6488248654050039, 2.000000000000151879, -0.8284271247458149245 ) ) ;
#23540 = CARTESIAN_POINT ( 'NONE',  ( 143.8913997308104058, -2.071067811865468400, 4.999999999999989342 ) ) ;
#23541 = CARTESIAN_POINT ( 'NONE',  ( 6.000000000000000888, -1.859271017917181981E-14, -124.5863248654052171 ) ) ;
#23542 = DIRECTION ( 'NONE',  ( -0.000000000000000000, -0.000000000000000000, 1.000000000000000000 ) ) ;
#23543 = CARTESIAN_POINT ( 'NONE',  ( 5.196152422706629359, -2.999999999999988898, -139.7113248654052313 ) ) ;
#23544 = CARTESIAN_POINT ( 'NONE',  ( 24.77133704109404277, -1.424057122634293959, -1.721093397680183656 ) ) ;
#23545 = FILL_AREA_STYLE ('',( #14355 ) ) ;
#23546 = CARTESIAN_POINT ( 'NONE',  ( 110.3749999999999289, -1.767766952966209892, 1.767766952966542959 ) ) ;
#23547 = CIRCLE ( 'NONE', #24971, 1.000000000000000888 ) ;
#23548 = VECTOR ( 'NONE', #5218, 1000.000000000000114 ) ;
#23549 = LINE ( 'NONE', #7252, #1395 ) ;
#23550 = CARTESIAN_POINT ( 'NONE',  ( 140.9136751345948539, 0.000000000000000000, -5.500000000000005329 ) ) ;
#23551 = VERTEX_POINT ( 'NONE', #8674 ) ;
#23552 = EDGE_CURVE ( 'NONE', #18896, #27181, #17610, .T. ) ;
#23553 = CARTESIAN_POINT ( 'NONE',  ( -2.775557561562891351E-14, -5.500000000000115463, -54.75000000000002132 ) ) ;
#23554 = ORIENTED_EDGE ( 'NONE', *, *, #18341, .T. ) ;
#23555 = CARTESIAN_POINT ( 'NONE',  ( 106.8749999999998437, 1.767766952966320915, -1.767766952966320915 ) ) ;
#23556 = CARTESIAN_POINT ( 'NONE',  ( 141.1875000000000284, 4.242640687119269671, 4.242640687119298093 ) ) ;
#23557 = CARTESIAN_POINT ( 'NONE',  ( 3.608439182435180470, -6.249999999999997335, -102.1919872981078328 ) ) ;
#23558 = DIRECTION ( 'NONE',  ( -7.147005652999508048E-36, 5.642372883946980038E-36, 1.000000000000000000 ) ) ;
#23559 = EDGE_CURVE ( 'NONE', #4026, #10268, #25820, .T. ) ;
#23560 = CARTESIAN_POINT ( 'NONE',  ( 135.2812500000000284, 2.485281374238585972, 6.000000000000005329 ) ) ;
#23561 = CARTESIAN_POINT ( 'NONE',  ( 116.3124999999997158, -1.035533905932598975, 2.500000000000144773 ) ) ;
#23562 = AXIS2_PLACEMENT_3D ( 'NONE', #19772, #21936, #581 ) ;
#23563 = CARTESIAN_POINT ( 'NONE',  ( 3.175426480543072749, 5.499999999999865885, -133.6250000000000284 ) ) ;
#23564 = AXIS2_PLACEMENT_3D ( 'NONE', #17311, #29390, #3281 ) ;
#23565 = ORIENTED_EDGE ( 'NONE', *, *, #20069, .T. ) ;
#23566 = ORIENTED_EDGE ( 'NONE', *, *, #10585, .F. ) ;
#23567 = CARTESIAN_POINT ( 'NONE',  ( -3.464101615137725076, 5.999999999999979572, -163.0863248654051745 ) ) ;
#23568 = CARTESIAN_POINT ( 'NONE',  ( 4.763139720814407951, 2.750000000000002665, -64.75000000000002842 ) ) ;
#23569 = DIRECTION ( 'NONE',  ( -7.147005652999508048E-36, 5.642372883946980038E-36, 1.000000000000000000 ) ) ;
#23570 = LINE ( 'NONE', #16827, #1433 ) ;
#23571 = CARTESIAN_POINT ( 'NONE',  ( 3.608439182435180470, -6.249999999999997335, -80.55801270189219565 ) ) ;
#23572 = CARTESIAN_POINT ( 'NONE',  ( 119.7738248654049613, 2.000000000000061728, 0.8284271247464759513 ) ) ;
#23573 = CARTESIAN_POINT ( 'NONE',  ( 105.0622167782375840, -1.849990392679501827, 0.7662911109077686911 ) ) ;
#23574 = CARTESIAN_POINT ( 'NONE',  ( 6.000000000000000888, -6.507448562710137091E-15, -175.5863248654052029 ) ) ;
#23575 = CARTESIAN_POINT ( 'NONE',  ( 120.7502832217623308, -1.308140751793640533, 1.308140751793751555 ) ) ;
#23576 =( BOUNDED_CURVE ( )  B_SPLINE_CURVE ( 2, ( #11246, #20756, #9067, #14030, #13719, #151, #7061, #25325, #16474 ),
 .UNSPECIFIED., .F., .T. ) 
 B_SPLINE_CURVE_WITH_KNOTS ( ( 3, 2, 2, 2, 3 ),
 ( 0.2374999999999997391, 0.2437499999999999944, 0.2500000000000002220, 0.2562500000000004774, 0.2625000000000007327 ),
 .UNSPECIFIED. ) 
 CURVE ( )  GEOMETRIC_REPRESENTATION_ITEM ( )  RATIONAL_B_SPLINE_CURVE ( ( 1.000000000000003109, 0.9238795325112837409, 1.000000000000000000, 0.9238795325112867385, 1.000000000000000000, 0.9238795325112867385, 1.000000000000000000, 0.9238795325112779677, 1.000000000000008882 ) ) 
 REPRESENTATION_ITEM ( '' )  );
#23577 = CARTESIAN_POINT ( 'NONE',  ( -6.350852961085760029, -1.281975124255709124E-13, -148.1250000000000284 ) ) ;
#23578 = CARTESIAN_POINT ( 'NONE',  ( 6.000000000000000888, -1.859271017917181981E-14, -105.0863248654052313 ) ) ;
#23579 = CARTESIAN_POINT ( 'NONE',  ( -3.608439182435115633, 6.249999999999965361, -160.8080127018922667 ) ) ;
#23580 = CARTESIAN_POINT ( 'NONE',  ( -5.999999999999904965, -1.607695154586834541, -149.2693375672974128 ) ) ;
#23581 = ADVANCED_FACE ( 'NONE', ( #27387 ), #8358, .T. ) ;
#23582 = CARTESIAN_POINT ( 'NONE',  ( 6.350852961086080661, -9.614813431917819062E-14, -78.37500000000001421 ) ) ;
#23583 = CARTESIAN_POINT ( 'NONE',  ( 6.000000000000000888, 7.762456499804234384E-14, -132.6636751345948539 ) ) ;
#23584 = CARTESIAN_POINT ( 'NONE',  ( 3.175426480543072749, -5.500000000000105693, -65.12500000000001421 ) ) ;
#23585 = CIRCLE ( 'NONE', #9350, 30.00000000000000000 ) ;
#23586 = DIRECTION ( 'NONE',  ( 1.000000000000000000, 0.000000000000000000, 0.000000000000000000 ) ) ;
#23587 = CARTESIAN_POINT ( 'NONE',  ( 143.1711002691896795, 4.999999999999989342, 2.071067811865468400 ) ) ;
#23588 = CARTESIAN_POINT ( 'NONE',  ( 6.000000000000000000, 2.951592740943527306E-14, -148.5863248654052313 ) ) ;
#23589 = CARTESIAN_POINT ( 'NONE',  ( 158.5312500000000284, -2.485281374238556218, -6.000000000000005329 ) ) ;
#23590 = SURFACE_STYLE_USAGE ( .BOTH. , #25409 ) ;
#23591 = CARTESIAN_POINT ( 'NONE',  ( 17.56250000000009592, -1.999999999999851674, -0.8284271247461753029 ) ) ;
#23592 = LINE ( 'NONE', #11440, #2109 ) ;
#23593 = DIRECTION ( 'NONE',  ( -0.000000000000000000, -0.000000000000000000, -1.000000000000000000 ) ) ;
#23594 = CARTESIAN_POINT ( 'NONE',  ( 118.8122167782374987, 0.7662911109078287542, 1.849990392679712103 ) ) ;
#23595 = ADVANCED_FACE ( 'NONE', ( #27088 ), #26927, .T. ) ;
#23596 = LINE ( 'NONE', #2533, #19438 ) ;
#23597 = ORIENTED_EDGE ( 'NONE', *, *, #15662, .F. ) ;
#23598 = CARTESIAN_POINT ( 'NONE',  ( 148.8750000000000284, 0.000000000000000000, 6.000000000000005329 ) ) ;
#23599 = DIRECTION ( 'NONE',  ( 1.000000000000000000, 9.251858538542971828E-16, 0.000000000000000000 ) ) ;
#23600 = CARTESIAN_POINT ( 'NONE',  ( 114.3752832217622597, 1.849990392679551343, 0.000000000000000000 ) ) ;
#23601 = B_SPLINE_CURVE_WITH_KNOTS ( 'NONE', 3,
 ( #5397, #10493, #3236, #26885, #21855, #12815, #12973, #24438, #22308, #29349, #10647, #5845, #22158, #14948, #24148, #802 ),
 .UNSPECIFIED., .F., .F.,
 ( 4, 2, 2, 2, 2, 2, 2, 4 ),
 ( 0.000000000000000000, 0.0003858708990758222723, 0.0007717417981516445447, 0.001543483596303289089, 0.001929354495379140798, 0.002315225394454992723, 0.002701096293530844215, 0.003086967192606696140 ),
 .UNSPECIFIED. ) ;
#23602 = CARTESIAN_POINT ( 'NONE',  ( 140.0769230769231228, -11.53846153846155254, 4.615384615384604317 ) ) ;
#23603 = CARTESIAN_POINT ( 'NONE',  ( 21.87500000000011724, 1.414213562373201061, -1.414213562373090038 ) ) ;
#23604 = CARTESIAN_POINT ( 'NONE',  ( 5.412658773652712085, -3.125000000000086153, -154.5669872981078186 ) ) ;
#23605 = EDGE_LOOP ( 'NONE', ( #18135, #27445, #21294, #19616 ) ) ;
#23606 = CARTESIAN_POINT ( 'NONE',  ( 3.175426480543072749, 5.499999999999865885, -85.62500000000000000 ) ) ;
#23607 = TOROIDAL_SURFACE ( 'NONE', #24065, 28.99999999999999645, 1.000000000000000000 ) ;
#23608 = CARTESIAN_POINT ( 'NONE',  ( 16.12500000000005684, 1.665334536937734811E-13, -2.649519052838444910 ) ) ;
#23609 = CARTESIAN_POINT ( 'NONE',  ( 3.608439182435180470, -6.249999999999997335, -101.5580127018922383 ) ) ;
#23610 = ORIENTED_EDGE ( 'NONE', *, *, #17078, .T. ) ;
#23611 = VECTOR ( 'NONE', #22209, 1000.000000000000000 ) ;
#23612 = AXIS2_PLACEMENT_3D ( 'NONE', #28210, #18888, #408 ) ;
#23613 = CARTESIAN_POINT ( 'NONE',  ( 156.7351497308104058, 3.535533905932725318, -3.535533905932725318 ) ) ;
#23614 = CARTESIAN_POINT ( 'NONE',  ( -3.608439182435115633, 6.249999999999965361, -48.30801270189223828 ) ) ;
#23615 = VECTOR ( 'NONE', #18643, 1000.000000000000000 ) ;
#23616 = CARTESIAN_POINT ( 'NONE',  ( 6.350852961086080661, -9.614813431917819062E-14, -171.3750000000000000 ) ) ;
#23617 = CARTESIAN_POINT ( 'NONE',  ( 5.196152422706629359, 3.000000000000002665, -161.9613248654052597 ) ) ;
#23618 = CARTESIAN_POINT ( 'NONE',  ( -4.763139720814407951, 2.749999999999946709, -157.2500000000000000 ) ) ;
#23619 = CARTESIAN_POINT ( 'NONE',  ( 112.8749999999998437, 1.767766952966320915, -1.767766952966320915 ) ) ;
#23620 = EDGE_CURVE ( 'NONE', #6372, #12915, #1022, .T. ) ;
#23621 = CARTESIAN_POINT ( 'NONE',  ( 3.175426480543072749, 5.499999999999865885, -105.1250000000000284 ) ) ;
#23622 = CYLINDRICAL_SURFACE ( 'NONE', #1007, 1.000000000000000888 ) ;
#23623 = ADVANCED_FACE ( 'NONE', ( #22810 ), #4659, .T. ) ;
#23625 = CARTESIAN_POINT ( 'NONE',  ( 4.763139720814407951, 2.750000000000002665, -88.75000000000000000 ) ) ;
#23624 = CARTESIAN_POINT ( 'NONE',  ( -3.175426480542816510, -5.500000000000057732, -156.8750000000000284 ) ) ;
#23626 = PRODUCT_RELATED_PRODUCT_CATEGORY ( 'part', '', ( #6217 ) ) ;
#23627 = CARTESIAN_POINT ( 'NONE',  ( 156.8586002691896510, 2.071067811865468400, 4.999999999999989342 ) ) ;
#23628 = CARTESIAN_POINT ( 'NONE',  ( 106.7886751345947403, -1.999999999999946265, 0.000000000000000000 ) ) ;
#23629 = ORIENTED_EDGE ( 'NONE', *, *, #23986, .F. ) ;
#23630 = CARTESIAN_POINT ( 'NONE',  ( 111.6874999999997584, -1.035533905932719101, -2.499999999999844569 ) ) ;
#23631 = DIRECTION ( 'NONE',  ( -1.000000000000000000, 0.000000000000000000, 0.000000000000000000 ) ) ;
#23632 = CARTESIAN_POINT ( 'NONE',  ( 106.2502832217621460, 1.308140751793696044, -1.308140751793640533 ) ) ;
#23633 = DIRECTION ( 'NONE',  ( 5.551115123125785167E-17, -1.000000000000000000, -8.881784197001256268E-16 ) ) ;
#23634 = ORIENTED_EDGE ( 'NONE', *, *, #28272, .F. ) ;
#23635 = CARTESIAN_POINT ( 'NONE',  ( 0.000000000000000000, 0.000000000000000000, 0.000000000000000000 ) ) ;
#23636 = DIRECTION ( 'NONE',  ( -1.000000000000000000, -1.665334536937731113E-16, 1.526556658859586792E-16 ) ) ;
#23637 = CARTESIAN_POINT ( 'NONE',  ( 106.5622167782373708, 1.849990392679501827, -0.7662911109076485650 ) ) ;
#23638 = CIRCLE ( 'NONE', #21680, 0.5000000000000004441 ) ;
#23639 = EDGE_LOOP ( 'NONE', ( #20962, #20368, #10440, #27517 ) ) ;
#23640 = CARTESIAN_POINT ( 'NONE',  ( 5.196152422706629359, -2.999999999999988898, -52.71132486540519579 ) ) ;
#23641 = AXIS2_PLACEMENT_3D ( 'NONE', #25032, #8775, #4304 ) ;
#23642 = CARTESIAN_POINT ( 'NONE',  ( 151.3125000000000568, 4.242640687119298093, -4.242640687119298093 ) ) ;
#23643 = ORIENTED_EDGE ( 'NONE', *, *, #15265, .T. ) ;
#23644 = CARTESIAN_POINT ( 'NONE',  ( -2.775557561562891351E-14, -5.500000000000115463, -111.7500000000000142 ) ) ;
#23645 = CARTESIAN_POINT ( 'NONE',  ( 24.18750000000006395, 1.097466725451559322, -2.649519052838358757 ) ) ;
#23646 = CARTESIAN_POINT ( 'NONE',  ( -5.412658773652739619, 3.124999999999975131, -121.6830127018922525 ) ) ;
#23647 = ORIENTED_EDGE ( 'NONE', *, *, #12743, .F. ) ;
#23648 = CARTESIAN_POINT ( 'NONE',  ( -5.999999999999963585, 1.780251999655701777E-13, -56.91367513459483973 ) ) ;
#23649 = CARTESIAN_POINT ( 'NONE',  ( -5.412658773652739619, 3.124999999999975131, -170.3169872981078470 ) ) ;
#23650 = CARTESIAN_POINT ( 'NONE',  ( 109.8124999999997868, 1.035533905932779275, -2.499999999999784173 ) ) ;
#23651 = CARTESIAN_POINT ( 'NONE',  ( 133.3913997308104058, -2.071067811865468400, 4.999999999999989342 ) ) ;
#23652 = CIRCLE ( 'NONE', #5451, 2.499999999999998224 ) ;
#23653 = ORIENTED_EDGE ( 'NONE', *, *, #19259, .T. ) ;
#23654 = CARTESIAN_POINT ( 'NONE',  ( 153.1011751345948824, 3.889087296526011706, -3.889087296526011706 ) ) ;
#23655 = CARTESIAN_POINT ( 'NONE',  ( -3.175426480542816510, 5.499999999999865885, -176.8750000000000568 ) ) ;
#23656 = CARTESIAN_POINT ( 'NONE',  ( 109.5627832217622455, 0.7662911109077987781, 1.849990392679652151 ) ) ;
#23657 = CARTESIAN_POINT ( 'NONE',  ( 5.412658773652712085, -3.125000000000086153, -174.9330127018922099 ) ) ;
#23658 = CARTESIAN_POINT ( 'NONE',  ( 136.0000000000000284, -9.165151389911669000, 8.000000000000007105 ) ) ;
#23659 = CARTESIAN_POINT ( 'NONE',  ( 140.0000000000000284, -54.99999999999990763, 5.000000000000004441 ) ) ;
#23660 = CARTESIAN_POINT ( 'NONE',  ( 160.5767363903362082, -11.34513390049722936, -3.911391104096503479 ) ) ;
#23661 = EDGE_CURVE ( 'NONE', #452, #19300, #16387, .T. ) ;
#23662 = CARTESIAN_POINT ( 'NONE',  ( 4.763139720814407951, 2.750000000000002665, -115.7500000000000142 ) ) ;
#23663 = ORIENTED_EDGE ( 'NONE', *, *, #26401, .T. ) ;
#23664 = AXIS2_PLACEMENT_3D ( 'NONE', #15231, #24564, #3515 ) ;
#23665 = VECTOR ( 'NONE', #5893, 1000.000000000000000 ) ;
#23666 = DIRECTION ( 'NONE',  ( 0.000000000000000000, 0.000000000000000000, 1.000000000000000000 ) ) ;
#23667 = CARTESIAN_POINT ( 'NONE',  ( 6.000000000000000888, -3.330669073875464691E-16, -7.560779664488942560E-35 ) ) ;
#23668 = CARTESIAN_POINT ( 'NONE',  ( -5.999999999999963585, 8.134310703387671600E-14, -131.3363248654052313 ) ) ;
#23669 = VERTEX_POINT ( 'NONE', #13468 ) ;
#23670 =( LENGTH_UNIT ( ) NAMED_UNIT ( * ) SI_UNIT ( .MILLI., .METRE. ) );
#23671 = CARTESIAN_POINT ( 'NONE',  ( -6.350852961085760029, -1.281975124255709124E-13, -178.1250000000000284 ) ) ;
#23672 = DIRECTION ( 'NONE',  ( -0.000000000000000000, -0.000000000000000000, -1.000000000000000000 ) ) ;
#23673 = CARTESIAN_POINT ( 'NONE',  ( 156.8511751345948539, -3.889087296526011706, 3.889087296526011706 ) ) ;
#23674 =( BOUNDED_CURVE ( )  B_SPLINE_CURVE ( 2, ( #1646, #8410, #1795, #29747, #29283, #18111, #25130, #1489, #13517 ),
 .UNSPECIFIED., .F., .T. ) 
 B_SPLINE_CURVE_WITH_KNOTS ( ( 3, 2, 2, 2, 3 ),
 ( 0.8529411764705882026, 0.8602941176470588758, 0.8676470588235294379, 0.8750000000000000000, 0.8823529411764705621 ),
 .UNSPECIFIED. ) 
 CURVE ( )  GEOMETRIC_REPRESENTATION_ITEM ( )  RATIONAL_B_SPLINE_CURVE ( ( 1.000000000000000000, 0.9238795325112867385, 1.000000000000000000, 0.9238795325112867385, 1.000000000000000000, 0.9238795325112867385, 1.000000000000000000, 0.9238795325112867385, 1.000000000000000000 ) ) 
 REPRESENTATION_ITEM ( '' )  );
#23675 = CARTESIAN_POINT ( 'NONE',  ( 140.8988248654052029, 3.889087296526011706, 3.889087296526011706 ) ) ;
#23676 = ORIENTED_EDGE ( 'NONE', *, *, #21777, .F. ) ;
#23677 = ORIENTED_EDGE ( 'NONE', *, *, #1013, .T. ) ;
#23678 = CARTESIAN_POINT ( 'NONE',  ( 6.000000000000000888, -1.859271017917181981E-14, -141.6636751345948255 ) ) ;
#23679 = CARTESIAN_POINT ( 'NONE',  ( 138.1875000000000284, 4.242640687119269671, 4.242640687119298093 ) ) ;
#23680 = CARTESIAN_POINT ( 'NONE',  ( -5.412658773652684552, -3.125000000000099920, -138.5669872981077901 ) ) ;
#23681 = SURFACE_STYLE_USAGE ( .BOTH. , #14343 ) ;
#23682 = CARTESIAN_POINT ( 'NONE',  ( 11.68750000000011902, -1.097466725451379244, 2.649519052838238409 ) ) ;
#23683 = ADVANCED_FACE ( 'NONE', ( #25392 ), #23280, .F. ) ;
#23684 = CARTESIAN_POINT ( 'NONE',  ( 5.196152422706629359, 3.000000000000002665, -129.5386751345948255 ) ) ;
#23685 = CARTESIAN_POINT ( 'NONE',  ( 18.00000000000012790, 2.000000000000112799, 0.000000000000000000 ) ) ;
#23686 = CYLINDRICAL_SURFACE ( 'NONE', #21585, 6.000000000000000888 ) ;
#23687 = CARTESIAN_POINT ( 'NONE',  ( 117.5863248654050608, 1.414213562373090038, -1.414213562373034527 ) ) ;
#23688 = CYLINDRICAL_SURFACE ( 'NONE', #26468, 6.000000000000000888 ) ;
#23689 = CARTESIAN_POINT ( 'NONE',  ( 137.2351497308104058, 3.535533905932725318, -3.535533905932725318 ) ) ;
#23690 = CARTESIAN_POINT ( 'NONE',  ( 5.196152422706629359, 3.000000000000002665, -99.53867513459479710 ) ) ;
#23691 = CARTESIAN_POINT ( 'NONE',  ( 139.5000000000000000, -24.99999999999999289, -8.000000000000007105 ) ) ;
#23692 = CARTESIAN_POINT ( 'NONE',  ( 6.000000000000000888, -1.859271017917181981E-14, -147.0863248654052313 ) ) ;
#23693 = DIRECTION ( 'NONE',  ( -1.000000000000000000, -1.665334536937736783E-16, -2.220446049250315546E-16 ) ) ;
#23694 = CARTESIAN_POINT ( 'NONE',  ( -5.999999999999963585, 1.780251999655701777E-13, -69.83632486540523132 ) ) ;
#23695 = CARTESIAN_POINT ( 'NONE',  ( 106.9999999999999716, 2.500000000000030198, 0.000000000000000000 ) ) ;
#23696 = DIRECTION ( 'NONE',  ( -7.147005652999508048E-36, 5.642372883946980038E-36, 1.000000000000000000 ) ) ;
#23697 = EDGE_CURVE ( 'NONE', #29700, #7379, #7323, .T. ) ;
#23698 = CARTESIAN_POINT ( 'NONE',  ( 15.83632486540537165, 1.767766952966542959, 1.767766952966209892 ) ) ;
#23699 = CARTESIAN_POINT ( 'NONE',  ( 14.53867513459486460, 1.665334536937734811E-13, 2.499999999999835687 ) ) ;
#23700 = VERTEX_POINT ( 'NONE', #18374 ) ;
#23701 = CARTESIAN_POINT ( 'NONE',  ( 0.000000000000000000, 5.499999999999991118, -46.49999999999998579 ) ) ;
#23702 = CYLINDRICAL_SURFACE ( 'NONE', #22751, 2.499999999999999112 ) ;
#23703 = COLOUR_RGB ( '', 0.08235294, 0.09019608, 0.10196078) ;
#23704 = ORIENTED_EDGE ( 'NONE', *, *, #13066, .T. ) ;
#23705 = CARTESIAN_POINT ( 'NONE',  ( 116.6247167782376692, 1.849990392679523588, 0.000000000000000000 ) ) ;
#23706 = CARTESIAN_POINT ( 'NONE',  ( 139.9687500000000284, -2.485281374238585972, 6.000000000000005329 ) ) ;
#23707 = CARTESIAN_POINT ( 'NONE',  ( -7.216878364870328078, 0.000000000000000000, -104.1919872981078470 ) ) ;
#23708 = CARTESIAN_POINT ( 'NONE',  ( 138.0863248654052313, 0.000000000000000000, 5.500000000000005329 ) ) ;
#23709 = CARTESIAN_POINT ( 'NONE',  ( 159.3601497308104058, -3.535533905932725318, -3.535533905932725318 ) ) ;
#23710 = CARTESIAN_POINT ( 'NONE',  ( -3.175426480542816510, -5.500000000000057732, -126.8749999999999858 ) ) ;
#23711 = ORIENTED_EDGE ( 'NONE', *, *, #25651, .F. ) ;
#23712 = DIRECTION ( 'NONE',  ( 1.000000000000000000, -0.000000000000000000, -0.000000000000000000 ) ) ;
#23713 = EDGE_CURVE ( 'NONE', #12427, #12660, #17506, .T. ) ;
#23714 = CARTESIAN_POINT ( 'NONE',  ( -4.763139720814407951, -2.750000000000016431, -59.50000000000000000 ) ) ;
#23715 =( BOUNDED_CURVE ( )  B_SPLINE_CURVE ( 2, ( #11933, #18977, #18820, #9436, #5251, #2800, #2370, #14381, #4949 ),
 .UNSPECIFIED., .F., .F. ) 
 B_SPLINE_CURVE_WITH_KNOTS ( ( 3, 2, 2, 2, 3 ),
 ( 0.2352941176470587648, 0.2426470588235294379, 0.2500000000000000000, 0.2573529411764705621, 0.2647058823529411242 ),
 .UNSPECIFIED. ) 
 CURVE ( )  GEOMETRIC_REPRESENTATION_ITEM ( )  RATIONAL_B_SPLINE_CURVE ( ( 1.000000000000000000, 0.9238795325112867385, 1.000000000000000000, 0.9238795325112867385, 1.000000000000000000, 0.9238795325112867385, 1.000000000000000000, 0.9238795325112867385, 1.000000000000000000 ) ) 
 REPRESENTATION_ITEM ( '' )  );
#23716 = CARTESIAN_POINT ( 'NONE',  ( 0.000000000000000000, 0.000000000000000000, 0.000000000000000000 ) ) ;
#23717 = DIRECTION ( 'NONE',  ( -1.000000000000000000, -1.665334536937731113E-16, 1.526556658859586792E-16 ) ) ;
#23718 = CARTESIAN_POINT ( 'NONE',  ( 7.216878364870455975, -6.409875621278545621E-14, -83.30801270189226670 ) ) ;
#23719 = DIRECTION ( 'NONE',  ( 1.000000000000000000, -0.000000000000000000, 0.000000000000000000 ) ) ;
#23720 = CARTESIAN_POINT ( 'NONE',  ( 106.9997167782376550, -1.308140751793612777, 1.308140751793640533 ) ) ;
#23721 = CARTESIAN_POINT ( 'NONE',  ( 140.6451377260904678, -11.29027545218211515, -4.288736938852192537 ) ) ;
#23722 = CARTESIAN_POINT ( 'NONE',  ( 116.0000000000000142, 6.735557395310442023E-16, 5.500000000000000000 ) ) ;
#23723 = CARTESIAN_POINT ( 'NONE',  ( 113.5627832217622029, 0.7662911109078888172, 1.849990392679652151 ) ) ;
#23724 = EDGE_CURVE ( 'NONE', #30382, #25961, #21897, .T. ) ;
#23725 = ITEM_DEFINED_TRANSFORMATION ( 'NONE', 'NONE', #7044,  #18805 ) ;
#23726 = CARTESIAN_POINT ( 'NONE',  ( -4.763139720814407951, -2.750000000000016431, -140.5000000000000000 ) ) ;
#23727 = PLANE ( 'NONE',  #22665 ) ;
#23728 = CARTESIAN_POINT ( 'NONE',  ( -5.412658773652684552, -3.125000000000099920, -152.9330127018922383 ) ) ;
#23729 = CARTESIAN_POINT ( 'NONE',  ( 2.570750408560660700E-15, 10.49588505988223375, 2.088097429759527849E-50 ) ) ;
#23730 = CARTESIAN_POINT ( 'NONE',  ( -3.464101615137757051, -5.999999999999979572, -73.16367513459482552 ) ) ;
#23731 = CARTESIAN_POINT ( 'NONE',  ( -3.175426480542816066, -5.500000000000057732, -71.37499999999998579 ) ) ;
#23732 = CARTESIAN_POINT ( 'NONE',  ( -5.999999999999963585, -1.487416814333745711E-14, -113.9136751345948255 ) ) ;
#23733 = CARTESIAN_POINT ( 'NONE',  ( -1.110223024625164676E-16, 2.000000000000012879, 2.021286199229734960E-15 ) ) ;
#23734 = CARTESIAN_POINT ( 'NONE',  ( 4.763139720814407951, -2.749999999999988454, -65.00000000000000000 ) ) ;
#23735 = CARTESIAN_POINT ( 'NONE',  ( 145.4211002691896510, -4.999999999999989342, -2.071067811865468400 ) ) ;
#23736 = CARTESIAN_POINT ( 'NONE',  ( 6.000000000000000888, 7.762456499804234384E-14, -144.0863248654052313 ) ) ;
#23737 = PRESENTATION_LAYER_ASSIGNMENT (  '', '', ( #7531 ) ) ;
#23738 = CARTESIAN_POINT ( 'NONE',  ( 158.9062500000000284, 6.000000000000005329, -2.485281374238556218 ) ) ;
#23739 = CARTESIAN_POINT ( 'NONE',  ( 135.0000000000000284, -6.982120021884474781, -8.500000000000007105 ) ) ;
#23740 = CARTESIAN_POINT ( 'NONE',  ( 17.12500000000005684, 1.414213562373090038, 1.414213562373201061 ) ) ;
#23741 = SURFACE_STYLE_FILL_AREA ( #4676 ) ;
#23742 = DIRECTION ( 'NONE',  ( -8.326672684688675286E-17, -2.081668171172168821E-17, 1.000000000000000000 ) ) ;
#23743 = CARTESIAN_POINT ( 'NONE',  ( 115.4997167782375129, 1.308140751793640533, -1.308140751793640533 ) ) ;
#23744 = CARTESIAN_POINT ( 'NONE',  ( -5.196152422706573404, -3.000000000000002665, -145.2886751345948255 ) ) ;
#23745 = ORIENTED_EDGE ( 'NONE', *, *, #2849, .F. ) ;
#23746 = CARTESIAN_POINT ( 'NONE',  ( 150.2812500000000284, 2.485281374238585972, 6.000000000000005329 ) ) ;
#23747 = CARTESIAN_POINT ( 'NONE',  ( -5.999999999999919176, 1.607695154586804565, -63.90331216351301435 ) ) ;
#23748 = CARTESIAN_POINT ( 'NONE',  ( -2.775557561562891351E-14, -5.500000000000115463, -180.7500000000000284 ) ) ;
#23749 = CARTESIAN_POINT ( 'NONE',  ( 19.18750000000004263, 0.8284271247462955401, 2.000000000000031530 ) ) ;
#23750 = ORIENTED_EDGE ( 'NONE', *, *, #16432, .F. ) ;
#23751 = EDGE_CURVE ( 'NONE', #26686, #24771, #8650, .T. ) ;
#23752 = CARTESIAN_POINT ( 'NONE',  ( 3.175426480543072749, 5.499999999999865885, -87.12500000000000000 ) ) ;
#23753 =( BOUNDED_CURVE ( )  B_SPLINE_CURVE ( 2, ( #4354, #9129, #13467, #6512, #18521, #20497, #11004, #8832, #15784 ),
 .UNSPECIFIED., .F., .T. ) 
 B_SPLINE_CURVE_WITH_KNOTS ( ( 3, 2, 2, 2, 3 ),
 ( 0.2305555555555555691, 0.2314814814814814825, 0.2333333333333333370, 0.2351851851851851916, 0.2361111111111111049 ),
 .UNSPECIFIED. ) 
 CURVE ( )  GEOMETRIC_REPRESENTATION_ITEM ( )  RATIONAL_B_SPLINE_CURVE ( ( 0.9330127018922194093, 0.9330127018922204085, 1.000000000000000000, 0.8660254037844388186, 1.000000000000000000, 0.8660254037844388186, 1.000000000000000000, 0.9330127018922205195, 0.9330127018922196314 ) ) 
 REPRESENTATION_ITEM ( '' )  );
#23754 = CARTESIAN_POINT ( 'NONE',  ( 2.775557561562891351E-14, 6.250000000000033751, -100.9330127018922525 ) ) ;
#23755 = CYLINDRICAL_SURFACE ( 'NONE', #19179, 6.000000000000000888 ) ;
#23756 = CARTESIAN_POINT ( 'NONE',  ( 156.2663997308104342, -4.999999999999989342, -2.071067811865468400 ) ) ;
#23757 = CYLINDRICAL_SURFACE ( 'NONE', #25513, 9.999999999999980460 ) ;
#23758 = CARTESIAN_POINT ( 'NONE',  ( -5.999999999999963585, 1.780251999655701777E-13, -58.41367513459482552 ) ) ;
#23759 = FILL_AREA_STYLE ('',( #19596 ) ) ;
#23760 = EDGE_CURVE ( 'NONE', #2905, #2098, #13642, .T. ) ;
#23761 =( BOUNDED_CURVE ( )  B_SPLINE_CURVE ( 2, ( #18044, #15751, #2190, #18496, #1724, #29978, #11280, #1876, #25207 ),
 .UNSPECIFIED., .F., .T. ) 
 B_SPLINE_CURVE_WITH_KNOTS ( ( 3, 2, 2, 2, 3 ),
 ( 0.08823529411764707842, 0.09558823529411764053, 0.1029411764705882026, 0.1102941176470587648, 0.1176470588235294379 ),
 .UNSPECIFIED. ) 
 CURVE ( )  GEOMETRIC_REPRESENTATION_ITEM ( )  RATIONAL_B_SPLINE_CURVE ( ( 1.000000000000000000, 0.9238795325112867385, 1.000000000000000000, 0.9238795325112867385, 1.000000000000000000, 0.9238795325112867385, 1.000000000000000000, 0.9238795325112867385, 1.000000000000000000 ) ) 
 REPRESENTATION_ITEM ( '' )  );
#23762 = ADVANCED_FACE ( 'NONE', ( #15785 ), #23429, .T. ) ;
#23763 = CARTESIAN_POINT ( 'NONE',  ( -3.175426480542816066, 5.499999999999865885, -163.3750000000000568 ) ) ;
#23764 = CARTESIAN_POINT ( 'NONE',  ( -3.464101615137725076, 5.999999999999979572, -58.08632486540519579 ) ) ;
#23765 = CARTESIAN_POINT ( 'NONE',  ( 3.175426480543072749, 5.499999999999865885, -156.1250000000000000 ) ) ;
#23766 = CARTESIAN_POINT ( 'NONE',  ( 113.4999999999999147, -2.499999999999919176, 0.000000000000000000 ) ) ;
#23767 = CARTESIAN_POINT ( 'NONE',  ( -3.175426480542816510, -5.500000000000057732, -92.37500000000002842 ) ) ;
#23768 = CARTESIAN_POINT ( 'NONE',  ( 3.464101615137757051, -5.999999999999979572, -135.9136751345947971 ) ) ;
#23769 = CARTESIAN_POINT ( 'NONE',  ( 24.68750000000014566, -0.8284271247460552878, -2.000000000000151879 ) ) ;
#23770 = UNCERTAINTY_MEASURE_WITH_UNIT (LENGTH_MEASURE( 1.000000000000000082E-05 ), #25367, 'distance_accuracy_value', 'NONE');
#23771 = CARTESIAN_POINT ( 'NONE',  ( 114.6874999999997300, -1.035533905932689347, -2.499999999999784173 ) ) ;
#23772 = CARTESIAN_POINT ( 'NONE',  ( 3.464101615137852974, 5.999999999999884537, -126.4136751345948113 ) ) ;
#23773 = CARTESIAN_POINT ( 'NONE',  ( 10.00000000000014388, 2.023420126299062982, -0.3429612746322239780 ) ) ;
#23774 = DIRECTION ( 'NONE',  ( 1.000000000000000000, -5.551115123125773458E-17, -1.260129944081490338E-35 ) ) ;
#23775 = ORIENTED_EDGE ( 'NONE', *, *, #14701, .T. ) ;
#23776 = FILL_AREA_STYLE ('',( #19041 ) ) ;
#23777 = LINE ( 'NONE', #12138, #28004 ) ;
#23778 = CARTESIAN_POINT ( 'NONE',  ( 106.6247167782375840, 1.849990392679523588, 0.000000000000000000 ) ) ;
#23779 = ORIENTED_EDGE ( 'NONE', *, *, #12207, .T. ) ;
#23780 = CARTESIAN_POINT ( 'NONE',  ( 145.8750000000000284, 0.000000000000000000, 6.000000000000005329 ) ) ;
#23781 = EDGE_CURVE ( 'NONE', #25470, #22801, #19064, .T. ) ;
#23782 = CARTESIAN_POINT ( 'NONE',  ( -4.763139720814407951, 2.749999999999946709, -110.7500000000000142 ) ) ;
#23783 = CARTESIAN_POINT ( 'NONE',  ( 17.31250000000004263, 2.649519052838419153, -1.097466725451439196 ) ) ;
#23784 = CARTESIAN_POINT ( 'NONE',  ( -5.412658773652684552, -3.125000000000099920, -119.9330127018922667 ) ) ;
#23785 = UNCERTAINTY_MEASURE_WITH_UNIT (LENGTH_MEASURE( 1.000000000000000082E-05 ), #23670, 'distance_accuracy_value', 'NONE');
#23786 = VERTEX_POINT ( 'NONE', #15936 ) ;
#23787 = CARTESIAN_POINT ( 'NONE',  ( -5.412658773652739619, 3.124999999999975131, -162.8169872981078470 ) ) ;
#23788 = CARTESIAN_POINT ( 'NONE',  ( 108.5624999999997442, -2.499999999999934719, -1.035533905932568777 ) ) ;
#23789 = CARTESIAN_POINT ( 'NONE',  ( 132.6413997308104342, 2.071067811865468400, -4.999999999999989342 ) ) ;
#23790 = ORIENTED_EDGE ( 'NONE', *, *, #1889, .T. ) ;
#23791 = EDGE_CURVE ( 'NONE', #12642, #20769, #3307, .T. ) ;
#23792 = CARTESIAN_POINT ( 'NONE',  ( 6.000000000000000888, 1.743066579297358182E-13, -96.66367513459479710 ) ) ;
#23793 = DIRECTION ( 'NONE',  ( 1.000000000000000000, -5.551115123125773458E-17, -1.260129944081490338E-35 ) ) ;
#23794 = CARTESIAN_POINT ( 'NONE',  ( -3.175426480542816510, -5.500000000000057732, -177.8750000000000568 ) ) ;
#23795 = CARTESIAN_POINT ( 'NONE',  ( 106.0627832217622455, -0.7662911109077388261, -1.849990392679351725 ) ) ;
#23796 = DIRECTION ( 'NONE',  ( 1.000000000000000000, 0.000000000000000000, -0.000000000000000000 ) ) ;
#23797 = CARTESIAN_POINT ( 'NONE',  ( -3.608439182435052128, -6.250000000000110134, -175.3080127018922667 ) ) ;
#23798 = CARTESIAN_POINT ( 'NONE',  ( 119.4136751345947403, 1.414213562373117794, 1.414213562373034527 ) ) ;
#23799 = DIRECTION ( 'NONE',  ( 0.000000000000000000, 0.000000000000000000, -1.000000000000000000 ) ) ;
#23800 = CARTESIAN_POINT ( 'NONE',  ( -4.763139720814407951, -2.750000000000016431, -124.0000000000000000 ) ) ;
#23801 = CARTESIAN_POINT ( 'NONE',  ( 136.0000000000000284, -8.798545334315205579, 8.160000000000000142 ) ) ;
#23802 = UNCERTAINTY_MEASURE_WITH_UNIT (LENGTH_MEASURE( 1.000000000000000082E-05 ), #29198, 'distance_accuracy_value', 'NONE');
#23803 = CARTESIAN_POINT ( 'NONE',  ( 3.175426480543072749, 5.499999999999865885, -117.1250000000000142 ) ) ;
#23804 = CARTESIAN_POINT ( 'NONE',  ( -6.000000000000000888, 1.067854986875958443E-15, 7.560779664488942560E-35 ) ) ;
#23805 = CARTESIAN_POINT ( 'NONE',  ( 6.000000000000000888, -1.859271017917181981E-14, -131.1636751345948539 ) ) ;
#23806 = VERTEX_POINT ( 'NONE', #21118 ) ;
#23807 = CARTESIAN_POINT ( 'NONE',  ( 18.87500000000014211, 1.110223024625156540E-13, 2.649519052838056332 ) ) ;
#23808 = DIRECTION ( 'NONE',  ( -7.147005652999508048E-36, 5.642372883946980038E-36, 1.000000000000000000 ) ) ;
#23809 = CARTESIAN_POINT ( 'NONE',  ( 5.196152422706629359, -2.999999999999988898, -55.71132486540519579 ) ) ;
#23810 = VERTEX_POINT ( 'NONE', #18218 ) ;
#23811 = AXIS2_PLACEMENT_3D ( 'NONE', #27393, #11161, #22977 ) ;
#23812 = CARTESIAN_POINT ( 'NONE',  ( 111.5386751345947403, 5.551115123125782702E-14, 2.000000000000001776 ) ) ;
#23813 = CARTESIAN_POINT ( 'NONE',  ( -6.350852961085760029, -1.281975124255709124E-13, -176.6250000000000284 ) ) ;
#23814 = CARTESIAN_POINT ( 'NONE',  ( 22.96132486540528106, 1.665334536937734811E-13, 2.499999999999946709 ) ) ;
#23815 = ORIENTED_EDGE ( 'NONE', *, *, #27603, .T. ) ;
#23816 = CARTESIAN_POINT ( 'NONE',  ( -6.000000000000007105, -1.607695154586655129, -77.84668783648702117 ) ) ;
#23817 = ORIENTED_EDGE ( 'NONE', *, *, #20072, .F. ) ;
#23818 = EDGE_LOOP ( 'NONE', ( #19870, #29958, #26688, #5 ) ) ;
#23819 = CARTESIAN_POINT ( 'NONE',  ( -5.999999999999963585, -2.788906526875773208E-15, -176.3363248654052029 ) ) ;
#23820 = CARTESIAN_POINT ( 'NONE',  ( 133.8898502691896510, 3.535533905932725318, -3.535533905932725318 ) ) ;
#23821 = ADVANCED_FACE ( 'NONE', ( #18675 ), #16784, .F. ) ;
#23822 = AXIS2_PLACEMENT_3D ( 'NONE', #30225, #23342, #16450 ) ;
#23823 = EDGE_CURVE ( 'NONE', #8771, #1653, #14665, .T. ) ;
#23824 = ORIENTED_EDGE ( 'NONE', *, *, #22385, .T. ) ;
#23825 = CARTESIAN_POINT ( 'NONE',  ( -3.608439182435115633, 6.249999999999965361, -138.9419872981077901 ) ) ;
#23826 = SURFACE_STYLE_USAGE ( .BOTH. , #12485 ) ;
#23827 = CARTESIAN_POINT ( 'NONE',  ( -3.464101615137725076, 5.999999999999979572, -175.0863248654052029 ) ) ;
#23828 = CARTESIAN_POINT ( 'NONE',  ( 19.39882486540527040, -1.035533905932568999, -2.499999999999904521 ) ) ;
#23829 = EDGE_LOOP ( 'NONE', ( #8653, #10828, #9570, #26109 ) ) ;
#23830 = CARTESIAN_POINT ( 'NONE',  ( 20.06250000000006395, 2.000000000000151879, 0.8284271247461753029 ) ) ;
#23831 = CARTESIAN_POINT ( 'NONE',  ( 0.000000000000000000, -5.999999999999991118, -130.0386751345948824 ) ) ;
#23832 = LINE ( 'NONE', #29009, #10797 ) ;
#23833 = CARTESIAN_POINT ( 'NONE',  ( -2.000000000000000000, 3.559516622919861969E-16, -185.0000000000000000 ) ) ;
#23834 = CARTESIAN_POINT ( 'NONE',  ( 140.6101497308104058, 3.535533905932725318, 3.535533905932725318 ) ) ;
#23835 = CARTESIAN_POINT ( 'NONE',  ( -5.999999999999919176, 1.607695154586804565, -98.98066243270261566 ) ) ;
#23836 = CARTESIAN_POINT ( 'NONE',  ( 11.96132486540524198, 1.110223024625156540E-13, 2.499999999999835687 ) ) ;
#23837 = CARTESIAN_POINT ( 'NONE',  ( 6.000000000000000888, 1.607695154586715303, -147.0193375672974696 ) ) ;
#23838 = AXIS2_PLACEMENT_3D ( 'NONE', #25108, #3909, #24955 ) ;
#23839 = DIRECTION ( 'NONE',  ( 1.387778780781444256E-14, 1.000000000000000000, -0.000000000000000000 ) ) ;
#23840 = CARTESIAN_POINT ( 'NONE',  ( -3.464101615137725076, 5.999999999999979572, -113.5863248654051887 ) ) ;
#23841 = CARTESIAN_POINT ( 'NONE',  ( 106.2499999999999716, -2.775557561562891351E-14, 2.499999999999946709 ) ) ;
#23842 = VERTEX_POINT ( 'NONE', #16977 ) ;
#23843 = DIRECTION ( 'NONE',  ( -7.147005652999508048E-36, 5.642372883946980038E-36, 1.000000000000000000 ) ) ;
#23844 = CARTESIAN_POINT ( 'NONE',  ( -3.464101615137725076, 5.999999999999979572, -62.58632486540521711 ) ) ;
#23845 =( BOUNDED_CURVE ( )  B_SPLINE_CURVE ( 2, ( #7848, #19991, #26723, #5687, #24586, #21995, #29343, #28883, #29183 ),
 .UNSPECIFIED., .F., .T. ) 
 B_SPLINE_CURVE_WITH_KNOTS ( ( 3, 2, 2, 2, 3 ),
 ( 0.7624999999999992895, 0.7687499999999996003, 0.7749999999999998002, 0.7812500000000000000, 0.7875000000000001998 ),
 .UNSPECIFIED. ) 
 CURVE ( )  GEOMETRIC_REPRESENTATION_ITEM ( )  RATIONAL_B_SPLINE_CURVE ( ( 1.000000000000008216, 0.9238795325112786339, 1.000000000000000000, 0.9238795325112867385, 1.000000000000000000, 0.9238795325112867385, 1.000000000000000000, 0.9238795325112840739, 1.000000000000002665 ) ) 
 REPRESENTATION_ITEM ( '' )  );
#23846 = ORIENTED_EDGE ( 'NONE', *, *, #5928, .T. ) ;
#23847 = CARTESIAN_POINT ( 'NONE',  ( 115.8122167782375982, 0.7662911109078588412, 1.849990392679712103 ) ) ;
#23848 = CARTESIAN_POINT ( 'NONE',  ( 24.99999999999999289, 1.110223024625156540E-13, -2.220446049250313081E-13 ) ) ;
#23849 = VECTOR ( 'NONE', #1163, 1000.000000000000000 ) ;
#23850 = CARTESIAN_POINT ( 'NONE',  ( -5.412658773652684552, -3.125000000000099920, -105.5669872981078186 ) ) ;
#23851 = CARTESIAN_POINT ( 'NONE',  ( 133.2187500000000568, 2.485281374238555774, -6.000000000000005329 ) ) ;
#23852 = CARTESIAN_POINT ( 'NONE',  ( 117.9374999999998721, 2.500000000000115019, -1.035533905932448873 ) ) ;
#23853 = AXIS2_PLACEMENT_3D ( 'NONE', #20794, #30141, #2349 ) ;
#23854 = CARTESIAN_POINT ( 'NONE',  ( 0.000000000000000000, 5.499999999999991118, -129.0000000000000000 ) ) ;
#23855 = EDGE_CURVE ( 'NONE', #27302, #22419, #2806, .T. ) ;
#23856 = ORIENTED_EDGE ( 'NONE', *, *, #23880, .T. ) ;
#23857 = ORIENTED_EDGE ( 'NONE', *, *, #21685, .F. ) ;
#23858 = SURFACE_STYLE_FILL_AREA ( #12224 ) ;
#23859 = CARTESIAN_POINT ( 'NONE',  ( 4.763139720814407951, -2.749999999999988454, -54.49999999999999289 ) ) ;
#23860 = CARTESIAN_POINT ( 'NONE',  ( -5.999999999999963585, 0.000000000000000000, -179.9136751345948255 ) ) ;
#23861 = DIRECTION ( 'NONE',  ( 0.000000000000000000, 0.000000000000000000, -1.000000000000000000 ) ) ;
#23862 = CARTESIAN_POINT ( 'NONE',  ( -5.412658773652684552, -3.125000000000099920, -80.93301270189223828 ) ) ;
#23863 = PRODUCT_DEFINITION_CONTEXT ( 'detailed design', #9497, 'design' ) ;
#23864 = CARTESIAN_POINT ( 'NONE',  ( 5.196152422706629359, 3.000000000000002665, -149.9613248654052597 ) ) ;
#23865 = CARTESIAN_POINT ( 'NONE',  ( 107.7497167782375982, 1.308140751793668288, 1.308140751793640533 ) ) ;
#23866 = CARTESIAN_POINT ( 'NONE',  ( 116.5627832217621034, 0.7662911109078888172, 1.849990392679652151 ) ) ;
#23867 = CARTESIAN_POINT ( 'NONE',  ( -3.175426480542816066, 5.499999999999865885, -139.3750000000000568 ) ) ;
#23868 = DIRECTION ( 'NONE',  ( 1.000000000000000000, -3.469446951953694061E-16, 0.000000000000000000 ) ) ;
#23869 = CARTESIAN_POINT ( 'NONE',  ( -3.608439182435115633, 6.249999999999965361, -150.3080127018922099 ) ) ;
#23870 = CARTESIAN_POINT ( 'NONE',  ( 5.196152422706629359, -2.999999999999988898, -70.71132486540521711 ) ) ;
#23871 = CARTESIAN_POINT ( 'NONE',  ( 15.00000000000000000, 0.000000000000000000, 0.000000000000000000 ) ) ;
#23872 = CARTESIAN_POINT ( 'NONE',  ( -3.175426480542816066, 5.499999999999865885, -70.37500000000004263 ) ) ;
#23873 = CARTESIAN_POINT ( 'NONE',  ( 0.000000000000000000, 5.499999999999991118, -64.50000000000000000 ) ) ;
#23874 = CARTESIAN_POINT ( 'NONE',  ( 15.00000000000000000, 0.000000000000000000, 0.000000000000000000 ) ) ;
#23875 = CARTESIAN_POINT ( 'NONE',  ( 143.5461002691896510, -2.071067811865468400, 4.999999999999989342 ) ) ;
#23876 = CARTESIAN_POINT ( 'NONE',  ( 0.7669223171414760731, -15.58766199952932396, 7.954545454545463912 ) ) ;
#23877 = CARTESIAN_POINT ( 'NONE',  ( 152.1562500000000284, -6.000000000000005329, 2.485281374238556218 ) ) ;
#23878 = CYLINDRICAL_SURFACE ( 'NONE', #1583, 2.499999999999999112 ) ;
#23879 = CARTESIAN_POINT ( 'NONE',  ( 17.62500000000008527, -1.414213562372923505, -1.414213562373145550 ) ) ;
#23880 = EDGE_CURVE ( 'NONE', #5354, #28619, #17913, .T. ) ;
#23881 = AXIS2_PLACEMENT_3D ( 'NONE', #4025, #6494, #22945 ) ;
#23882 = CARTESIAN_POINT ( 'NONE',  ( 6.000000000000000888, 7.762456499804234384E-14, -144.6636751345948255 ) ) ;
#23883 = VERTEX_POINT ( 'NONE', #19271 ) ;
#23884 = CARTESIAN_POINT ( 'NONE',  ( 151.9687500000000568, -2.485281374238585972, 6.000000000000005329 ) ) ;
#23885 = DIRECTION ( 'NONE',  ( 0.000000000000000000, -1.000000000000000000, -8.881784197001264156E-16 ) ) ;
#23886 = TOROIDAL_SURFACE ( 'NONE', #14589, 2.000000000000000000, 1.000000000000000000 ) ;
#23887 = UNCERTAINTY_MEASURE_WITH_UNIT (LENGTH_MEASURE( 1.000000000000000082E-05 ), #3816, 'distance_accuracy_value', 'NONE');
#23888 = CARTESIAN_POINT ( 'NONE',  ( 3.464101615137757051, -5.999999999999979572, -102.3363248654052171 ) ) ;
#23889 = ADVANCED_FACE ( 'NONE', ( #14388 ), #10198, .F. ) ;
#23890 = CARTESIAN_POINT ( 'NONE',  ( -3.175426480542816510, 5.499999999999865885, -178.3750000000000568 ) ) ;
#23891 = CARTESIAN_POINT ( 'NONE',  ( 23.12500000000003553, 1.414213562373090038, 1.414213562373034527 ) ) ;
#23892 = ORIENTED_EDGE ( 'NONE', *, *, #4341, .T. ) ;
#23893 = CARTESIAN_POINT ( 'NONE',  ( 7.216878364870455975, -6.409875621278545621E-14, -155.9419872981078470 ) ) ;
#23894 = VERTEX_POINT ( 'NONE', #16539 ) ;
#23895 = CARTESIAN_POINT ( 'NONE',  ( -6.350852961085760029, -1.281975124255709124E-13, -83.62499999999998579 ) ) ;
#23896 = CARTESIAN_POINT ( 'NONE',  ( -7.216878364870328078, 0.000000000000000000, -99.05801270189222407 ) ) ;
#23897 = ORIENTED_EDGE ( 'NONE', *, *, #7417, .T. ) ;
#23898 = VECTOR ( 'NONE', #11932, 1000.000000000000000 ) ;
#23899 = DIRECTION ( 'NONE',  ( -7.147005652999508048E-36, 5.642372883946980038E-36, 1.000000000000000000 ) ) ;
#23900 = CARTESIAN_POINT ( 'NONE',  ( 5.950275682033426605, -9.251745015924175419, -24.20335556275641054 ) ) ;
#23901 = CARTESIAN_POINT ( 'NONE',  ( 140.0707155294784911, -11.09459640813488690, 4.575173035329051174 ) ) ;
#23902 = AXIS2_PLACEMENT_3D ( 'NONE', #7300, #21138, #23300 ) ;
#23903 = AXIS2_PLACEMENT_3D ( 'NONE', #6451, #23521, #16182 ) ;
#23904 = CARTESIAN_POINT ( 'NONE',  ( 4.763139720814407951, 2.750000000000002665, -163.7500000000000000 ) ) ;
#23905 = CARTESIAN_POINT ( 'NONE',  ( 143.6175748654052597, 5.500000000000012434, -2.278174593052012309 ) ) ;
#23906 = CARTESIAN_POINT ( 'NONE',  ( 0.000000000000000000, 5.499999999999991118, -154.5000000000000284 ) ) ;
#23907 = CARTESIAN_POINT ( 'NONE',  ( 0.000000000000000000, 5.999999999999977796, -76.78867513459481131 ) ) ;
#23908 = CARTESIAN_POINT ( 'NONE',  ( 148.7738248654052597, -3.889087296526011706, 3.889087296526011706 ) ) ;
#23909 = CARTESIAN_POINT ( 'NONE',  ( -3.175426480542816066, 5.499999999999865885, -91.37500000000001421 ) ) ;
#23910 = DIRECTION ( 'NONE',  ( 0.000000000000000000, 0.000000000000000000, -1.000000000000000000 ) ) ;
#23911 = CARTESIAN_POINT ( 'NONE',  ( 104.5938208054404299, -2.337497598169785640, 2.220446049250313081E-13 ) ) ;
#23912 = CARTESIAN_POINT ( 'NONE',  ( -2.775557561562891351E-14, -5.500000000000115463, -86.25000000000004263 ) ) ;
#23913 = CARTESIAN_POINT ( 'NONE',  ( 157.5148502691896510, -3.535533905932725318, -3.535533905932725318 ) ) ;
#23914 = CARTESIAN_POINT ( 'NONE',  ( 119.9999999999997868, 6.000000000000152767, 2.049675791781414311E-14 ) ) ;
#23915 = AXIS2_PLACEMENT_3D ( 'NONE', #29996, #27982, #1737 ) ;
#23916 = CARTESIAN_POINT ( 'NONE',  ( 24.06250000000009592, 2.000000000000091926, 0.8284271247461152399 ) ) ;
#23917 = CARTESIAN_POINT ( 'NONE',  ( 113.1874999999998295, 1.035533905932779275, 2.500000000000205169 ) ) ;
#23918 = EDGE_CURVE ( 'NONE', #29310, #8028, #27001, .T. ) ;
#23919 = CARTESIAN_POINT ( 'NONE',  ( 3.464101615137757051, -5.999999999999979572, -66.33632486540516027 ) ) ;
#23920 = CYLINDRICAL_SURFACE ( 'NONE', #27705, 6.000000000000000888 ) ;
#23921 = ORIENTED_EDGE ( 'NONE', *, *, #3502, .F. ) ;
#23922 =( LENGTH_UNIT ( ) NAMED_UNIT ( * ) SI_UNIT ( .MILLI., .METRE. ) );
#23923 = CYLINDRICAL_SURFACE ( 'NONE', #536, 6.000000000000000888 ) ;
#23924 = CARTESIAN_POINT ( 'NONE',  ( 119.4377832217620607, 1.849990392679591977, 0.7662911109080692285 ) ) ;
#23925 = VERTEX_POINT ( 'NONE', #9743 ) ;
#23926 = COLOUR_RGB ( '', 0.40784314, 0.44705882, 0.49803922) ;
#23927 = EDGE_CURVE ( 'NONE', #6918, #17372, #9729, .T. ) ;
#23928 =( BOUNDED_CURVE ( )  B_SPLINE_CURVE ( 2, ( #25918, #16596, #4866, #14296, #27189, #25774, #13269, #1702, #11099 ),
 .UNSPECIFIED., .F., .T. ) 
 B_SPLINE_CURVE_WITH_KNOTS ( ( 3, 2, 2, 2, 3 ),
 ( 0.5781250000000000000, 0.5859375000000000000, 0.5937500000000000000, 0.6015625000000000000, 0.6093750000000000000 ),
 .UNSPECIFIED. ) 
 CURVE ( )  GEOMETRIC_REPRESENTATION_ITEM ( )  RATIONAL_B_SPLINE_CURVE ( ( 1.000000000000000000, 0.9238795325112867385, 1.000000000000000000, 0.9238795325112867385, 1.000000000000000000, 0.9238795325112867385, 1.000000000000000000, 0.9238795325112867385, 1.000000000000000000 ) ) 
 REPRESENTATION_ITEM ( '' )  );
#23929 = ADVANCED_FACE ( 'NONE', ( #20008 ), #3553, .T. ) ;
#23930 = VERTEX_POINT ( 'NONE', #15115 ) ;
#23931 = VERTEX_POINT ( 'NONE', #10347 ) ;
#23932 = CARTESIAN_POINT ( 'NONE',  ( -2.775557561562891351E-14, -5.500000000000115463, -108.7500000000000142 ) ) ;
#23933 = CARTESIAN_POINT ( 'NONE',  ( 18.50000000000012790, 1.873492889145011997, 1.873492889144845464 ) ) ;
#23934 = CARTESIAN_POINT ( 'NONE',  ( 4.763139720814407951, -2.749999999999988454, -150.5000000000000284 ) ) ;
#23935 = CARTESIAN_POINT ( 'NONE',  ( 5.412658773652712085, -3.125000000000086153, -122.4330127018922241 ) ) ;
#23936 = ORIENTED_EDGE ( 'NONE', *, *, #22351, .F. ) ;
#23937 = CARTESIAN_POINT ( 'NONE',  ( -5.999999999999963585, 1.780251999655701777E-13, -110.9136751345948255 ) ) ;
#23938 = CARTESIAN_POINT ( 'NONE',  ( 2.775557561562891351E-14, 6.250000000000033751, -164.5669872981078186 ) ) ;
#23939 = CARTESIAN_POINT ( 'NONE',  ( 108.8124999999997442, 1.035533905932839449, -2.499999999999964473 ) ) ;
#23940 = VECTOR ( 'NONE', #10954, 1000.000000000000000 ) ;
#23941 = CARTESIAN_POINT ( 'NONE',  ( 134.3288997308104058, 4.999999999999989342, -2.071067811865468400 ) ) ;
#23942 = CARTESIAN_POINT ( 'NONE',  ( 2.775557561562891351E-14, 6.250000000000033751, -57.43301270189227381 ) ) ;
#23943 = ORIENTED_EDGE ( 'NONE', *, *, #23918, .T. ) ;
#23944 = CARTESIAN_POINT ( 'NONE',  ( 6.000000000000000888, 1.607695154586715303, -168.0193375672974128 ) ) ;
#23945 = CARTESIAN_POINT ( 'NONE',  ( 124.9999999999999432, -69.50000000000000000, -7.500000000000007105 ) ) ;
#23946 = FILL_AREA_STYLE ('',( #25936 ) ) ;
#23947 = CARTESIAN_POINT ( 'NONE',  ( 4.763139720814407951, 2.750000000000002665, -178.7500000000000284 ) ) ;
#23948 = CARTESIAN_POINT ( 'NONE',  ( 108.2502832217622029, 1.308140751793640533, -1.308140751793640533 ) ) ;
#23949 = CARTESIAN_POINT ( 'NONE',  ( -3.464101615137757051, -5.999999999999979572, -169.1636751345948255 ) ) ;
#23950 = CARTESIAN_POINT ( 'NONE',  ( 3.608439182435180470, 6.249999999999982236, -179.0580127018922667 ) ) ;
#23951 = CARTESIAN_POINT ( 'NONE',  ( 113.4136751345947260, 1.414213562373117794, 1.414213562373034527 ) ) ;
#23952 = CARTESIAN_POINT ( 'NONE',  ( -3.464101615137757051, -5.999999999999979572, -48.58632486540521711 ) ) ;
#23953 = CARTESIAN_POINT ( 'NONE',  ( 6.350852961086080661, -9.614813431917819062E-14, -114.3750000000000000 ) ) ;
#23954 = CARTESIAN_POINT ( 'NONE',  ( 3.464101615137852974, 5.999999999999884537, -84.41367513459481131 ) ) ;
#23955 = CARTESIAN_POINT ( 'NONE',  ( 0.000000000000000000, 5.499999999999991118, -109.5000000000000426 ) ) ;
#23956 = DIRECTION ( 'NONE',  ( 0.000000000000000000, 0.000000000000000000, -1.000000000000000000 ) ) ;
#23957 = ORIENTED_EDGE ( 'NONE', *, *, #29482, .T. ) ;
#23958 = CARTESIAN_POINT ( 'NONE',  ( 18.56250000000011013, 2.649519052838358757, -1.097466725451559322 ) ) ;
#23959 = CARTESIAN_POINT ( 'NONE',  ( 2.775557561562891351E-14, 20.00000000000001776, -25.00000000000002132 ) ) ;
#23960 = ADVANCED_FACE ( 'NONE', ( #10976 ), #1414, .F. ) ;
#23961 = CYLINDRICAL_SURFACE ( 'NONE', #28290, 6.000000000000000888 ) ;
#23962 = CARTESIAN_POINT ( 'NONE',  ( 5.999999999999949374, -1.607695154586841868, -145.6533121635130499 ) ) ;
#23963 = ORIENTED_EDGE ( 'NONE', *, *, #28989, .T. ) ;
#23964 = DIRECTION ( 'NONE',  ( 1.000000000000000000, 0.000000000000000000, 0.000000000000000000 ) ) ;
#23965 = VERTEX_POINT ( 'NONE', #15275 ) ;
#23966 = ADVANCED_FACE ( 'NONE', ( #24448 ), #5706, .T. ) ;
#23967 = LINE ( 'NONE', #28691, #767 ) ;
#23968 = VERTEX_POINT ( 'NONE', #17578 ) ;
#23969 = VERTEX_POINT ( 'NONE', #22168 ) ;
#23970 = CARTESIAN_POINT ( 'NONE',  ( 132.6562500000000284, -6.000000000000005329, 2.485281374238555774 ) ) ;
#23971 = CARTESIAN_POINT ( 'NONE',  ( 160.8750000000000568, 0.000000000000000000, 6.000000000000005329 ) ) ;
#23972 = ORIENTED_EDGE ( 'NONE', *, *, #26161, .F. ) ;
#23973 = CARTESIAN_POINT ( 'NONE',  ( 3.608439182435180470, -6.249999999999997335, -127.6919872981078328 ) ) ;
#23974 = CARTESIAN_POINT ( 'NONE',  ( 11.25000000000009237, 1.873492889145011997, -1.873492889144956486 ) ) ;
#23975 = CARTESIAN_POINT ( 'NONE',  ( 19.81250000000009237, 0.8284271247463557142, -2.000000000000091926 ) ) ;
#23976 = CARTESIAN_POINT ( 'NONE',  ( 6.000000000000000888, 7.762456499804234384E-14, -129.6636751345948255 ) ) ;
#23977 = CARTESIAN_POINT ( 'NONE',  ( 6.000000000000000888, -3.330669073875464691E-16, -7.560779664488942560E-35 ) ) ;
#23978 = CARTESIAN_POINT ( 'NONE',  ( 135.2663997308104342, -4.999999999999989342, -2.071067811865468400 ) ) ;
#23979 = FACE_OUTER_BOUND ( 'NONE', #2213, .T. ) ;
#23980 = SURFACE_STYLE_USAGE ( .BOTH. , #16655 ) ;
#23981 = DIRECTION ( 'NONE',  ( 1.000000000000000000, -5.551115123125773458E-17, -1.260129944081490338E-35 ) ) ;
#23982 = CARTESIAN_POINT ( 'NONE',  ( 105.3124999999998437, -1.035533905932598975, 2.500000000000265121 ) ) ;
#23983 = CARTESIAN_POINT ( 'NONE',  ( -6.350852961085760029, -1.281975124255709124E-13, -137.6250000000000568 ) ) ;
#23984 = CARTESIAN_POINT ( 'NONE',  ( 0.9568781502952149465, -15.26121788209296959, -8.567725837855926230 ) ) ;
#23985 = ORIENTED_EDGE ( 'NONE', *, *, #3829, .T. ) ;
#23986 = EDGE_CURVE ( 'NONE', #10258, #124, #6183, .T. ) ;
#23987 = CARTESIAN_POINT ( 'NONE',  ( 107.9761751345945839, -0.8284271247461453269, -1.999999999999791278 ) ) ;
#23988 = CARTESIAN_POINT ( 'NONE',  ( 118.0386751345946976, 8.326672684688674053E-14, -2.000000000000001776 ) ) ;
#23989 = ADVANCED_FACE ( 'NONE', ( #26894 ), #15438, .F. ) ;
#23990 = VECTOR ( 'NONE', #2162, 1000.000000000000000 ) ;
#23991 = ORIENTED_EDGE ( 'NONE', *, *, #933, .T. ) ;
#23992 = CARTESIAN_POINT ( 'NONE',  ( 118.2497167782374419, -1.308140751793585022, -1.308140751793640533 ) ) ;
#23993 = CARTESIAN_POINT ( 'NONE',  ( 136.1250000000000284, 0.000000000000000000, -6.000000000000005329 ) ) ;
#23994 = CARTESIAN_POINT ( 'NONE',  ( -3.608439182435115633, 6.249999999999965361, -98.44198729810783277 ) ) ;
#23995 = DIRECTION ( 'NONE',  ( 1.000000000000000000, 0.000000000000000000, 0.000000000000000000 ) ) ;
#23996 = CARTESIAN_POINT ( 'NONE',  ( 11.08632486540533968, -1.767766952966265404, 1.767766952966376426 ) ) ;
#23997 = CARTESIAN_POINT ( 'NONE',  ( 118.1874999999997300, 1.035533905932719101, 2.500000000000205169 ) ) ;
#23998 = CARTESIAN_POINT ( 'NONE',  ( -1.000000000000000888, 11.00000000000001066, 4.000000000000003553 ) ) ;
#23999 = CARTESIAN_POINT ( 'NONE',  ( 4.763139720814407951, 2.750000000000002665, -126.2500000000000284 ) ) ;
#24000 = ORIENTED_EDGE ( 'NONE', *, *, #4595, .T. ) ;
#24001 = FILL_AREA_STYLE_COLOUR ( '', #10659 ) ;
#24002 = CARTESIAN_POINT ( 'NONE',  ( -3.175426480542816510, 5.499999999999865885, -61.37500000000000000 ) ) ;
#24003 = CARTESIAN_POINT ( 'NONE',  ( 6.000000000000000888, 1.607695154586715303, -116.0966878364870496 ) ) ;
#24004 = CARTESIAN_POINT ( 'NONE',  ( 159.2870157019986550, -12.02748541700689522, -3.967488760539278125 ) ) ;
#24005 = CARTESIAN_POINT ( 'NONE',  ( 5.196552517144625405, 9.698180938751583824, -21.97571210926420093 ) ) ;
#24006 =( BOUNDED_CURVE ( )  B_SPLINE_CURVE ( 2, ( #15908, #28119, #11743, #23396, #21087, #7090, #2034, #9406, #4168 ),
 .UNSPECIFIED., .F., .F. ) 
 B_SPLINE_CURVE_WITH_KNOTS ( ( 3, 2, 2, 2, 3 ),
 ( 0.2583333333333333037, 0.2592592592592592449, 0.2611111111111111271, 0.2629629629629629539, 0.2638888888888888951 ),
 .UNSPECIFIED. ) 
 CURVE ( )  GEOMETRIC_REPRESENTATION_ITEM ( )  RATIONAL_B_SPLINE_CURVE ( ( 0.9330127018922194093, 0.9330127018922174109, 1.000000000000000000, 0.8660254037844388186, 1.000000000000000000, 0.8660254037844388186, 1.000000000000000000, 0.9330127018922194093, 0.9330127018922194093 ) ) 
 REPRESENTATION_ITEM ( '' )  );
#24007 = CARTESIAN_POINT ( 'NONE',  ( 3.608439182435180470, 6.249999999999982236, -86.05801270189222407 ) ) ;
#24008 = DIRECTION ( 'NONE',  ( -0.7071067811865477948, 3.925231146709432986E-17, -0.7071067811865472397 ) ) ;
#24009 = CARTESIAN_POINT ( 'NONE',  ( 5.999999999999949374, 1.607695154586804565, -150.0193375672974128 ) ) ;
#24010 = DIRECTION ( 'NONE',  ( -1.000000000000000000, -0.000000000000000000, -0.000000000000000000 ) ) ;
#24011 = CARTESIAN_POINT ( 'NONE',  ( 140.8038234968595646, -11.90191174842906108, -4.000000000000003553 ) ) ;
#24012 = CARTESIAN_POINT ( 'NONE',  ( 116.6877832217621460, -0.7662911109077388261, 1.849990392679712103 ) ) ;
#24013 =( BOUNDED_CURVE ( )  B_SPLINE_CURVE ( 2, ( #10644, #22304, #19840, #10181, #24436, #14654, #10333, #19552, #28885 ),
 .UNSPECIFIED., .F., .T. ) 
 B_SPLINE_CURVE_WITH_KNOTS ( ( 3, 2, 2, 2, 3 ),
 ( 0.2305555555555556246, 0.2314814814814815103, 0.2333333333333332815, 0.2351851851851851638, 0.2361111111111110494 ),
 .UNSPECIFIED. ) 
 CURVE ( )  GEOMETRIC_REPRESENTATION_ITEM ( )  RATIONAL_B_SPLINE_CURVE ( ( 0.9330127018922194093, 0.9330127018922234061, 1.000000000000000000, 0.8660254037844388186, 1.000000000000000000, 0.8660254037844388186, 1.000000000000000000, 0.9330127018922234061, 0.9330127018922194093 ) ) 
 REPRESENTATION_ITEM ( '' )  );
#24014 = CARTESIAN_POINT ( 'NONE',  ( -3.175426480542816066, -5.500000000000057732, -137.3750000000000568 ) ) ;
#24015 = CARTESIAN_POINT ( 'NONE',  ( 139.8373098077242105, -9.046954833815613384, 7.886428923425581772 ) ) ;
#24016 = CARTESIAN_POINT ( 'NONE',  ( -7.216878364870328078, 0.000000000000000000, -153.0580127018922383 ) ) ;
#24017 = CARTESIAN_POINT ( 'NONE',  ( 4.763139720814407951, 2.750000000000002665, -67.75000000000002842 ) ) ;
#24018 = CARTESIAN_POINT ( 'NONE',  ( -4.763139720814407951, 2.749999999999946709, -65.75000000000002842 ) ) ;
#24019 = EDGE_CURVE ( 'NONE', #23883, #14503, #15862, .T. ) ;
#24020 =( NAMED_UNIT ( * ) SI_UNIT ( $, .STERADIAN. ) SOLID_ANGLE_UNIT ( ) );
#24021 = CARTESIAN_POINT ( 'NONE',  ( 147.1086002691896510, -2.071067811865468400, -4.999999999999989342 ) ) ;
#24022 = CARTESIAN_POINT ( 'NONE',  ( 150.4687500000000284, -2.485281374238585972, 6.000000000000005329 ) ) ;
#24023 = CARTESIAN_POINT ( 'NONE',  ( -3.464101615137725076, 5.999999999999979572, -127.0863248654051887 ) ) ;
#24024 = VECTOR ( 'NONE', #10735, 1000.000000000000000 ) ;
#24025 = CARTESIAN_POINT ( 'NONE',  ( 3.464101615137757051, -5.999999999999979572, -104.4136751345948539 ) ) ;
#24026 = CYLINDRICAL_SURFACE ( 'NONE', #15533, 6.000000000000000888 ) ;
#24027 = ORIENTED_EDGE ( 'NONE', *, *, #4350, .F. ) ;
#24028 = CIRCLE ( 'NONE', #16231, 0.5000000000000004441 ) ;
#24029 = CARTESIAN_POINT ( 'NONE',  ( 152.4375000000000284, -4.242640687119298093, -4.242640687119298093 ) ) ;
#24030 = VECTOR ( 'NONE', #13752, 1000.000000000000000 ) ;
#24031 = CARTESIAN_POINT ( 'NONE',  ( -5.999999999999962697, 3.323446944526963891E-14, -158.9136751345947971 ) ) ;
#24032 = CARTESIAN_POINT ( 'NONE',  ( 4.763139720814407951, 2.750000000000002665, -177.2500000000000284 ) ) ;
#24033 = CARTESIAN_POINT ( 'NONE',  ( 21.56250000000015987, -1.999999999999911626, -0.8284271247462354770 ) ) ;
#24034 = ORIENTED_EDGE ( 'NONE', *, *, #8120, .F. ) ;
#24035 = CARTESIAN_POINT ( 'NONE',  ( 3.608439182435180470, 6.249999999999982236, -154.1919872981078186 ) ) ;
#24036 = ORIENTED_EDGE ( 'NONE', *, *, #23282, .F. ) ;
#24037 = CARTESIAN_POINT ( 'NONE',  ( -4.763139720814407951, 2.749999999999946709, -80.74999999999998579 ) ) ;
#24038 = CARTESIAN_POINT ( 'NONE',  ( 3.608439182435180470, 6.249999999999982236, -101.0580127018922241 ) ) ;
#24039 = ORIENTED_EDGE ( 'NONE', *, *, #25044, .F. ) ;
#24040 = CARTESIAN_POINT ( 'NONE',  ( 119.9999999999999005, 0.6961469067658530019, 2.048720570865176338 ) ) ;
#24041 = EDGE_CURVE ( 'NONE', #9495, #12642, #13748, .T. ) ;
#24042 = CARTESIAN_POINT ( 'NONE',  ( 6.350852961086080661, -9.614813431917819062E-14, -168.3750000000000568 ) ) ;
#24043 = CARTESIAN_POINT ( 'NONE',  ( 111.2886751345946834, 2.000000000000001776, 3.330669073875469621E-13 ) ) ;
#24044 = CARTESIAN_POINT ( 'NONE',  ( 5.920437777358367626, -9.270953676058775628, -24.00610273346770640 ) ) ;
#24045 = CARTESIAN_POINT ( 'NONE',  ( 3.175426480543072749, -5.500000000000105693, -167.1250000000000000 ) ) ;
#24046 = CARTESIAN_POINT ( 'NONE',  ( 3.464101615137757051, -5.999999999999979572, -60.33632486540521001 ) ) ;
#24047 = CARTESIAN_POINT ( 'NONE',  ( 4.763139720814407951, 2.750000000000002665, -147.2500000000000000 ) ) ;
#24048 = CYLINDRICAL_SURFACE ( 'NONE', #13031, 6.000000000000000888 ) ;
#24049 = DIRECTION ( 'NONE',  ( 0.000000000000000000, -1.000000000000000000, -8.881784197001264156E-16 ) ) ;
#24050 = CARTESIAN_POINT ( 'NONE',  ( 3.175426480543072749, 5.499999999999865885, -97.62500000000004263 ) ) ;
#24051 = CARTESIAN_POINT ( 'NONE',  ( 115.7261751345947118, -1.999999999999941602, 0.8284271247464759513 ) ) ;
#24052 = CARTESIAN_POINT ( 'NONE',  ( 4.763139720814407951, 2.750000000000002665, -91.75000000000000000 ) ) ;
#24053 = EDGE_CURVE ( 'NONE', #5313, #2934, #8162, .T. ) ;
#24054 = CARTESIAN_POINT ( 'NONE',  ( 6.000000000000000888, 1.743066579297358182E-13, -99.66367513459479710 ) ) ;
#24055 = CARTESIAN_POINT ( 'NONE',  ( -5.196152422706601826, 2.999999999999975131, -64.53867513459482552 ) ) ;
#24056 = CARTESIAN_POINT ( 'NONE',  ( 6.000000000000000888, -1.859271017917181981E-14, -93.66367513459481131 ) ) ;
#24057 = CARTESIAN_POINT ( 'NONE',  ( 9.750000000000092371, 1.873492889145011997, 1.873492889144678930 ) ) ;
#24058 = CARTESIAN_POINT ( 'NONE',  ( 109.0624999999997868, 2.500000000000055067, 1.035533905932809473 ) ) ;
#24059 = CARTESIAN_POINT ( 'NONE',  ( -3.464101615137725076, 5.999999999999979572, -126.1636751345948113 ) ) ;
#24060 =( BOUNDED_CURVE ( )  B_SPLINE_CURVE ( 2, ( #4017, #30288, #9097, #9248, #8954, #27814, #8801, #6321, #15750 ),
 .UNSPECIFIED., .F., .F. ) 
 B_SPLINE_CURVE_WITH_KNOTS ( ( 3, 2, 2, 2, 3 ),
 ( 0.4218750000000000000, 0.4296875000000000000, 0.4375000000000000000, 0.4453125000000000000, 0.4531250000000000000 ),
 .UNSPECIFIED. ) 
 CURVE ( )  GEOMETRIC_REPRESENTATION_ITEM ( )  RATIONAL_B_SPLINE_CURVE ( ( 1.000000000000000000, 0.9238795325112867385, 1.000000000000000000, 0.9238795325112867385, 1.000000000000000000, 0.9238795325112867385, 1.000000000000000000, 0.9238795325112867385, 1.000000000000000000 ) ) 
 REPRESENTATION_ITEM ( '' )  );
#24061 = CARTESIAN_POINT ( 'NONE',  ( 113.1488248654051176, -1.999999999999941602, 0.8284271247465359034 ) ) ;
#24062 = ORIENTED_EDGE ( 'NONE', *, *, #8222, .F. ) ;
#24063 = CARTESIAN_POINT ( 'NONE',  ( 0.000000000000000000, 0.000000000000000000, 0.000000000000000000 ) ) ;
#24064 = CARTESIAN_POINT ( 'NONE',  ( 119.6252832217623165, 0.000000000000000000, 1.849990392679523588 ) ) ;
#24065 = AXIS2_PLACEMENT_3D ( 'NONE', #24556, #10455, #27010 ) ;
#24066 = EDGE_LOOP ( 'NONE', ( #4688, #1625, #23503, #22955 ) ) ;
#24067 = ORIENTED_EDGE ( 'NONE', *, *, #5246, .T. ) ;
#24068 = CARTESIAN_POINT ( 'NONE',  ( -3.175426480542816510, -5.500000000000057732, -104.3750000000000142 ) ) ;
#24069 = CARTESIAN_POINT ( 'NONE',  ( 17.12500000000011369, 1.665334536937734811E-13, -2.649519052838444910 ) ) ;
#24070 = CARTESIAN_POINT ( 'NONE',  ( -3.608439182435115633, 6.249999999999965361, -123.3080127018922099 ) ) ;
#24071 = AXIS2_PLACEMENT_3D ( 'NONE', #1752, #22966, #25555 ) ;
#24072 = ORIENTED_EDGE ( 'NONE', *, *, #26161, .T. ) ;
#24073 = CARTESIAN_POINT ( 'NONE',  ( 113.8988248654049755, 0.8284271247462654530, 2.000000000000271783 ) ) ;
#24074 = CARTESIAN_POINT ( 'NONE',  ( 7.216878364870455975, -6.409875621278545621E-14, -157.4419872981077901 ) ) ;
#24075 = CARTESIAN_POINT ( 'NONE',  ( 104.7499999999998295, 5.551115123125782702E-14, -2.499999999999835687 ) ) ;
#24076 = CARTESIAN_POINT ( 'NONE',  ( 131.9851497308104058, -3.535533905932725318, 3.535533905932725318 ) ) ;
#24077 = EDGE_CURVE ( 'NONE', #14503, #14874, #22935, .T. ) ;
#24078 = CARTESIAN_POINT ( 'NONE',  ( 5.412658773652712085, -3.125000000000086153, -57.93301270189221697 ) ) ;
#24079 = EDGE_LOOP ( 'NONE', ( #26059, #28927, #12776, #6550 ) ) ;
#24080 = CARTESIAN_POINT ( 'NONE',  ( 5.196152422706629359, 3.000000000000002665, -117.5386751345948113 ) ) ;
#24081 = CARTESIAN_POINT ( 'NONE',  ( 141.4613248654052597, -5.500000000000005329, 0.000000000000000000 ) ) ;
#24082 = CARTESIAN_POINT ( 'NONE',  ( 6.000000000000000888, 7.762456499804235646E-14, -142.5863248654051745 ) ) ;
#24083 = CARTESIAN_POINT ( 'NONE',  ( 119.1249999999999432, 1.767766952966348670, 1.767766952966431937 ) ) ;
#24084 = LINE ( 'NONE', #431, #19139 ) ;
#24085 = CARTESIAN_POINT ( 'NONE',  ( -3.608439182435052128, -6.250000000000110134, -167.8080127018922951 ) ) ;
#24086 = DIRECTION ( 'NONE',  ( 0.000000000000000000, 0.000000000000000000, -1.000000000000000000 ) ) ;
#24087 = DIRECTION ( 'NONE',  ( 1.000000000000000000, -0.000000000000000000, -0.000000000000000000 ) ) ;
#24088 = AXIS2_PLACEMENT_3D ( 'NONE', #6181, #25058, #20465 ) ;
#24089 = CARTESIAN_POINT ( 'NONE',  ( -4.763139720814407951, -2.750000000000016431, -114.9999999999999858 ) ) ;
#24090 = EDGE_CURVE ( 'NONE', #21961, #9159, #24060, .T. ) ;
#24091 = CARTESIAN_POINT ( 'NONE',  ( 3.175426480543072749, -5.500000000000105693, -114.6250000000000000 ) ) ;
#24092 = DIRECTION ( 'NONE',  ( 0.000000000000000000, 0.000000000000000000, -1.000000000000000000 ) ) ;
#24093 = CARTESIAN_POINT ( 'NONE',  ( 0.000000000000000000, 5.999999999999977796, -100.7886751345948255 ) ) ;
#24094 = VECTOR ( 'NONE', #19328, 1000.000000000000000 ) ;
#24095 = EDGE_LOOP ( 'NONE', ( #24465, #15044, #27760, #6298 ) ) ;
#24096 = CARTESIAN_POINT ( 'NONE',  ( 17.62500000000011369, 2.649519052838500421, 0.000000000000000000 ) ) ;
#24097 = DIRECTION ( 'NONE',  ( -0.000000000000000000, -0.000000000000000000, -1.000000000000000000 ) ) ;
#24098 = FACE_OUTER_BOUND ( 'NONE', #11463, .T. ) ;
#24099 =( BOUNDED_CURVE ( )  B_SPLINE_CURVE ( 2, ( #2128, #2283, #18583, #8890, #18427, #20400, #16301, #11054, #13842 ),
 .UNSPECIFIED., .F., .T. ) 
 B_SPLINE_CURVE_WITH_KNOTS ( ( 3, 2, 2, 2, 3 ),
 ( 0.4861111111111111605, 0.4870370370370370461, 0.4888888888888889284, 0.4907407407407406996, 0.4916666666666665853 ),
 .UNSPECIFIED. ) 
 CURVE ( )  GEOMETRIC_REPRESENTATION_ITEM ( )  RATIONAL_B_SPLINE_CURVE ( ( 0.9330127018922194093, 0.9330127018922234061, 1.000000000000000000, 0.8660254037844388186, 1.000000000000000000, 0.8660254037844388186, 1.000000000000000000, 0.9330127018922234061, 0.9330127018922194093 ) ) 
 REPRESENTATION_ITEM ( '' )  );
#24100 = VERTEX_POINT ( 'NONE', #25060 ) ;
#24101 = CARTESIAN_POINT ( 'NONE',  ( 0.000000000000000000, -9.500000000000008882, -7.500000000000007105 ) ) ;
#24102 = LINE ( 'NONE', #16923, #29764 ) ;
#24103 = ORIENTED_EDGE ( 'NONE', *, *, #1051, .T. ) ;
#24104 = CARTESIAN_POINT ( 'NONE',  ( -5.999999999999963585, 8.134310703387671600E-14, -125.9136751345948397 ) ) ;
#24105 = ORIENTED_EDGE ( 'NONE', *, *, #28474, .F. ) ;
#24106 = ORIENTED_EDGE ( 'NONE', *, *, #29806, .F. ) ;
#24107 = CARTESIAN_POINT ( 'NONE',  ( 1.110223024625164183E-16, -2.000000000000012879, -1.776356839400262692E-15 ) ) ;
#24108 = CARTESIAN_POINT ( 'NONE',  ( 135.6711002691896795, 4.999999999999989342, 2.071067811865468400 ) ) ;
#24109 = STYLED_ITEM ( 'NONE', ( #21344 ), #29379 ) ;
#24110 = CARTESIAN_POINT ( 'NONE',  ( 157.3050748654052029, 5.500000000000012434, 2.278174593052012309 ) ) ;
#24111 = CARTESIAN_POINT ( 'NONE',  ( -3.608439182435052128, -6.250000000000110134, -129.4419872981078186 ) ) ;
#24112 = CARTESIAN_POINT ( 'NONE',  ( 104.4999999999998863, -2.499999999999919176, 0.000000000000000000 ) ) ;
#24113 = DIRECTION ( 'NONE',  ( 1.000000000000000000, -5.551115123125773458E-17, -1.260129944081490338E-35 ) ) ;
#24114 = DIRECTION ( 'NONE',  ( 1.000000000000000000, -5.551115123125773458E-17, -1.260129944081490338E-35 ) ) ;
#24115 = EDGE_CURVE ( 'NONE', #6843, #22842, #18641, .T. ) ;
#24116 = ORIENTED_EDGE ( 'NONE', *, *, #532, .T. ) ;
#24117 = CARTESIAN_POINT ( 'NONE',  ( 15.18750000000007105, 0.8284271247462955401, 1.999999999999851674 ) ) ;
#24118 = CARTESIAN_POINT ( 'NONE',  ( -5.999999999999963585, 1.780251999655701777E-13, -84.83632486540523132 ) ) ;
#24119 = DIRECTION ( 'NONE',  ( -7.147005652999508048E-36, 5.642372883946980038E-36, 1.000000000000000000 ) ) ;
#24120 = CARTESIAN_POINT ( 'NONE',  ( 135.6413997308104058, 2.071067811865468400, -4.999999999999989342 ) ) ;
#24121 =( GEOMETRIC_REPRESENTATION_CONTEXT ( 3 ) GLOBAL_UNCERTAINTY_ASSIGNED_CONTEXT ( ( #5019 ) ) GLOBAL_UNIT_ASSIGNED_CONTEXT ( ( #28319, #4220, #23297 ) ) REPRESENTATION_CONTEXT ( 'NONE', 'WORKASPACE' ) );
#24122 = CARTESIAN_POINT ( 'NONE',  ( 15.00000000000000000, 0.000000000000000000, 17.50000000000000355 ) ) ;
#24123 = CARTESIAN_POINT ( 'NONE',  ( -3.464101615137725076, 5.999999999999979572, -146.5863248654052313 ) ) ;
#24124 = VECTOR ( 'NONE', #1910, 1000.000000000000000 ) ;
#24125 = CARTESIAN_POINT ( 'NONE',  ( -6.000000000000007105, -1.607695154586655129, -162.7693375672974128 ) ) ;
#24126 = CARTESIAN_POINT ( 'NONE',  ( -5.196152422706573404, -3.000000000000002665, -115.2886751345948397 ) ) ;
#24127 = ADVANCED_FACE ( 'NONE', ( #29975 ), #4627, .T. ) ;
#24128 = CARTESIAN_POINT ( 'NONE',  ( 4.763139720814407951, 2.750000000000002665, -133.7500000000000284 ) ) ;
#24129 = ADVANCED_FACE ( 'NONE', ( #14060 ), #22971, .T. ) ;
#24130 = CIRCLE ( 'NONE', #19242, 4.000000000000010658 ) ;
#24131 = PRESENTATION_STYLE_ASSIGNMENT (( #8132 ) ) ;
#24132 = ORIENTED_EDGE ( 'NONE', *, *, #6128, .F. ) ;
#24133 = VECTOR ( 'NONE', #5933, 1000.000000000000000 ) ;
#24134 = CARTESIAN_POINT ( 'NONE',  ( 118.1636751345947829, 1.414213562373090038, -1.414213562373145550 ) ) ;
#24135 = B_SPLINE_CURVE_WITH_KNOTS ( 'NONE', 3,
 ( #24378, #10894, #6099, #1025, #12904, #24682 ),
 .UNSPECIFIED., .F., .F.,
 ( 4, 2, 4 ),
 ( 0.000000000000000000, 0.001072522389057928034, 0.002145044778115856067 ),
 .UNSPECIFIED. ) ;
#24136 = EDGE_LOOP ( 'NONE', ( #9926, #4272, #3524, #3714 ) ) ;
#24137 = CARTESIAN_POINT ( 'NONE',  ( 119.4997167782375982, 1.308140751793723799, -1.308140751793640533 ) ) ;
#24138 = SURFACE_SIDE_STYLE ('',( #21402 ) ) ;
#24139 = CARTESIAN_POINT ( 'NONE',  ( -7.216878364870328078, 0.000000000000000000, -98.19198729810781856 ) ) ;
#24140 = CARTESIAN_POINT ( 'NONE',  ( 158.9136751345948539, 0.000000000000000000, -5.500000000000005329 ) ) ;
#24141 = DIRECTION ( 'NONE',  ( 0.000000000000000000, 1.776356839400250465E-15, 1.000000000000000000 ) ) ;
#24142 = CARTESIAN_POINT ( 'NONE',  ( 113.5624999999997016, -2.499999999999964473, -1.035533905932689347 ) ) ;
#24143 = CARTESIAN_POINT ( 'NONE',  ( -19.99999999999998224, -54.99999999999990763, 8.000000000000007105 ) ) ;
#24144 =( BOUNDED_CURVE ( )  B_SPLINE_CURVE ( 2, ( #11734, #16049, #13584, #27801, #20927, #27496, #16350, #4472, #6779 ),
 .UNSPECIFIED., .F., .F. ) 
 B_SPLINE_CURVE_WITH_KNOTS ( ( 3, 2, 2, 2, 3 ),
 ( 0.2968750000000000000, 0.3046875000000000000, 0.3125000000000000000, 0.3203125000000000000, 0.3281250000000000000 ),
 .UNSPECIFIED. ) 
 CURVE ( )  GEOMETRIC_REPRESENTATION_ITEM ( )  RATIONAL_B_SPLINE_CURVE ( ( 1.000000000000000000, 0.9238795325112867385, 1.000000000000000000, 0.9238795325112867385, 1.000000000000000000, 0.9238795325112867385, 1.000000000000000000, 0.9238795325112867385, 1.000000000000000000 ) ) 
 REPRESENTATION_ITEM ( '' )  );
#24145 = CARTESIAN_POINT ( 'NONE',  ( 4.763139720814407951, -2.749999999999988454, -132.5000000000000000 ) ) ;
#24146 = ORIENTED_EDGE ( 'NONE', *, *, #27994, .F. ) ;
#24147 = EDGE_LOOP ( 'NONE', ( #8099, #26873, #10186, #2980 ) ) ;
#24148 = CARTESIAN_POINT ( 'NONE',  ( 159.1298473403915068, -11.07692307692306777, 4.615384615384606093 ) ) ;
#24149 = CARTESIAN_POINT ( 'NONE',  ( -2.775557561562891351E-14, -5.500000000000115463, -54.75000000000002132 ) ) ;
#24150 = ADVANCED_FACE ( 'NONE', ( #20323 ), #14207, .T. ) ;
#24151 = CARTESIAN_POINT ( 'NONE',  ( 140.1636751345948255, 0.000000000000000000, 5.500000000000005329 ) ) ;
#24152 = CARTESIAN_POINT ( 'NONE',  ( 5.196152422706629359, -2.999999999999988898, -62.28867513459485394 ) ) ;
#24153 = CARTESIAN_POINT ( 'NONE',  ( 5.381246803625141517, 9.595437032880905548, -22.31808132294488445 ) ) ;
#24154 = EDGE_CURVE ( 'NONE', #2721, #14144, #18981, .T. ) ;
#24155 = CARTESIAN_POINT ( 'NONE',  ( -5.412658773652684552, -3.125000000000099920, -74.93301270189223828 ) ) ;
#24156 = DIRECTION ( 'NONE',  ( 1.000000000000000000, -5.551115123125773458E-17, -1.260129944081490338E-35 ) ) ;
#24157 = CARTESIAN_POINT ( 'NONE',  ( 0.000000000000000000, 0.000000000000000000, -14.99152654425661702 ) ) ;
#24158 = CARTESIAN_POINT ( 'NONE',  ( 140.4088296780374776, -11.40882967803863934, -4.170790813163522515 ) ) ;
#24159 = DIRECTION ( 'NONE',  ( -7.147005652999508048E-36, 5.642372883946980038E-36, 1.000000000000000000 ) ) ;
#24160 = CARTESIAN_POINT ( 'NONE',  ( 115.6252832217622597, 0.000000000000000000, 1.849990392679523588 ) ) ;
#24161 = CARTESIAN_POINT ( 'NONE',  ( 0.000000000000000000, 5.499999999999991118, -141.0000000000000000 ) ) ;
#24162 = CARTESIAN_POINT ( 'NONE',  ( 139.6504835472090349, -9.198789620363742259, 7.981988490022517979 ) ) ;
#24163 = CARTESIAN_POINT ( 'NONE',  ( 7.216878364870455975, -6.409875621278545621E-14, -155.3080127018922099 ) ) ;
#24164 = CARTESIAN_POINT ( 'NONE',  ( 139.9761751345948539, 3.889087296526011706, 3.889087296526011706 ) ) ;
#24165 = PRESENTATION_STYLE_ASSIGNMENT (( #12532 ) ) ;
#24166 = CARTESIAN_POINT ( 'NONE',  ( -6.350852961085760029, -1.281975124255709124E-13, -67.12500000000002842 ) ) ;
#24167 = CARTESIAN_POINT ( 'NONE',  ( 5.196152422706629359, 3.000000000000002665, -86.03867513459483973 ) ) ;
#24168 = CARTESIAN_POINT ( 'NONE',  ( -3.175426480542816510, -5.500000000000057732, -54.87500000000003553 ) ) ;
#24169 = DIRECTION ( 'NONE',  ( 0.000000000000000000, 0.000000000000000000, 1.000000000000000000 ) ) ;
#24170 = EDGE_LOOP ( 'NONE', ( #4652, #11574, #18673, #21097 ) ) ;
#24171 = CARTESIAN_POINT ( 'NONE',  ( 146.2648502691896510, 3.535533905932725318, 3.535533905932752852 ) ) ;
#24172 = CARTESIAN_POINT ( 'NONE',  ( 151.5937500000000284, 6.000000000000005329, 2.485281374238585972 ) ) ;
#24173 = DIRECTION ( 'NONE',  ( -7.155734338404322954E-15, 0.000000000000000000, 1.000000000000000000 ) ) ;
#24174 = CARTESIAN_POINT ( 'NONE',  ( 13.81249999999996980, 0.8284271247461753029, -2.000000000000091926 ) ) ;
#24175 = DIRECTION ( 'NONE',  ( -7.147005652999508048E-36, 5.642372883946980038E-36, 1.000000000000000000 ) ) ;
#24176 = EDGE_LOOP ( 'NONE', ( #18878, #15703, #21046, #21197 ) ) ;
#24177 = CARTESIAN_POINT ( 'NONE',  ( 142.5937500000000568, 6.000000000000005329, 2.485281374238585972 ) ) ;
#24178 =( BOUNDED_CURVE ( )  B_SPLINE_CURVE ( 2, ( #27569, #23003, #25749, #9480, #6706, #15969, #25267, #4239, #4695 ),
 .UNSPECIFIED., .F., .F. ) 
 B_SPLINE_CURVE_WITH_KNOTS ( ( 3, 2, 2, 2, 3 ),
 ( 0.5583333333333333481, 0.5592592592592592338, 0.5611111111111111160, 0.5629629629629629983, 0.5638888888888888840 ),
 .UNSPECIFIED. ) 
 CURVE ( )  GEOMETRIC_REPRESENTATION_ITEM ( )  RATIONAL_B_SPLINE_CURVE ( ( 0.9330127018922194093, 0.9330127018922194093, 1.000000000000000000, 0.8660254037844388186, 1.000000000000000000, 0.8660254037844388186, 1.000000000000000000, 0.9330127018922194093, 0.9330127018922194093 ) ) 
 REPRESENTATION_ITEM ( '' )  );
#24179 = DIRECTION ( 'NONE',  ( -6.938893903907250071E-16, 0.6000000000000006439, -0.7999999999999997113 ) ) ;
#24180 = CARTESIAN_POINT ( 'NONE',  ( 3.608439182435180470, -6.249999999999997335, -46.69198729810783277 ) ) ;
#24181 = CARTESIAN_POINT ( 'NONE',  ( 17.31250000000003908, -0.8284271247461153509, 2.000000000000091926 ) ) ;
#24182 = EDGE_LOOP ( 'NONE', ( #30076, #21002, #21316, #3112 ) ) ;
#24183 = CARTESIAN_POINT ( 'NONE',  ( 4.763139720814407951, -2.749999999999988454, -81.50000000000001421 ) ) ;
#24184 = EDGE_CURVE ( 'NONE', #23551, #16922, #18801, .T. ) ;
#24185 = EDGE_CURVE ( 'NONE', #12143, #26678, #22097, .T. ) ;
#24186 =( BOUNDED_CURVE ( )  B_SPLINE_CURVE ( 2, ( #28468, #2824, #14541, #12247, #18845, #18541, #6835, #16259, #28168 ),
 .UNSPECIFIED., .F., .T. ) 
 B_SPLINE_CURVE_WITH_KNOTS ( ( 3, 2, 2, 2, 3 ),
 ( 0.7472222222222222321, 0.7481481481481482287, 0.7500000000000000000, 0.7518518518518518823, 0.7527777777777777679 ),
 .UNSPECIFIED. ) 
 CURVE ( )  GEOMETRIC_REPRESENTATION_ITEM ( )  RATIONAL_B_SPLINE_CURVE ( ( 0.9330127018922194093, 0.9330127018922194093, 1.000000000000000000, 0.8660254037844388186, 1.000000000000000000, 0.8660254037844388186, 1.000000000000000000, 0.9330127018922234061, 0.9330127018922194093 ) ) 
 REPRESENTATION_ITEM ( '' )  );
#24187 = CARTESIAN_POINT ( 'NONE',  ( 5.196152422706629359, 3.000000000000002665, -176.0386751345948255 ) ) ;
#24188 = CARTESIAN_POINT ( 'NONE',  ( 6.000000000000000888, -3.330669073875464691E-16, -7.560779664488942560E-35 ) ) ;
#24189 = CARTESIAN_POINT ( 'NONE',  ( 5.990257846049584778, -9.225907948257320967, -24.60347258678507387 ) ) ;
#24190 = CARTESIAN_POINT ( 'NONE',  ( 111.6488248654050750, 2.000000000000061728, -0.8284271247459952248 ) ) ;
#24191 = CARTESIAN_POINT ( 'NONE',  ( 140.0769230769231228, -11.53846153846155254, 4.615384615384630074 ) ) ;
#24192 = VECTOR ( 'NONE', #24740, 1000.000000000000000 ) ;
#24193 = CARTESIAN_POINT ( 'NONE',  ( -2.775557561562891351E-14, -5.500000000000115463, -165.7500000000000000 ) ) ;
#24194 = CARTESIAN_POINT ( 'NONE',  ( 4.763139720814407951, -2.749999999999988454, -150.5000000000000284 ) ) ;
#24195 = CARTESIAN_POINT ( 'NONE',  ( -1.000000000000000888, -19.99999999999998934, 4.000000000000003553 ) ) ;
#24196 = CARTESIAN_POINT ( 'NONE',  ( -3.175426480542816066, 5.499999999999865885, -95.87500000000004263 ) ) ;
#24197 = CARTESIAN_POINT ( 'NONE',  ( 6.000000000000000888, -1.859271017917181981E-14, -130.5863248654052313 ) ) ;
#24198 = CARTESIAN_POINT ( 'NONE',  ( -3.175426480542816510, 5.499999999999865885, -79.37500000000001421 ) ) ;
#24199 = CARTESIAN_POINT ( 'NONE',  ( 0.000000000000000000, 0.000000000000000000, 0.000000000000000000 ) ) ;
#24200 = CARTESIAN_POINT ( 'NONE',  ( -3.464101615137757051, -5.999999999999979572, -136.1636751345947971 ) ) ;
#24201 = CARTESIAN_POINT ( 'NONE',  ( 23.25000000000004974, 5.551115123125782702E-14, 1.999999999999946265 ) ) ;
#24202 = DIRECTION ( 'NONE',  ( 1.000000000000000000, 0.000000000000000000, 0.000000000000000000 ) ) ;
#24203 = DIRECTION ( 'NONE',  ( -7.147005652999508048E-36, 5.642372883946980038E-36, 1.000000000000000000 ) ) ;
#24204 = ORIENTED_EDGE ( 'NONE', *, *, #3831, .T. ) ;
#24205 = CARTESIAN_POINT ( 'NONE',  ( 160.7812500000000568, 2.485281374238585972, 6.000000000000005329 ) ) ;
#24206 = DIRECTION ( 'NONE',  ( -7.147005652999508048E-36, 5.642372883946980038E-36, 1.000000000000000000 ) ) ;
#24207 = CARTESIAN_POINT ( 'NONE',  ( 3.464101615137757051, -5.999999999999979572, -78.91367513459476868 ) ) ;
#24208 = CARTESIAN_POINT ( 'NONE',  ( 119.6877832217621176, -0.7662911109077686911, 1.849990392679532247 ) ) ;
#24209 = ORIENTED_EDGE ( 'NONE', *, *, #21744, .T. ) ;
#24210 = CARTESIAN_POINT ( 'NONE',  ( 147.0000000000000284, 6.000000000000005329, 0.000000000000000000 ) ) ;
#24211 = ORIENTED_EDGE ( 'NONE', *, *, #7025, .F. ) ;
#24212 = CARTESIAN_POINT ( 'NONE',  ( -6.350852961085760029, -1.281975124255709124E-13, -103.1250000000000000 ) ) ;
#24213 = CARTESIAN_POINT ( 'NONE',  ( 19.87500000000008527, -2.649519052838111843, 1.110223024625156540E-13 ) ) ;
#24214 = ADVANCED_FACE ( 'NONE', ( #4924 ), #323, .T. ) ;
#24215 = CARTESIAN_POINT ( 'NONE',  ( -3.608439182435115633, 6.249999999999965361, -124.8080127018922099 ) ) ;
#24216 = VERTEX_POINT ( 'NONE', #26420 ) ;
#24217 = CARTESIAN_POINT ( 'NONE',  ( 0.000000000000000000, -5.999999999999991118, -110.5386751345948113 ) ) ;
#24218 = CARTESIAN_POINT ( 'NONE',  ( 3.608439182435180470, 6.249999999999982236, -164.6919872981078754 ) ) ;
#24219 = CARTESIAN_POINT ( 'NONE',  ( 135.0000000000000000, -7.391412244009264221, 8.245343090279524390 ) ) ;
#24220 =( BOUNDED_CURVE ( )  B_SPLINE_CURVE ( 2, ( #12046, #320, #1023, #8080, #10574, #19927, #9709, #11195, #11512 ),
 .UNSPECIFIED., .F., .F. ) 
 B_SPLINE_CURVE_WITH_KNOTS ( ( 3, 2, 2, 2, 3 ),
 ( 0.9249999999999999334, 0.9259259259259259300, 0.9277777777777778123, 0.9296296296296295836, 0.9305555555555555802 ),
 .UNSPECIFIED. ) 
 CURVE ( )  GEOMETRIC_REPRESENTATION_ITEM ( )  RATIONAL_B_SPLINE_CURVE ( ( 0.9330127018922194093, 0.9330127018922154125, 1.000000000000000000, 0.8660254037844388186, 1.000000000000000000, 0.8660254037844388186, 1.000000000000000000, 0.9330127018922154125, 0.9330127018922194093 ) ) 
 REPRESENTATION_ITEM ( '' )  );
#24221 = CARTESIAN_POINT ( 'NONE',  ( 3.608439182435180470, 6.249999999999982236, -57.55801270189221697 ) ) ;
#24222 = ORIENTED_EDGE ( 'NONE', *, *, #9401, .F. ) ;
#24223 = CARTESIAN_POINT ( 'NONE',  ( -0.04562205425674302484, -14.49999999999998046, -8.291335958003948292 ) ) ;
#24224 = CYLINDRICAL_SURFACE ( 'NONE', #16520, 6.000000000000000888 ) ;
#24225 = CARTESIAN_POINT ( 'NONE',  ( -9.999999999999980460, -60.00000000000001421, 4.000000000000003553 ) ) ;
#24226 = CARTESIAN_POINT ( 'NONE',  ( 3.175426480543072749, -5.500000000000105693, -168.6250000000000000 ) ) ;
#24227 = CARTESIAN_POINT ( 'NONE',  ( 120.5624999999997442, -2.499999999999964473, -1.035533905932508825 ) ) ;
#24228 = CARTESIAN_POINT ( 'NONE',  ( -5.412658773652739619, 3.124999999999975131, -168.1830127018922383 ) ) ;
#24229 = FACE_OUTER_BOUND ( 'NONE', #13691, .T. ) ;
#24230 = CARTESIAN_POINT ( 'NONE',  ( 24.43750000000014921, -1.999999999999851674, 0.8284271247462354770 ) ) ;
#24231 = CARTESIAN_POINT ( 'NONE',  ( 6.350852961086080661, -9.614813431917819062E-14, -118.8750000000000426 ) ) ;
#24232 =( NAMED_UNIT ( * ) SI_UNIT ( $, .STERADIAN. ) SOLID_ANGLE_UNIT ( ) );
#24233 = CARTESIAN_POINT ( 'NONE',  ( -2.775557561562891351E-14, -5.500000000000115463, -108.7500000000000142 ) ) ;
#24234 = DIRECTION ( 'NONE',  ( 1.000000000000000000, 0.000000000000000000, 0.000000000000000000 ) ) ;
#24235 = ORIENTED_EDGE ( 'NONE', *, *, #4133, .F. ) ;
#24236 = CARTESIAN_POINT ( 'NONE',  ( 18.62500000000011369, 2.649519052838500421, 0.000000000000000000 ) ) ;
#24237 = CARTESIAN_POINT ( 'NONE',  ( 6.000000000000052403, -1.607695154586662678, -90.15331216351299304 ) ) ;
#24238 = CARTESIAN_POINT ( 'NONE',  ( 6.000000000000052403, -1.607695154586662678, -75.73066243270262987 ) ) ;
#24239 = ORIENTED_EDGE ( 'NONE', *, *, #8455, .F. ) ;
#24240 = CARTESIAN_POINT ( 'NONE',  ( -3.464101615137757051, -5.999999999999979572, -127.1636751345948113 ) ) ;
#24241 = ADVANCED_FACE ( 'NONE', ( #25834, #21090 ), #21, .T. ) ;
#24242 = ADVANCED_FACE ( 'NONE', ( #5518 ), #22442, .T. ) ;
#24243 = CARTESIAN_POINT ( 'NONE',  ( 7.216878364870455975, -6.409875621278545621E-14, -79.44198729810779014 ) ) ;
#24244 = DIRECTION ( 'NONE',  ( 1.000000000000000000, 0.000000000000000000, 0.000000000000000000 ) ) ;
#24245 = ORIENTED_EDGE ( 'NONE', *, *, #8784, .F. ) ;
#24246 = CARTESIAN_POINT ( 'NONE',  ( -4.999999999999990230, -24.99999999999999289, 7.500000000000007105 ) ) ;
#24247 = ORIENTED_EDGE ( 'NONE', *, *, #28701, .T. ) ;
#24248 = EDGE_LOOP ( 'NONE', ( #4107, #21775, #7101, #13309 ) ) ;
#24249 = CARTESIAN_POINT ( 'NONE',  ( 161.8125000000000284, 4.242640687119298093, -4.242640687119298093 ) ) ;
#24250 = ORIENTED_EDGE ( 'NONE', *, *, #11726, .T. ) ;
#24251 = CARTESIAN_POINT ( 'NONE',  ( 3.608439182435180470, 6.249999999999982236, -128.6919872981078186 ) ) ;
#24252 =( LENGTH_UNIT ( ) NAMED_UNIT ( * ) SI_UNIT ( .MILLI., .METRE. ) );
#24253 = LINE ( 'NONE', #5974, #21453 ) ;
#24254 = MANIFOLD_SOLID_BREP ( 'Fillet1', #1140 ) ;
#24255 = ORIENTED_EDGE ( 'NONE', *, *, #27680, .F. ) ;
#24256 = CARTESIAN_POINT ( 'NONE',  ( 16.00000000000007105, 2.000000000000223821, -5.551115123125782702E-14 ) ) ;
#24257 = CARTESIAN_POINT ( 'NONE',  ( 6.000000000000000888, 7.762456499804235646E-14, -134.1636751345948539 ) ) ;
#24258 = CARTESIAN_POINT ( 'NONE',  ( 6.000000000000052403, -1.607695154586662678, -91.65331216351299304 ) ) ;
#24259 = CARTESIAN_POINT ( 'NONE',  ( 138.9226497308104342, 5.000000000000004441, 0.000000000000000000 ) ) ;
#24260 = LINE ( 'NONE', #20131, #22722 ) ;
#24261 = CARTESIAN_POINT ( 'NONE',  ( 5.196152422706629359, -2.999999999999988898, -162.2113248654052313 ) ) ;
#24262 = FILL_AREA_STYLE_COLOUR ( '', #3156 ) ;
#24263 = CARTESIAN_POINT ( 'NONE',  ( 106.6874999999998010, -1.035533905932689347, -2.499999999999784173 ) ) ;
#24264 =( BOUNDED_CURVE ( )  B_SPLINE_CURVE ( 2, ( #10911, #5494, #14900, #24240, #3191, #12616, #892, #19652, #28992 ),
 .UNSPECIFIED., .F., .T. ) 
 B_SPLINE_CURVE_WITH_KNOTS ( ( 3, 2, 2, 2, 3 ),
 ( 0.4027777777777777901, 0.4037037037037037313, 0.4055555555555555580, 0.4074074074074073848, 0.4083333333333333259 ),
 .UNSPECIFIED. ) 
 CURVE ( )  GEOMETRIC_REPRESENTATION_ITEM ( )  RATIONAL_B_SPLINE_CURVE ( ( 0.9330127018922194093, 0.9330127018922194093, 1.000000000000000000, 0.8660254037844388186, 1.000000000000000000, 0.8660254037844388186, 1.000000000000000000, 0.9330127018922194093, 0.9330127018922194093 ) ) 
 REPRESENTATION_ITEM ( '' )  );
#24265 = CARTESIAN_POINT ( 'NONE',  ( -6.350852961085760029, -1.281975124255709124E-13, -140.6249999999999716 ) ) ;
#24266 = CARTESIAN_POINT ( 'NONE',  ( 116.0000000000000142, 0.000000000000000000, 0.000000000000000000 ) ) ;
#24267 = CARTESIAN_POINT ( 'NONE',  ( 104.7401757384974417, 1.849990392679521589, 1.011113220803300925E-30 ) ) ;
#24268 = ORIENTED_EDGE ( 'NONE', *, *, #3195, .F. ) ;
#24269 = CARTESIAN_POINT ( 'NONE',  ( -5.196152422706601826, 2.999999999999975131, -173.4613248654052313 ) ) ;
#24270 = B_SPLINE_CURVE_WITH_KNOTS ( 'NONE', 3,
 ( #23486, #2426, #23773, #20716, #9124, #29851, #16381, #15933, #27383, #23275, #4511, #22806, #20964, #25702, #11145, #20493 ),
 .UNSPECIFIED., .F., .F.,
 ( 4, 2, 2, 2, 2, 2, 2, 4 ),
 ( 4.273303003478170257E-15, 0.0005126943745045677188, 0.001025388749004862163, 0.001538083123505156607, 0.002050777498005451269, 0.002563471872505745930, 0.003076166247006041025, 0.004101554996006630781 ),
 .UNSPECIFIED. ) ;
#24271 = CARTESIAN_POINT ( 'NONE',  ( -6.350852961085760029, -1.281975124255709124E-13, -50.62500000000001421 ) ) ;
#24272 = CARTESIAN_POINT ( 'NONE',  ( 16.96132486540522066, 1.110223024625156540E-13, 2.500000000000002220 ) ) ;
#24273 = CARTESIAN_POINT ( 'NONE',  ( 153.8363248654052029, 0.000000000000000000, -5.500000000000005329 ) ) ;
#24274 = CARTESIAN_POINT ( 'NONE',  ( -3.464101615137725076, 5.999999999999979572, -152.5863248654051745 ) ) ;
#24275 = ORIENTED_EDGE ( 'NONE', *, *, #18530, .T. ) ;
#24276 = CARTESIAN_POINT ( 'NONE',  ( 119.6247167782376124, 1.849990392679523588, 0.000000000000000000 ) ) ;
#24277 = CARTESIAN_POINT ( 'NONE',  ( 135.7500000000000284, -6.000000000000005329, 0.000000000000000000 ) ) ;
#24278 = CARTESIAN_POINT ( 'NONE',  ( 10.75000000000014921, 1.665334536937734811E-13, -2.000000000000168310 ) ) ;
#24279 = EDGE_CURVE ( 'NONE', #13349, #7272, #7569, .T. ) ;
#24280 = CARTESIAN_POINT ( 'NONE',  ( 2.775557561562891351E-14, -6.250000000000061284, -93.31698729810783277 ) ) ;
#24281 = CARTESIAN_POINT ( 'NONE',  ( -5.999999999999963585, -1.487416814333745711E-14, -50.91367513459483973 ) ) ;
#24282 = DIRECTION ( 'NONE',  ( 0.000000000000000000, -5.551115123125767911E-17, 1.000000000000000000 ) ) ;
#24283 = CARTESIAN_POINT ( 'NONE',  ( 114.9374999999997726, 2.500000000000054623, -1.035533905932629173 ) ) ;
#24284 = AXIS2_PLACEMENT_3D ( 'NONE', #10960, #8622, #6309 ) ;
#24285 = CARTESIAN_POINT ( 'NONE',  ( 140.6818792730027781, -11.36375854600488644, 4.222310544175423175 ) ) ;
#24286 = ADVANCED_FACE ( 'NONE', ( #21834 ), #732, .F. ) ;
#24287 = EDGE_CURVE ( 'NONE', #14937, #21073, #7202, .T. ) ;
#24288 = EDGE_LOOP ( 'NONE', ( #28487, #12406, #5315, #30269 ) ) ;
#24289 = CARTESIAN_POINT ( 'NONE',  ( 5.999999999999949374, -1.607695154586841868, -138.1533121635129930 ) ) ;
#24290 = AXIS2_PLACEMENT_3D ( 'NONE', #20836, #4680, #18847 ) ;
#24291 = CARTESIAN_POINT ( 'NONE',  ( 3.175426480543072749, 5.499999999999865885, -57.12500000000004974 ) ) ;
#24292 = CARTESIAN_POINT ( 'NONE',  ( 159.5699251345948255, 2.278174593052136210, 5.499999999999888978 ) ) ;
#24293 = CARTESIAN_POINT ( 'NONE',  ( 135.0000000000000284, 0.000000000000000000, 0.000000000000000000 ) ) ;
#24294 = CARTESIAN_POINT ( 'NONE',  ( -5.412658773652739619, 3.124999999999975131, -72.18301270189225249 ) ) ;
#24295 = CARTESIAN_POINT ( 'NONE',  ( 153.1726497308104058, -5.000000000000004441, 0.000000000000000000 ) ) ;
#24296 = CYLINDRICAL_SURFACE ( 'NONE', #3966, 6.000000000000000888 ) ;
#24297 = CARTESIAN_POINT ( 'NONE',  ( 3.464101615137757051, -5.999999999999979572, -168.3363248654051745 ) ) ;
#24298 =( NAMED_UNIT ( * ) SI_UNIT ( $, .STERADIAN. ) SOLID_ANGLE_UNIT ( ) );
#24299 = CARTESIAN_POINT ( 'NONE',  ( 3.175426480543072749, -5.500000000000105693, -140.1250000000000000 ) ) ;
#24300 = AXIS2_PLACEMENT_3D ( 'NONE', #25454, #23189, #4111 ) ;
#24301 = CARTESIAN_POINT ( 'NONE',  ( 105.4761751345946976, 0.8284271247463257382, 2.000000000000212275 ) ) ;
#24302 = CARTESIAN_POINT ( 'NONE',  ( 2.775557561562891351E-14, -6.250000000000061284, -151.1830127018922667 ) ) ;
#24303 = CARTESIAN_POINT ( 'NONE',  ( 140.1636751345948255, 0.000000000000000000, 5.500000000000005329 ) ) ;
#24304 = CARTESIAN_POINT ( 'NONE',  ( -3.175426480542816066, -5.500000000000057732, -74.37500000000000000 ) ) ;
#24305 = CARTESIAN_POINT ( 'NONE',  ( -2.775557561562891351E-14, -5.500000000000115463, -56.25000000000002132 ) ) ;
#24306 = DIRECTION ( 'NONE',  ( 0.000000000000000000, 0.000000000000000000, -1.000000000000000000 ) ) ;
#24307 = ORIENTED_EDGE ( 'NONE', *, *, #18246, .T. ) ;
#24308 = CARTESIAN_POINT ( 'NONE',  ( 140.1711002691896795, 4.999999999999989342, 2.071067811865468400 ) ) ;
#24309 = CARTESIAN_POINT ( 'NONE',  ( 149.9062500000000568, 6.000000000000005329, -2.485281374238556218 ) ) ;
#24310 = DIRECTION ( 'NONE',  ( -0.000000000000000000, -1.000000000000000000, -0.000000000000000000 ) ) ;
#24311 = AXIS2_PLACEMENT_3D ( 'NONE', #25946, #30252, #28240 ) ;
#24312 = EDGE_CURVE ( 'NONE', #12019, #21812, #13514, .T. ) ;
#24313 = CARTESIAN_POINT ( 'NONE',  ( 114.3747167782375556, -1.665334536937734811E-13, -1.849990392679523588 ) ) ;
#24314 = ORIENTED_EDGE ( 'NONE', *, *, #8081, .T. ) ;
#24315 = CARTESIAN_POINT ( 'NONE',  ( 142.5000000000000568, 6.000000000000005329, 0.000000000000000000 ) ) ;
#24316 = CARTESIAN_POINT ( 'NONE',  ( 0.000000000000000000, -5.999999999999991118, -121.9613248654052313 ) ) ;
#24317 = EDGE_CURVE ( 'NONE', #20296, #19034, #24472, .T. ) ;
#24318 = CARTESIAN_POINT ( 'NONE',  ( 116.0000000000000142, 6.735557395310442023E-16, 5.500000000000000000 ) ) ;
#24319 = CARTESIAN_POINT ( 'NONE',  ( -6.350852961085760029, -1.281975124255709124E-13, -181.1249999999999716 ) ) ;
#24320 = CARTESIAN_POINT ( 'NONE',  ( 16.06250000000006040, 2.000000000000151879, 0.8284271247461153509 ) ) ;
#24321 = CARTESIAN_POINT ( 'NONE',  ( -7.216878364870328078, 0.000000000000000000, -147.6919872981077901 ) ) ;
#24322 = ORIENTED_EDGE ( 'NONE', *, *, #8741, .T. ) ;
#24323 = CARTESIAN_POINT ( 'NONE',  ( 0.000000000000000000, 5.499999999999991118, -85.50000000000001421 ) ) ;
#24324 = CARTESIAN_POINT ( 'NONE',  ( 15.37500000000011013, 2.649519052838500421, -5.551115123125782702E-14 ) ) ;
#24325 = CARTESIAN_POINT ( 'NONE',  ( -7.216878364870328078, 0.000000000000000000, -93.05801270189225249 ) ) ;
#24326 = CARTESIAN_POINT ( 'NONE',  ( 119.9999999999998579, 0.3537249946243956056, 2.089338094881703967 ) ) ;
#24327 = CARTESIAN_POINT ( 'NONE',  ( -4.999999999999990230, -55.00000000000002132, 5.000000000000004441 ) ) ;
#24328 = DIRECTION ( 'NONE',  ( 0.000000000000000000, 0.000000000000000000, 1.000000000000000000 ) ) ;
#24329 = DIRECTION ( 'NONE',  ( -1.000000000000000000, -1.665334536937731113E-16, -8.326672684688674053E-17 ) ) ;
#24330 = PRESENTATION_STYLE_ASSIGNMENT (( #26340 ) ) ;
#24331 = CARTESIAN_POINT ( 'NONE',  ( 0.000000000000000000, 5.499999999999991118, -162.0000000000000284 ) ) ;
#24332 = CARTESIAN_POINT ( 'NONE',  ( -5.999999999999963585, -1.487416814333745711E-14, -133.4136751345948255 ) ) ;
#24333 = CARTESIAN_POINT ( 'NONE',  ( -4.763139720814407951, -2.750000000000016431, -148.0000000000000284 ) ) ;
#24334 = CARTESIAN_POINT ( 'NONE',  ( 5.196152422706629359, 3.000000000000002665, -77.03867513459483973 ) ) ;
#24335 = CARTESIAN_POINT ( 'NONE',  ( 6.000000000000000888, 1.743066579297358182E-13, -103.5863248654052171 ) ) ;
#24336 = CARTESIAN_POINT ( 'NONE',  ( 4.763139720814407951, -2.749999999999988454, -98.00000000000002842 ) ) ;
#24337 = DIRECTION ( 'NONE',  ( -8.326672684688675286E-17, -2.081668171172168821E-17, 1.000000000000000000 ) ) ;
#24338 = CYLINDRICAL_SURFACE ( 'NONE', #22129, 0.5000000000000004441 ) ;
#24339 = CARTESIAN_POINT ( 'NONE',  ( -4.763139720814407951, -2.750000000000016431, -83.50000000000001421 ) ) ;
#24340 = CARTESIAN_POINT ( 'NONE',  ( 152.9211002691896795, -4.999999999999989342, -2.071067811865468400 ) ) ;
#24341 = CARTESIAN_POINT ( 'NONE',  ( 6.000000000000000888, 1.743066579297358182E-13, -60.08632486540520290 ) ) ;
#24342 = CARTESIAN_POINT ( 'NONE',  ( 161.4590559403349630, -3.334791428567227989, -4.957026983497794248 ) ) ;
#24344 = CARTESIAN_POINT ( 'NONE',  ( 3.464101615137852974, 5.999999999999884537, -155.8363248654052029 ) ) ;
#24343 = AXIS2_PLACEMENT_3D ( 'NONE', #22934, #4016, #13433 ) ;
#24345 = CARTESIAN_POINT ( 'NONE',  ( 22.00000000000010303, 2.000000000000168310, 0.000000000000000000 ) ) ;
#24346 = CARTESIAN_POINT ( 'NONE',  ( 3.464101615137852974, 5.999999999999884537, -128.8363248654052029 ) ) ;
#24347 = EDGE_CURVE ( 'NONE', #23842, #23894, #29088, .T. ) ;
#24348 = DIRECTION ( 'NONE',  ( 1.000000000000000000, 0.000000000000000000, -0.000000000000000000 ) ) ;
#24349 = CARTESIAN_POINT ( 'NONE',  ( 3.464101615137852974, 5.999999999999884537, -78.41367513459479710 ) ) ;
#24350 =( BOUNDED_CURVE ( )  B_SPLINE_CURVE ( 2, ( #13801, #22829, #7140, #11173, #6837, #16261, #8853, #18236, #4224 ),
 .UNSPECIFIED., .F., .T. ) 
 B_SPLINE_CURVE_WITH_KNOTS ( ( 3, 2, 2, 2, 3 ),
 ( 0.08611111111111111049, 0.08703703703703703776, 0.08888888888888889228, 0.09074074074074074681, 0.09166666666666666019 ),
 .UNSPECIFIED. ) 
 CURVE ( )  GEOMETRIC_REPRESENTATION_ITEM ( )  RATIONAL_B_SPLINE_CURVE ( ( 0.9330127018922194093, 0.9330127018922194093, 1.000000000000000000, 0.8660254037844388186, 1.000000000000000000, 0.8660254037844388186, 1.000000000000000000, 0.9330127018922198534, 0.9330127018922194093 ) ) 
 REPRESENTATION_ITEM ( '' )  );
#24351 = ADVANCED_FACE ( 'NONE', ( #7601 ), #17936, .T. ) ;
#24352 = ORIENTED_EDGE ( 'NONE', *, *, #26398, .F. ) ;
#24353 = FILL_AREA_STYLE ('',( #21921 ) ) ;
#24354 = DIRECTION ( 'NONE',  ( 0.000000000000000000, 0.9165151389911677660, -0.4000000000000004663 ) ) ;
#24355 = CARTESIAN_POINT ( 'NONE',  ( 146.0699251345948255, 2.278174593052290753, 5.499999999999732658 ) ) ;
#24356 = CARTESIAN_POINT ( 'NONE',  ( 121.2502832217622171, 1.308140751793640533, -1.308140751793418488 ) ) ;
#24357 = CARTESIAN_POINT ( 'NONE',  ( 0.000000000000000000, 0.000000000000000000, 0.000000000000000000 ) ) ;
#24358 = ORIENTED_EDGE ( 'NONE', *, *, #10873, .T. ) ;
#24359 =( BOUNDED_CURVE ( )  B_SPLINE_CURVE ( 2, ( #20447, #5840, #15420, #15887, #25186, #4152, #17561, #26878, #24585 ),
 .UNSPECIFIED., .F., .T. ) 
 B_SPLINE_CURVE_WITH_KNOTS ( ( 3, 2, 2, 2, 3 ),
 ( 0.05833333333333334814, 0.05925925925925923377, 0.06111111111111111605, 0.06296296296296299833, 0.06388888888888888395 ),
 .UNSPECIFIED. ) 
 CURVE ( )  GEOMETRIC_REPRESENTATION_ITEM ( )  RATIONAL_B_SPLINE_CURVE ( ( 0.9330127018922194093, 0.9330127018922194093, 1.000000000000000000, 0.8660254037844388186, 1.000000000000000000, 0.8660254037844388186, 1.000000000000000000, 0.9330127018922194093, 0.9330127018922194093 ) ) 
 REPRESENTATION_ITEM ( '' )  );
#24360 = AXIS2_PLACEMENT_3D ( 'NONE', #14914, #3350, #24113 ) ;
#24361 = CARTESIAN_POINT ( 'NONE',  ( 146.3437500000000568, -6.000000000000005329, -2.485281374238555774 ) ) ;
#24362 = ORIENTED_EDGE ( 'NONE', *, *, #25790, .T. ) ;
#24363 = CARTESIAN_POINT ( 'NONE',  ( 4.763139720814407951, 2.750000000000002665, -102.2500000000000142 ) ) ;
#24364 = AXIS2_PLACEMENT_3D ( 'NONE', #11295, #11133, #27373 ) ;
#24365 = CARTESIAN_POINT ( 'NONE',  ( 20.31250000000012079, 2.649519052838358757, -1.097466725451559322 ) ) ;
#24366 = CARTESIAN_POINT ( 'NONE',  ( -5.412658773652739619, 3.124999999999975131, -112.6830127018922383 ) ) ;
#24367 = ORIENTED_EDGE ( 'NONE', *, *, #25187, .T. ) ;
#24368 = CARTESIAN_POINT ( 'NONE',  ( 5.999999999999949374, 1.607695154586804565, -111.5966878364870212 ) ) ;
#24369 = CARTESIAN_POINT ( 'NONE',  ( 5.412658773652739619, 3.124999999999988898, -160.3169872981078470 ) ) ;
#24370 = CARTESIAN_POINT ( 'NONE',  ( 104.8749999999998437, 1.767766952966320915, -1.767766952966431937 ) ) ;
#24371 = VECTOR ( 'NONE', #10488, 1000.000000000000000 ) ;
#24372 = CARTESIAN_POINT ( 'NONE',  ( 21.10117513459481486, 1.035533905932809473, -2.499999999999904521 ) ) ;
#24373 = CARTESIAN_POINT ( 'NONE',  ( 2.775557561562891351E-14, -6.250000000000061284, -59.68301270189224539 ) ) ;
#24374 = ORIENTED_EDGE ( 'NONE', *, *, #9466, .F. ) ;
#24375 = CARTESIAN_POINT ( 'NONE',  ( 6.000000000000000888, 7.762456499804234384E-14, -117.6636751345948255 ) ) ;
#24376 = CARTESIAN_POINT ( 'NONE',  ( -5.999999999999963585, -1.487416814333745711E-14, -105.8363248654052313 ) ) ;
#24377 = CARTESIAN_POINT ( 'NONE',  ( -2.686045755586558670, 10.67338275482133092, -19.62059632520456631 ) ) ;
#24378 = CARTESIAN_POINT ( 'NONE',  ( 1.000000000000000888, -16.43939393939394833, -5.999693900976793337 ) ) ;
#24379 = AXIS2_PLACEMENT_3D ( 'NONE', #11498, #30035, #27713 ) ;
#24380 = CARTESIAN_POINT ( 'NONE',  ( -2.775557561562891351E-14, -5.500000000000115463, -171.7500000000000000 ) ) ;
#24381 = CARTESIAN_POINT ( 'NONE',  ( 118.9374999999996589, 2.500000000000234479, -1.035533905932568777 ) ) ;
#24382 = CARTESIAN_POINT ( 'NONE',  ( -5.999999999999962697, -1.607695154586733288, -169.3466878364870354 ) ) ;
#24383 = CARTESIAN_POINT ( 'NONE',  ( -3.608439182435052128, -6.250000000000110134, -172.3080127018922383 ) ) ;
#24384 = CARTESIAN_POINT ( 'NONE',  ( 155.0550748654052313, -5.500000000000012434, -2.278174593052012309 ) ) ;
#24385 = CYLINDRICAL_SURFACE ( 'NONE', #17766, 6.000000000000000888 ) ;
#24386 = CARTESIAN_POINT ( 'NONE',  ( 3.175426480543072749, 5.499999999999865885, -115.6249999999999858 ) ) ;
#24387 = FACE_OUTER_BOUND ( 'NONE', #21356, .T. ) ;
#24388 = CARTESIAN_POINT ( 'NONE',  ( 3.175426480543072749, -5.500000000000105693, -108.6250000000000284 ) ) ;
#24389 = CARTESIAN_POINT ( 'NONE',  ( 6.000000000000052403, -1.607695154586662678, -111.7306624327026014 ) ) ;
#24390 = CARTESIAN_POINT ( 'NONE',  ( 11.03867513459494454, 1.665334536937734811E-13, -2.500000000000113243 ) ) ;
#24391 = CARTESIAN_POINT ( 'NONE',  ( 3.464101615137757051, -5.999999999999979572, -84.33632486540518869 ) ) ;
#24392 = ORIENTED_EDGE ( 'NONE', *, *, #18192, .T. ) ;
#24393 = CARTESIAN_POINT ( 'NONE',  ( 119.6249999999999716, -1.767766952966404181, -1.767766952966320915 ) ) ;
#24394 = CARTESIAN_POINT ( 'NONE',  ( -4.999999999999886313, -15.00000000000001421, 8.000000000000007105 ) ) ;
#24395 = MECHANICAL_DESIGN_GEOMETRIC_PRESENTATION_REPRESENTATION (  '', ( #29812 ), #8733 ) ;
#24396 = EDGE_CURVE ( 'NONE', #25843, #9799, #14851, .T. ) ;
#24397 = ORIENTED_EDGE ( 'NONE', *, *, #533, .T. ) ;
#24398 = CARTESIAN_POINT ( 'NONE',  ( -4.763139720814407951, -2.750000000000016431, -161.5000000000000284 ) ) ;
#24399 = CARTESIAN_POINT ( 'NONE',  ( 3.464101615137852974, 5.999999999999884537, -65.83632486540516027 ) ) ;
#24400 = CARTESIAN_POINT ( 'NONE',  ( 3.608439182435180470, 6.249999999999982236, -85.19198729810781856 ) ) ;
#24401 = ORIENTED_EDGE ( 'NONE', *, *, #23182, .F. ) ;
#24402 = CARTESIAN_POINT ( 'NONE',  ( 6.000000000000000888, 1.743066579297358182E-13, -75.66367513459485394 ) ) ;
#24403 = CIRCLE ( 'NONE', #26837, 0.5000000000000006661 ) ;
#24404 = ORIENTED_EDGE ( 'NONE', *, *, #30362, .F. ) ;
#24405 = CARTESIAN_POINT ( 'NONE',  ( 161.0625000000000284, -4.242640687119298093, 4.242640687119298093 ) ) ;
#24406 = ORIENTED_EDGE ( 'NONE', *, *, #5141, .F. ) ;
#24407 = CARTESIAN_POINT ( 'NONE',  ( -5.412658773652684552, -3.125000000000099920, -132.5669872981078470 ) ) ;
#24408 = CARTESIAN_POINT ( 'NONE',  ( -39.00000000000000000, -20.00000000000021316, -3.000000000000002665 ) ) ;
#24409 = SURFACE_STYLE_USAGE ( .BOTH. , #13245 ) ;
#24410 = ORIENTED_EDGE ( 'NONE', *, *, #20529, .T. ) ;
#24411 = VECTOR ( 'NONE', #20520, 1000.000000000000000 ) ;
#24412 = CARTESIAN_POINT ( 'NONE',  ( 14.68750000000004796, -0.8284271247460552878, -1.999999999999971800 ) ) ;
#24413 = CARTESIAN_POINT ( 'NONE',  ( -4.999999999999990230, -55.00000000000002132, 8.000000000000007105 ) ) ;
#24414 = STYLED_ITEM ( 'NONE', ( #469 ), #24241 ) ;
#24415 = CARTESIAN_POINT ( 'NONE',  ( 134.7976497308104058, 0.000000000000000000, 5.000000000000004441 ) ) ;
#24416 = CARTESIAN_POINT ( 'NONE',  ( 7.216878364870455975, -6.409875621278545621E-14, -70.44198729810780435 ) ) ;
#24417 = CARTESIAN_POINT ( 'NONE',  ( -3.608439182435115633, 6.249999999999965361, -51.94198729810779014 ) ) ;
#24418 = EDGE_CURVE ( 'NONE', #29800, #15916, #28849, .T. ) ;
#24419 = SURFACE_STYLE_FILL_AREA ( #7982 ) ;
#24420 = CARTESIAN_POINT ( 'NONE',  ( -5.196152422706601826, 2.999999999999975131, -102.9613248654052171 ) ) ;
#24421 = DIRECTION ( 'NONE',  ( 1.000000000000000000, -5.551115123125773458E-17, -1.260129944081490338E-35 ) ) ;
#24422 = CARTESIAN_POINT ( 'NONE',  ( 4.763139720814407951, 2.750000000000002665, -126.2500000000000284 ) ) ;
#24423 = FILL_AREA_STYLE_COLOUR ( '', #3375 ) ;
#24424 = EDGE_LOOP ( 'NONE', ( #6271, #12445, #27455, #26649 ) ) ;
#24425 = DIRECTION ( 'NONE',  ( 1.000000000000000000, -5.551115123125773458E-17, -1.260129944081490338E-35 ) ) ;
#24426 = CARTESIAN_POINT ( 'NONE',  ( 153.4613248654052029, -5.500000000000005329, 0.000000000000000000 ) ) ;
#24427 = DIRECTION ( 'NONE',  ( 0.000000000000000000, 0.000000000000000000, 1.000000000000000000 ) ) ;
#24428 = ADVANCED_FACE ( 'NONE', ( #12714 ), #24048, .T. ) ;
#24429 = ORIENTED_EDGE ( 'NONE', *, *, #11831, .T. ) ;
#24430 = CARTESIAN_POINT ( 'NONE',  ( 112.4997167782373992, 1.308140751793751555, -1.308140751793640533 ) ) ;
#24431 = CARTESIAN_POINT ( 'NONE',  ( 135.9375000000000568, -4.242640687119298093, -4.242640687119298093 ) ) ;
#24432 = CARTESIAN_POINT ( 'NONE',  ( 2.775557561562891351E-14, 6.250000000000033751, -98.56698729810780435 ) ) ;
#24433 = CARTESIAN_POINT ( 'NONE',  ( 20.83632486540534856, 1.767766952966487448, 1.767766952966209892 ) ) ;
#24434 = CARTESIAN_POINT ( 'NONE',  ( 112.9999999999998579, 2.500000000000057732, 0.000000000000000000 ) ) ;
#24435 = CARTESIAN_POINT ( 'NONE',  ( -6.000000000000000888, 1.067854986875958443E-15, 7.560779664488942560E-35 ) ) ;
#24436 = CARTESIAN_POINT ( 'NONE',  ( 0.000000000000000000, 5.999999999999977796, -77.71132486540521711 ) ) ;
#24437 = ORIENTED_EDGE ( 'NONE', *, *, #4350, .T. ) ;
#24438 = CARTESIAN_POINT ( 'NONE',  ( 160.3057606286754435, -11.25150511129604780, 4.172711468660709855 ) ) ;
#24439 = CARTESIAN_POINT ( 'NONE',  ( 3.175426480543072749, -5.500000000000105693, -53.12500000000002842 ) ) ;
#24440 = CARTESIAN_POINT ( 'NONE',  ( 6.000000000000000888, -1.859271017917181981E-14, -59.16367513459483263 ) ) ;
#24441 = CARTESIAN_POINT ( 'NONE',  ( 3.608439182435180470, 6.249999999999982236, -74.05801270189222407 ) ) ;
#24442 =( BOUNDED_CURVE ( )  B_SPLINE_CURVE ( 2, ( #20111, #27152, #28997, #3649, #26996, #15538, #29146, #24706, #3052 ),
 .UNSPECIFIED., .F., .T. ) 
 B_SPLINE_CURVE_WITH_KNOTS ( ( 3, 2, 2, 2, 3 ),
 ( 0.2647058823529411797, 0.2720588235294117418, 0.2794117647058823595, 0.2867647058823529216, 0.2941176470588235392 ),
 .UNSPECIFIED. ) 
 CURVE ( )  GEOMETRIC_REPRESENTATION_ITEM ( )  RATIONAL_B_SPLINE_CURVE ( ( 1.000000000000000000, 0.9238795325112867385, 1.000000000000000000, 0.9238795325112867385, 1.000000000000000000, 0.9238795325112867385, 1.000000000000000000, 0.9238795325112867385, 1.000000000000000000 ) ) 
 REPRESENTATION_ITEM ( '' )  );
#24443 = CARTESIAN_POINT ( 'NONE',  ( 116.2738248654050750, -2.000000000000001776, -0.8284271247461753029 ) ) ;
#24444 = CARTESIAN_POINT ( 'NONE',  ( 155.7976497308104342, 0.000000000000000000, 5.000000000000004441 ) ) ;
#24445 = DIRECTION ( 'NONE',  ( -7.147005652999508048E-36, 5.642372883946980038E-36, 1.000000000000000000 ) ) ;
#24446 = EDGE_CURVE ( 'NONE', #4859, #14973, #16662, .T. ) ;
#24447 = CARTESIAN_POINT ( 'NONE',  ( -3.464101615137725076, 5.999999999999979572, -79.66367513459485394 ) ) ;
#24448 = FACE_OUTER_BOUND ( 'NONE', #12488, .T. ) ;
#24449 = CARTESIAN_POINT ( 'NONE',  ( 3.175426480543072749, -5.500000000000105693, -132.6250000000000284 ) ) ;
#24450 = CARTESIAN_POINT ( 'NONE',  ( 6.000000000000000888, -1.607695154586752384, -177.1533121635130499 ) ) ;
#24451 = CARTESIAN_POINT ( 'NONE',  ( -5.999999999999956479, -1.607695154586745057, -71.26933756729742697 ) ) ;
#24452 = CARTESIAN_POINT ( 'NONE',  ( -3.175426480542816066, 5.499999999999865885, -64.37500000000001421 ) ) ;
#24453 = ADVANCED_FACE ( 'NONE', ( #3140 ), #26221, .T. ) ;
#24454 = CARTESIAN_POINT ( 'NONE',  ( 6.350852961086080661, -9.614813431917819062E-14, -57.37500000000004974 ) ) ;
#24455 = CYLINDRICAL_SURFACE ( 'NONE', #10165, 1.000000000000000888 ) ;
#24456 = EDGE_LOOP ( 'NONE', ( #10919, #13849, #22085, #5346 ) ) ;
#24457 = CARTESIAN_POINT ( 'NONE',  ( 151.3125000000000568, 4.242640687119298093, -4.242640687119298093 ) ) ;
#24458 = CARTESIAN_POINT ( 'NONE',  ( 6.000000000000000888, 1.743066579297358182E-13, -102.6636751345948397 ) ) ;
#24459 = CARTESIAN_POINT ( 'NONE',  ( 15.18750000000007105, 0.8284271247462955401, 1.999999999999851674 ) ) ;
#24460 = LINE ( 'NONE', #2969, #15613 ) ;
#24461 = CARTESIAN_POINT ( 'NONE',  ( 112.4997167782373992, 1.308140751793751555, -1.308140751793640533 ) ) ;
#24462 = ORIENTED_EDGE ( 'NONE', *, *, #977, .F. ) ;
#24463 = CARTESIAN_POINT ( 'NONE',  ( 146.2500000000000568, -6.000000000000005329, 0.000000000000000000 ) ) ;
#24464 = CARTESIAN_POINT ( 'NONE',  ( 161.2222053800996093, -4.042477648134306101, 4.062297615371217141 ) ) ;
#24465 = ORIENTED_EDGE ( 'NONE', *, *, #4660, .F. ) ;
#24466 = COLOUR_RGB ( '', 0.72549020, 0.75294118, 0.79215686) ;
#24467 = CARTESIAN_POINT ( 'NONE',  ( -4.763139720814407951, -2.750000000000016431, -148.0000000000000284 ) ) ;
#24468 = CARTESIAN_POINT ( 'NONE',  ( 15.43750000000009770, -1.999999999999851674, 0.8284271247462354770 ) ) ;
#24469 = ORIENTED_EDGE ( 'NONE', *, *, #11942, .F. ) ;
#24470 = CARTESIAN_POINT ( 'NONE',  ( -3.608439182435115633, 6.249999999999965361, -144.9419872981078470 ) ) ;
#24471 = CARTESIAN_POINT ( 'NONE',  ( -6.350852961085760029, -1.281975124255709124E-13, -77.62500000000001421 ) ) ;
#24472 = B_SPLINE_CURVE_WITH_KNOTS ( 'NONE', 3,
 ( #8128, #19677, #1076, #10466, #24570, #3519, #12949, #29326, #10389, #28630, #19741, #17616, #2995, #5441, #22205, #17317, #10539, #842 ),
 .UNSPECIFIED., .F., .F.,
 ( 4, 2, 2, 2, 2, 2, 2, 2, 4 ),
 ( 0.006357437601277660111, 0.007224154817333453514, 0.008090872033389246917, 0.008957589249445039453, 0.009824306465500833724, 0.01069102368155662626, 0.01155774089761241880, 0.01242445811366821307, 0.01329117532972400560 ),
 .UNSPECIFIED. ) ;
#24473 = CARTESIAN_POINT ( 'NONE',  ( 14.25000000000009592, 1.873492889145067508, -1.873492889144956486 ) ) ;
#24474 = CARTESIAN_POINT ( 'NONE',  ( -5.412658773652684552, -3.125000000000099920, -94.43301270189225249 ) ) ;
#24475 = ORIENTED_EDGE ( 'NONE', *, *, #19654, .F. ) ;
#24476 = CARTESIAN_POINT ( 'NONE',  ( -5.196152422706573404, -3.000000000000002665, -128.2113248654052029 ) ) ;
#24477 = EDGE_CURVE ( 'NONE', #18130, #22143, #22912, .T. ) ;
#24478 = FACE_OUTER_BOUND ( 'NONE', #2501, .T. ) ;
#24479 = CARTESIAN_POINT ( 'NONE',  ( 148.2113248654052313, 5.500000000000005329, 0.000000000000000000 ) ) ;
#24480 = DIRECTION ( 'NONE',  ( 1.000000000000000000, 0.000000000000000000, 0.000000000000000000 ) ) ;
#24481 = SURFACE_SIDE_STYLE ('',( #13016 ) ) ;
#24482 = CARTESIAN_POINT ( 'NONE',  ( 3.175426480543072749, 5.499999999999865885, -156.1250000000000000 ) ) ;
#24483 = CARTESIAN_POINT ( 'NONE',  ( 17.96132486540527751, 1.110223024625156540E-13, 2.499999999999946709 ) ) ;
#24484 = CARTESIAN_POINT ( 'NONE',  ( -3.175426480542816510, -5.500000000000057732, -149.3750000000000284 ) ) ;
#24485 = CARTESIAN_POINT ( 'NONE',  ( 116.7886751345947687, -2.000000000000001776, 0.000000000000000000 ) ) ;
#24486 = AXIS2_PLACEMENT_3D ( 'NONE', #11353, #10892, #20699 ) ;
#24487 = CARTESIAN_POINT ( 'NONE',  ( -3.175426480542816066, 5.499999999999865885, -92.87500000000002842 ) ) ;
#24488 = CARTESIAN_POINT ( 'NONE',  ( 140.3363248654052029, 0.000000000000000000, -5.500000000000005329 ) ) ;
#24489 = ADVANCED_FACE ( 'NONE', ( #28788 ), #14702, .T. ) ;
#24490 = CARTESIAN_POINT ( 'NONE',  ( 4.763139720814407951, -2.749999999999988454, -78.50000000000001421 ) ) ;
#24491 = CIRCLE ( 'NONE', #12294, 30.00000000000000000 ) ;
#24492 = CARTESIAN_POINT ( 'NONE',  ( 152.0773502691896510, 5.000000000000004441, 0.000000000000000000 ) ) ;
#24493 = CARTESIAN_POINT ( 'NONE',  ( 150.6636751345948255, 0.000000000000000000, 5.500000000000005329 ) ) ;
#24494 = CARTESIAN_POINT ( 'NONE',  ( 139.5985279861999686, -9.179712423653196396, -7.992169671736488290 ) ) ;
#24495 = AXIS2_PLACEMENT_3D ( 'NONE', #18009, #1838, #6289 ) ;
#24496 = CARTESIAN_POINT ( 'NONE',  ( 21.37500000000011724, -1.414213562373090038, 1.414213562373034527 ) ) ;
#24497 = PRESENTATION_LAYER_ASSIGNMENT (  '', '', ( #18668 ) ) ;
#24498 = CARTESIAN_POINT ( 'NONE',  ( -5.196152422706573404, -3.000000000000002665, -165.7113248654051745 ) ) ;
#24499 = CARTESIAN_POINT ( 'NONE',  ( 150.6488248654052029, -3.889087296526011706, -3.889087296526011706 ) ) ;
#24500 = CARTESIAN_POINT ( 'NONE',  ( -5.999999999999963585, -1.487416814333745711E-14, -138.8363248654052597 ) ) ;
#24501 = ORIENTED_EDGE ( 'NONE', *, *, #3958, .F. ) ;
#24502 = CARTESIAN_POINT ( 'NONE',  ( -5.999999999999963585, 3.021315404115421074E-15, -178.4136751345948255 ) ) ;
#24503 = CARTESIAN_POINT ( 'NONE',  ( -5.196152422706573404, -3.000000000000002665, -157.2886751345948824 ) ) ;
#24504 = CARTESIAN_POINT ( 'NONE',  ( 120.6877832217621176, -0.7662911109077388261, 1.849990392679652151 ) ) ;
#24505 = CARTESIAN_POINT ( 'NONE',  ( 0.000000000000000000, -5.999999999999991118, -115.9613248654052313 ) ) ;
#24506 = ORIENTED_EDGE ( 'NONE', *, *, #1550, .F. ) ;
#24507 = ORIENTED_EDGE ( 'NONE', *, *, #6658, .T. ) ;
#24508 = CARTESIAN_POINT ( 'NONE',  ( 0.000000000000000000, 5.499999999999991118, -102.0000000000000284 ) ) ;
#24509 = CYLINDRICAL_SURFACE ( 'NONE', #9703, 6.000000000000000888 ) ;
#24510 = CARTESIAN_POINT ( 'NONE',  ( -3.608439182435052128, -6.250000000000110134, -112.3080127018922241 ) ) ;
#24511 = ORIENTED_EDGE ( 'NONE', *, *, #12480, .F. ) ;
#24512 = CARTESIAN_POINT ( 'NONE',  ( 5.196152422706629359, 3.000000000000002665, -111.5386751345948113 ) ) ;
#24513 = TOROIDAL_SURFACE ( 'NONE', #29917, 15.99999999999999289, 1.000000000000000000 ) ;
#24514 = CARTESIAN_POINT ( 'NONE',  ( 135.0000000000000284, -6.982120021884474781, 8.500000000000007105 ) ) ;
#24515 = CARTESIAN_POINT ( 'NONE',  ( 15.03867513459491967, 1.665334536937734811E-13, -2.500000000000057732 ) ) ;
#24516 = EDGE_CURVE ( 'NONE', #3348, #10268, #10242, .T. ) ;
#24517 = CARTESIAN_POINT ( 'NONE',  ( 2.775557561562891351E-14, 6.250000000000033751, -54.43301270189226670 ) ) ;
#24518 = ORIENTED_EDGE ( 'NONE', *, *, #6714, .F. ) ;
#24519 = EDGE_CURVE ( 'NONE', #22378, #16791, #11360, .T. ) ;
#24520 = CARTESIAN_POINT ( 'NONE',  ( 6.000000000000026645, -1.607695154586707753, -119.2306624327025872 ) ) ;
#24521 = CARTESIAN_POINT ( 'NONE',  ( -3.464101615137725076, 5.999999999999979572, -136.0863248654051745 ) ) ;
#24522 = FACE_OUTER_BOUND ( 'NONE', #21816, .T. ) ;
#24523 = CARTESIAN_POINT ( 'NONE',  ( -4.763139720814407951, -2.750000000000016431, -167.4999999999999716 ) ) ;
#24524 = CARTESIAN_POINT ( 'NONE',  ( 118.6874999999998295, -1.035533905932719101, -2.499999999999844569 ) ) ;
#24525 = CARTESIAN_POINT ( 'NONE',  ( 7.216878364870455975, -6.409875621278545621E-14, -170.3080127018922667 ) ) ;
#24526 = CARTESIAN_POINT ( 'NONE',  ( -5.999999999999919176, 1.607695154586804565, -47.98066243270260856 ) ) ;
#24527 = CARTESIAN_POINT ( 'NONE',  ( 24.31250000000015277, -0.8284271247461153509, 2.000000000000031530 ) ) ;
#24528 = CARTESIAN_POINT ( 'NONE',  ( 0.000000000000000000, 5.499999999999991118, -120.0000000000000000 ) ) ;
#24529 = CARTESIAN_POINT ( 'NONE',  ( 23.46132486540525264, 1.110223024625156540E-13, -2.500000000000002220 ) ) ;
#24530 =( BOUNDED_CURVE ( )  B_SPLINE_CURVE ( 2, ( #21952, #2599, #2739, #12166, #24093, #5040, #885, #28836, #16773 ),
 .UNSPECIFIED., .F., .T. ) 
 B_SPLINE_CURVE_WITH_KNOTS ( ( 3, 2, 2, 2, 3 ),
 ( 0.5972222222222222099, 0.5981481481481480955, 0.5999999999999999778, 0.6018518518518518601, 0.6027777777777777457 ),
 .UNSPECIFIED. ) 
 CURVE ( )  GEOMETRIC_REPRESENTATION_ITEM ( )  RATIONAL_B_SPLINE_CURVE ( ( 0.9330127018922194093, 0.9330127018922194093, 1.000000000000000000, 0.8660254037844388186, 1.000000000000000000, 0.8660254037844388186, 1.000000000000000000, 0.9330127018922234061, 0.9330127018922194093 ) ) 
 REPRESENTATION_ITEM ( '' )  );
#24531 = CARTESIAN_POINT ( 'NONE',  ( 0.000000000000000000, 5.499999999999991118, -102.0000000000000284 ) ) ;
#24532 = CARTESIAN_POINT ( 'NONE',  ( 135.0000000000000284, -9.047800747817580813, -7.500000000000007105 ) ) ;
#24533 = CARTESIAN_POINT ( 'NONE',  ( 6.000000000000000888, 1.743066579297358182E-13, -111.6636751345948255 ) ) ;
#24534 = CARTESIAN_POINT ( 'NONE',  ( 16.33632486540528816, -1.767766952966209892, -1.767766952966487448 ) ) ;
#24535 = CARTESIAN_POINT ( 'NONE',  ( 0.000000000000000000, -5.999999999999991118, -84.46132486540524553 ) ) ;
#24536 = VERTEX_POINT ( 'NONE', #13627 ) ;
#24537 = CARTESIAN_POINT ( 'NONE',  ( 15.31250000000012967, -1.097466725451379244, -2.649519052838358757 ) ) ;
#24538 = CARTESIAN_POINT ( 'NONE',  ( 118.9999999999998437, 2.500000000000057732, 2.220446049250313081E-13 ) ) ;
#24539 = TOROIDAL_SURFACE ( 'NONE', #18707, 6.000000000000000000, 5.000000000000004441 ) ;
#24540 = AXIS2_PLACEMENT_3D ( 'NONE', #19080, #23527, #18935 ) ;
#24541 = ORIENTED_EDGE ( 'NONE', *, *, #1092, .T. ) ;
#24542 = CARTESIAN_POINT ( 'NONE',  ( -3.175426480542816510, 5.499999999999865885, -161.8750000000000568 ) ) ;
#24543 = CARTESIAN_POINT ( 'NONE',  ( 139.1175748654052029, 5.500000000000012434, -2.278174593052012309 ) ) ;
#24544 = CARTESIAN_POINT ( 'NONE',  ( 7.216878364870455975, -6.409875621278545621E-14, -77.94198729810779014 ) ) ;
#24545 = CARTESIAN_POINT ( 'NONE',  ( -3.464101615137757051, -5.999999999999979572, -129.5863248654052029 ) ) ;
#24546 = EDGE_LOOP ( 'NONE', ( #15381, #1787, #13961, #10832 ) ) ;
#24547 = CARTESIAN_POINT ( 'NONE',  ( -5.196152422706601826, 2.999999999999975131, -144.0386751345948539 ) ) ;
#24548 = ORIENTED_EDGE ( 'NONE', *, *, #3648, .T. ) ;
#24549 = ORIENTED_EDGE ( 'NONE', *, *, #13108, .F. ) ;
#24550 = CARTESIAN_POINT ( 'NONE',  ( 155.1562500000000284, -6.000000000000005329, 2.485281374238555774 ) ) ;
#24551 = CARTESIAN_POINT ( 'NONE',  ( -3.608439182435052128, -6.250000000000110134, -136.3080127018922667 ) ) ;
#24552 = ORIENTED_EDGE ( 'NONE', *, *, #23724, .T. ) ;
#24553 = CARTESIAN_POINT ( 'NONE',  ( 5.412658773652739619, 3.124999999999988898, -127.3169872981078043 ) ) ;
#24554 = CARTESIAN_POINT ( 'NONE',  ( -4.763139720814407951, -2.750000000000016431, -175.0000000000000568 ) ) ;
#24555 = CARTESIAN_POINT ( 'NONE',  ( -3.464101615137757051, -5.999999999999979572, -167.6636751345948255 ) ) ;
#24556 = CARTESIAN_POINT ( 'NONE',  ( -10.00000000000000178, -19.99999999999998934, -3.000000000000002665 ) ) ;
#24557 = AXIS2_PLACEMENT_3D ( 'NONE', #9927, #1130, #5735 ) ;
#24558 = ORIENTED_EDGE ( 'NONE', *, *, #9259, .T. ) ;
#24559 = CARTESIAN_POINT ( 'NONE',  ( 15.12500000000000000, 1.414213562373201061, 1.414213562373034527 ) ) ;
#24560 = CARTESIAN_POINT ( 'NONE',  ( -5.999999999999963585, -1.487416814333745711E-14, -171.8363248654052313 ) ) ;
#24561 = DIRECTION ( 'NONE',  ( 1.000000000000000000, -5.551115123125773458E-17, -1.260129944081490338E-35 ) ) ;
#24562 = EDGE_CURVE ( 'NONE', #26257, #14826, #27379, .T. ) ;
#24563 =( GEOMETRIC_REPRESENTATION_CONTEXT ( 3 ) GLOBAL_UNCERTAINTY_ASSIGNED_CONTEXT ( ( #19896 ) ) GLOBAL_UNIT_ASSIGNED_CONTEXT ( ( #13024, #13187, #3754 ) ) REPRESENTATION_CONTEXT ( 'NONE', 'WORKASPACE' ) );
#24564 = DIRECTION ( 'NONE',  ( 0.000000000000000000, 0.000000000000000000, 1.000000000000000000 ) ) ;
#24565 = CARTESIAN_POINT ( 'NONE',  ( -3.464101615137757051, -5.999999999999979572, -107.6636751345948539 ) ) ;
#24566 = DIRECTION ( 'NONE',  ( -0.000000000000000000, -0.000000000000000000, -1.000000000000000000 ) ) ;
#24567 = CARTESIAN_POINT ( 'NONE',  ( 2.775557561562891351E-14, 6.250000000000033751, -67.06698729810783277 ) ) ;
#24568 = CARTESIAN_POINT ( 'NONE',  ( 3.608439182435180470, -6.249999999999997335, -54.19198729810779724 ) ) ;
#24569 = CARTESIAN_POINT ( 'NONE',  ( 161.0000000000000284, -11.67610212985248452, 2.769230769230773603 ) ) ;
#24570 = CARTESIAN_POINT ( 'NONE',  ( 135.0000000000000284, 3.276830707260631304, 4.562445581355718538 ) ) ;
#24571 = FACE_OUTER_BOUND ( 'NONE', #6124, .T. ) ;
#24572 = CARTESIAN_POINT ( 'NONE',  ( 3.464101615137852974, 5.999999999999884537, -127.9136751345948113 ) ) ;
#24573 = CARTESIAN_POINT ( 'NONE',  ( 0.000000000000000000, 5.499999999999991118, -126.0000000000000000 ) ) ;
#24574 = CARTESIAN_POINT ( 'NONE',  ( 108.7113248654051176, 2.000000000000057288, 0.000000000000000000 ) ) ;
#24575 = EDGE_LOOP ( 'NONE', ( #2294, #13166, #8105, #20612 ) ) ;
#24576 = CARTESIAN_POINT ( 'NONE',  ( 24.43750000000014921, 1.097466725451679892, -2.649519052838298805 ) ) ;
#24577 = CARTESIAN_POINT ( 'NONE',  ( -5.196152422706601826, 2.999999999999975131, -119.4613248654052313 ) ) ;
#24578 = CARTESIAN_POINT ( 'NONE',  ( 5.196152422706629359, 3.000000000000002665, -97.46132486540525974 ) ) ;
#24579 = CARTESIAN_POINT ( 'NONE',  ( 0.000000000000000000, -5.999999999999991118, -100.0386751345948539 ) ) ;
#24580 = CARTESIAN_POINT ( 'NONE',  ( 5.196152422706629359, -2.999999999999988898, -144.2113248654052313 ) ) ;
#24581 = ORIENTED_EDGE ( 'NONE', *, *, #13835, .T. ) ;
#24582 = CARTESIAN_POINT ( 'NONE',  ( 112.6247167782375271, 1.849990392679523588, 0.000000000000000000 ) ) ;
#24583 = CARTESIAN_POINT ( 'NONE',  ( 5.412658773652712085, -3.125000000000086153, -94.56698729810780435 ) ) ;
#24584 = AXIS2_PLACEMENT_3D ( 'NONE', #20248, #3624, #24833 ) ;
#24585 = CARTESIAN_POINT ( 'NONE',  ( -5.999999999999963585, -1.487416814333745711E-14, -54.83632486540523132 ) ) ;
#24586 = CARTESIAN_POINT ( 'NONE',  ( 155.5386751345948539, -5.500000000000005329, 0.000000000000000000 ) ) ;
#24587 = CARTESIAN_POINT ( 'NONE',  ( 112.2499999999998153, -5.551115123125782702E-14, 2.500000000000168754 ) ) ;
#24588 = CARTESIAN_POINT ( 'NONE',  ( 141.0000000000000284, -12.00000000000001066, 4.000000000000003553 ) ) ;
#24589 = EDGE_CURVE ( 'NONE', #17182, #20541, #4052, .T. ) ;
#24590 = VERTEX_POINT ( 'NONE', #22815 ) ;
#24592 = CARTESIAN_POINT ( 'NONE',  ( 136.5863248654052313, 0.000000000000000000, 5.500000000000005329 ) ) ;
#24591 = VECTOR ( 'NONE', #14243, 1000.000000000000000 ) ;
#24593 = CARTESIAN_POINT ( 'NONE',  ( -4.763139720814407951, 2.749999999999946709, -52.25000000000002132 ) ) ;
#24594 = CARTESIAN_POINT ( 'NONE',  ( 6.000000000000000888, -1.607695154586752384, -59.23066243270262277 ) ) ;
#24595 = CARTESIAN_POINT ( 'NONE',  ( 6.000000000000000888, 1.743066579297358182E-13, -62.16367513459481131 ) ) ;
#24596 = CARTESIAN_POINT ( 'NONE',  ( -7.216878364870328078, 0.000000000000000000, -72.05801270189223828 ) ) ;
#24597 = ADVANCED_FACE ( 'NONE', ( #22520 ), #17928, .F. ) ;
#24598 = CARTESIAN_POINT ( 'NONE',  ( -5.999999999999964473, 9.063946212346262433E-15, -173.3363248654052597 ) ) ;
#24599 = CARTESIAN_POINT ( 'NONE',  ( 151.9538997308104058, -2.071067811865468400, -4.999999999999989342 ) ) ;
#24600 = CARTESIAN_POINT ( 'NONE',  ( 0.000000000000000000, 0.000000000000000000, 0.000000000000000000 ) ) ;
#24601 = CARTESIAN_POINT ( 'NONE',  ( 0.000000000000000000, 0.000000000000000000, 0.000000000000000000 ) ) ;
#24602 = CARTESIAN_POINT ( 'NONE',  ( -5.999999999999962697, 3.323446944526963891E-14, -152.9136751345948255 ) ) ;
#24603 = AXIS2_PLACEMENT_3D ( 'NONE', #15509, #15030, #22088 ) ;
#24604 = CARTESIAN_POINT ( 'NONE',  ( 0.000000000000000000, 5.499999999999991118, -132.0000000000000000 ) ) ;
#24605 = CARTESIAN_POINT ( 'NONE',  ( 10.10117513459485217, 1.035533905932809473, -2.499999999999904521 ) ) ;
#24606 = CYLINDRICAL_SURFACE ( 'NONE', #17008, 6.000000000000000888 ) ;
#24607 = CARTESIAN_POINT ( 'NONE',  ( -5.196152422706601826, 2.999999999999975131, -177.9613248654052313 ) ) ;
#24608 = VERTEX_POINT ( 'NONE', #15941 ) ;
#24609 = CARTESIAN_POINT ( 'NONE',  ( -3.175426480542816066, -5.500000000000057732, -66.87500000000002842 ) ) ;
#24610 = CARTESIAN_POINT ( 'NONE',  ( -3.175426480542816510, 5.499999999999865885, -59.87500000000005684 ) ) ;
#24611 = FILL_AREA_STYLE_COLOUR ( '', #17521 ) ;
#24612 = ORIENTED_EDGE ( 'NONE', *, *, #20191, .F. ) ;
#24613 = CARTESIAN_POINT ( 'NONE',  ( 144.0000000000000284, 6.000000000000005329, 0.000000000000000000 ) ) ;
#24614 = CARTESIAN_POINT ( 'NONE',  ( 141.7574251345948255, -2.278174593051702335, 5.500000000000323297 ) ) ;
#24615 = CARTESIAN_POINT ( 'NONE',  ( 15.62500000000013856, -1.414213562372979016, -1.414213562373145550 ) ) ;
#24616 = AXIS2_PLACEMENT_3D ( 'NONE', #24779, #13301, #18057 ) ;
#24617 = ADVANCED_BREP_SHAPE_REPRESENTATION ( '', ( #14219, #18805 ), #1104 ) ;
#24618 = CARTESIAN_POINT ( 'NONE',  ( 110.8747167782375556, 0.000000000000000000, 1.849990392679523588 ) ) ;
#24619 = ORIENTED_EDGE ( 'NONE', *, *, #16161, .F. ) ;
#24620 = CARTESIAN_POINT ( 'NONE',  ( 146.9062500000000284, 6.000000000000005329, -2.485281374238555774 ) ) ;
#24621 = CARTESIAN_POINT ( 'NONE',  ( 143.0550748654052313, -5.500000000000012434, -2.278174593052012309 ) ) ;
#24622 = EDGE_CURVE ( 'NONE', #9799, #2895, #25238, .T. ) ;
#24623 = EDGE_LOOP ( 'NONE', ( #5540, #1934, #30352, #25420 ) ) ;
#24624 = ADVANCED_FACE ( 'NONE', ( #8521 ), #1914, .T. ) ;
#24625 = CARTESIAN_POINT ( 'NONE',  ( -3.175426480542816510, 5.499999999999865885, -143.8750000000000000 ) ) ;
#24626 =( BOUNDED_CURVE ( )  B_SPLINE_CURVE ( 2, ( #549, #9938, #10246, #5594, #19314, #28634, #7605, #17018, #2997 ),
 .UNSPECIFIED., .F., .T. ) 
 B_SPLINE_CURVE_WITH_KNOTS ( ( 3, 2, 2, 2, 3 ),
 ( 0.5861111111111111382, 0.5870370370370370239, 0.5888888888888889062, 0.5907407407407407884, 0.5916666666666666741 ),
 .UNSPECIFIED. ) 
 CURVE ( )  GEOMETRIC_REPRESENTATION_ITEM ( )  RATIONAL_B_SPLINE_CURVE ( ( 0.9330127018922194093, 0.9330127018922194093, 1.000000000000000000, 0.8660254037844388186, 1.000000000000000000, 0.8660254037844388186, 1.000000000000000000, 0.9330127018922194093, 0.9330127018922194093 ) ) 
 REPRESENTATION_ITEM ( '' )  );
#24627 = CARTESIAN_POINT ( 'NONE',  ( 19.12500000000014211, 1.414213562373256572, 1.414213562373034527 ) ) ;
#24628 = ORIENTED_EDGE ( 'NONE', *, *, #6987, .T. ) ;
#24629 = CARTESIAN_POINT ( 'NONE',  ( 3.608439182435180470, 6.249999999999982236, -149.6919872981077901 ) ) ;
#24630 = CARTESIAN_POINT ( 'NONE',  ( 4.763139720814407951, 2.750000000000002665, -70.75000000000002842 ) ) ;
#24631 = CARTESIAN_POINT ( 'NONE',  ( 14.06249999999999645, -1.097466725451439196, -2.649519052838478661 ) ) ;
#24632 = EDGE_CURVE ( 'NONE', #5384, #19330, #4851, .T. ) ;
#24633 = CARTESIAN_POINT ( 'NONE',  ( -7.216878364870328078, 0.000000000000000000, -94.55801270189226670 ) ) ;
#24634 = EDGE_CURVE ( 'NONE', #29849, #2905, #14983, .T. ) ;
#24635 = CARTESIAN_POINT ( 'NONE',  ( 10.56250000000007461, -1.999999999999971800, -0.8284271247462354770 ) ) ;
#24636 = ORIENTED_EDGE ( 'NONE', *, *, #18530, .F. ) ;
#24637 = CARTESIAN_POINT ( 'NONE',  ( -4.767949350811372611, -9.915884935901891239, -28.66271918150853537 ) ) ;
#24638 = CARTESIAN_POINT ( 'NONE',  ( 0.000000000000000000, 0.000000000000000000, 0.000000000000000000 ) ) ;
#24639 = DIRECTION ( 'NONE',  ( 1.000000000000000000, -0.000000000000000000, -0.000000000000000000 ) ) ;
#24640 = CARTESIAN_POINT ( 'NONE',  ( -5.999999999999963585, 8.134310703387671600E-14, -131.9136751345948255 ) ) ;
#24641 = SURFACE_SIDE_STYLE ('',( #1288 ) ) ;
#24642 = CARTESIAN_POINT ( 'NONE',  ( -2.775557561562891351E-14, -5.500000000000115463, -155.2500000000000000 ) ) ;
#24643 = CARTESIAN_POINT ( 'NONE',  ( 117.8988248654050750, 0.8284271247462354770, 2.000000000000212275 ) ) ;
#24644 = CARTESIAN_POINT ( 'NONE',  ( 4.763139720814407951, -2.749999999999988454, -143.0000000000000284 ) ) ;
#24645 = CARTESIAN_POINT ( 'NONE',  ( 19.64882486540529882, 2.500000000000144773, -1.035533905932689347 ) ) ;
#24646 = CARTESIAN_POINT ( 'NONE',  ( -4.763139720814407951, -2.750000000000016431, -83.50000000000001421 ) ) ;
#24647 = CARTESIAN_POINT ( 'NONE',  ( 0.000000000000000000, 0.000000000000000000, 0.000000000000000000 ) ) ;
#24648 = CARTESIAN_POINT ( 'NONE',  ( 0.000000000000000000, 0.000000000000000000, 0.000000000000000000 ) ) ;
#24649 = CARTESIAN_POINT ( 'NONE',  ( -3.175426480542816510, -5.500000000000057732, -78.87500000000002842 ) ) ;
#24650 = CARTESIAN_POINT ( 'NONE',  ( 3.464101615137757051, -5.999999999999979572, -74.41367513459483973 ) ) ;
#24651 = CARTESIAN_POINT ( 'NONE',  ( 154.7023502691896510, 0.000000000000000000, -5.000000000000004441 ) ) ;
#24652 = CARTESIAN_POINT ( 'NONE',  ( 5.999999999999949374, 1.607695154586804565, -165.0193375672974128 ) ) ;
#24653 = CARTESIAN_POINT ( 'NONE',  ( -5.999999999999963585, 1.780251999655701777E-13, -108.8363248654052313 ) ) ;
#24654 = CARTESIAN_POINT ( 'NONE',  ( -5.196152422706573404, -3.000000000000002665, -149.7886751345948255 ) ) ;
#24655 = LINE ( 'NONE', #3602, #6018 ) ;
#24656 = CARTESIAN_POINT ( 'NONE',  ( 3.464101615137852974, 5.999999999999884537, -134.8363248654052313 ) ) ;
#24657 = DIRECTION ( 'NONE',  ( 1.000000000000000000, -5.551115123125782702E-17, 0.000000000000000000 ) ) ;
#24658 = VECTOR ( 'NONE', #8873, 1000.000000000000000 ) ;
#24659 = ORIENTED_EDGE ( 'NONE', *, *, #4249, .F. ) ;
#24660 =( NAMED_UNIT ( * ) PLANE_ANGLE_UNIT ( ) SI_UNIT ( $, .RADIAN. ) );
#24661 = CARTESIAN_POINT ( 'NONE',  ( 6.000000000000000888, 1.743066579297358182E-13, -56.16367513459481842 ) ) ;
#24662 = CARTESIAN_POINT ( 'NONE',  ( 109.8511751345945839, -1.999999999999941602, -0.8284271247459952248 ) ) ;
#24663 = CARTESIAN_POINT ( 'NONE',  ( 117.0002832217621602, -1.308140751793557266, -1.308140751793529510 ) ) ;
#24664 = EDGE_CURVE ( 'NONE', #10035, #10886, #25681, .T. ) ;
#24665 = CARTESIAN_POINT ( 'NONE',  ( -1.110223024625164676E-16, 2.000000000000012879, 2.021286199229734960E-15 ) ) ;
#24666 = ORIENTED_EDGE ( 'NONE', *, *, #15317, .T. ) ;
#24667 = CARTESIAN_POINT ( 'NONE',  ( 4.763139720814407951, -2.749999999999988454, -99.50000000000002842 ) ) ;
#24668 = DIRECTION ( 'NONE',  ( -1.000000000000000000, -1.665334536937736783E-16, -2.220446049250315546E-16 ) ) ;
#24669 = EDGE_CURVE ( 'NONE', #21789, #6076, #18437, .T. ) ;
#24670 = CARTESIAN_POINT ( 'NONE',  ( 5.412658773652739619, 3.124999999999988898, -116.1830127018922383 ) ) ;
#24671 = CIRCLE ( 'NONE', #25674, 1.000000000000000888 ) ;
#24672 = EDGE_CURVE ( 'NONE', #16270, #4691, #11171, .T. ) ;
#24673 = ORIENTED_EDGE ( 'NONE', *, *, #15664, .F. ) ;
#24674 = CARTESIAN_POINT ( 'NONE',  ( -11.00000000000000000, 1.957734142605923910E-15, -43.99152654425658682 ) ) ;
#24675 = CARTESIAN_POINT ( 'NONE',  ( 135.0000000000000284, -8.656813570721347162, 7.548387214344470131 ) ) ;
#24676 =( BOUNDED_CURVE ( )  B_SPLINE_CURVE ( 2, ( #22236, #1166, #10573, #19926, #29273, #9967, #5178, #23944, #2881 ),
 .UNSPECIFIED., .F., .F. ) 
 B_SPLINE_CURVE_WITH_KNOTS ( ( 3, 2, 2, 2, 3 ),
 ( 0.8972222222222222543, 0.8981481481481481399, 0.9000000000000000222, 0.9018518518518519045, 0.9027777777777777901 ),
 .UNSPECIFIED. ) 
 CURVE ( )  GEOMETRIC_REPRESENTATION_ITEM ( )  RATIONAL_B_SPLINE_CURVE ( ( 0.9330127018922194093, 0.9330127018922234061, 1.000000000000000000, 0.8660254037844388186, 1.000000000000000000, 0.8660254037844388186, 1.000000000000000000, 0.9330127018922194093, 0.9330127018922194093 ) ) 
 REPRESENTATION_ITEM ( '' )  );
#24677 = CARTESIAN_POINT ( 'NONE',  ( 5.412658773652712085, -3.125000000000086153, -48.93301270189220986 ) ) ;
#24678 = ORIENTED_EDGE ( 'NONE', *, *, #22012, .F. ) ;
#24679 = LINE ( 'NONE', #3620, #12290 ) ;
#24680 = CARTESIAN_POINT ( 'NONE',  ( -5.196152422706601826, 2.999999999999975131, -99.03867513459485394 ) ) ;
#24681 = CARTESIAN_POINT ( 'NONE',  ( -6.000000000000000888, 1.067854986875958443E-15, 7.560779664488942560E-35 ) ) ;
#24682 = CARTESIAN_POINT ( 'NONE',  ( 0.7669223171414829565, -15.58766199952932396, -7.954545454545463912 ) ) ;
#24683 = CARTESIAN_POINT ( 'NONE',  ( 0.000000000000000000, 5.499999999999991118, -174.0000000000000568 ) ) ;
#24684 = CARTESIAN_POINT ( 'NONE',  ( 119.1874999999998153, 1.035533905932779275, 2.500000000000205169 ) ) ;
#24685 = CARTESIAN_POINT ( 'NONE',  ( -5.999999999999963585, 1.780251999655701777E-13, -107.3363248654052455 ) ) ;
#24686 = CARTESIAN_POINT ( 'NONE',  ( 5.412658773652739619, 3.124999999999988898, -171.6830127018922383 ) ) ;
#24687 = CARTESIAN_POINT ( 'NONE',  ( -0.02602735246118784845, -9.486986323769393437, 4.738252045315884509 ) ) ;
#24688 = CARTESIAN_POINT ( 'NONE',  ( -2.775557561562891351E-14, -5.500000000000115463, -108.7500000000000142 ) ) ;
#24689 = CYLINDRICAL_SURFACE ( 'NONE', #9509, 6.000000000000000888 ) ;
#24690 = CARTESIAN_POINT ( 'NONE',  ( 0.000000000000000000, 5.499999999999991118, -105.0000000000000426 ) ) ;
#24691 = DIRECTION ( 'NONE',  ( -1.000000000000000000, -1.665334536937736783E-16, -2.220446049250315546E-16 ) ) ;
#24692 = CARTESIAN_POINT ( 'NONE',  ( 3.464101615137852974, 5.999999999999884537, -162.4136751345947971 ) ) ;
#24693 = ORIENTED_EDGE ( 'NONE', *, *, #22793, .F. ) ;
#24694 = CARTESIAN_POINT ( 'NONE',  ( 14.24999999999998579, -1.873492889144900975, -1.873492889144956486 ) ) ;
#24695 = FACE_OUTER_BOUND ( 'NONE', #18739, .T. ) ;
#24696 = CARTESIAN_POINT ( 'NONE',  ( 110.5002832217622881, 1.308140751793668288, 1.308140751793640533 ) ) ;
#24697 = CARTESIAN_POINT ( 'NONE',  ( -0.5000000000000004441, -10.50000000000000888, 8.000000000000007105 ) ) ;
#24698 = CARTESIAN_POINT ( 'NONE',  ( -5.196152422706573404, -3.000000000000002665, -146.2113248654052313 ) ) ;
#24699 = ORIENTED_EDGE ( 'NONE', *, *, #20383, .T. ) ;
#24700 = CARTESIAN_POINT ( 'NONE',  ( 3.175426480543072749, 5.499999999999865885, -162.1250000000000284 ) ) ;
#24701 = AXIS2_PLACEMENT_3D ( 'NONE', #2735, #883, #21800 ) ;
#24702 = CARTESIAN_POINT ( 'NONE',  ( 5.412658773652739619, 3.124999999999988898, -85.31698729810783277 ) ) ;
#24703 = EDGE_CURVE ( 'NONE', #2458, #799, #20979, .T. ) ;
#24704 = CARTESIAN_POINT ( 'NONE',  ( 5.196152422706629359, -2.999999999999988898, -102.7886751345948255 ) ) ;
#24705 = VERTEX_POINT ( 'NONE', #18987 ) ;
#24706 = CARTESIAN_POINT ( 'NONE',  ( 115.7738248654051034, 2.000000000000001776, 0.8284271247463557142 ) ) ;
#24707 = EDGE_LOOP ( 'NONE', ( #9873, #29659, #8309, #5692 ) ) ;
#24708 = CARTESIAN_POINT ( 'NONE',  ( 155.3437500000000284, -6.000000000000005329, -2.485281374238555774 ) ) ;
#24709 = CARTESIAN_POINT ( 'NONE',  ( -2.775557561562891351E-14, -5.500000000000115463, -132.7500000000000284 ) ) ;
#24710 = EDGE_CURVE ( 'NONE', #15017, #13841, #24755, .T. ) ;
#24711 = CARTESIAN_POINT ( 'NONE',  ( 3.608439182435180470, -6.249999999999997335, -136.0580127018922099 ) ) ;
#24712 = ORIENTED_EDGE ( 'NONE', *, *, #1538, .T. ) ;
#24713 = CARTESIAN_POINT ( 'NONE',  ( 5.196152422706629359, -2.999999999999988898, -57.21132486540525264 ) ) ;
#24714 = CARTESIAN_POINT ( 'NONE',  ( -3.608439182435115633, 6.249999999999965361, -120.9419872981077901 ) ) ;
#24715 =( NAMED_UNIT ( * ) PLANE_ANGLE_UNIT ( ) SI_UNIT ( $, .RADIAN. ) );
#24716 = CARTESIAN_POINT ( 'NONE',  ( -3.175426480542816510, -5.500000000000057732, -168.8750000000000568 ) ) ;
#24717 = CARTESIAN_POINT ( 'NONE',  ( 3.464101615137852974, 5.999999999999884537, -175.3363248654051461 ) ) ;
#24718 = CARTESIAN_POINT ( 'NONE',  ( -3.464101615137725076, 5.999999999999979572, -47.58632486540521711 ) ) ;
#24719 = ORIENTED_EDGE ( 'NONE', *, *, #14704, .F. ) ;
#24720 = CARTESIAN_POINT ( 'NONE',  ( 16.31250000000011369, -0.8284271247460552878, 1.999999999999971800 ) ) ;
#24721 = CARTESIAN_POINT ( 'NONE',  ( -5.999999999999962697, 3.323446944526963260E-14, -147.8363248654052313 ) ) ;
#24722 =( BOUNDED_CURVE ( )  B_SPLINE_CURVE ( 2, ( #23086, #11897, #2028, #20780, #9090, #18486, #16200, #25671, #9555 ),
 .UNSPECIFIED., .F., .T. ) 
 B_SPLINE_CURVE_WITH_KNOTS ( ( 3, 2, 2, 2, 3 ),
 ( 0.3250000000000000111, 0.3259259259259259522, 0.3277777777777777790, 0.3296296296296296058, 0.3305555555555555469 ),
 .UNSPECIFIED. ) 
 CURVE ( )  GEOMETRIC_REPRESENTATION_ITEM ( )  RATIONAL_B_SPLINE_CURVE ( ( 0.9330127018922194093, 0.9330127018922194093, 1.000000000000000000, 0.8660254037844388186, 1.000000000000000000, 0.8660254037844388186, 1.000000000000000000, 0.9330127018922194093, 0.9330127018922194093 ) ) 
 REPRESENTATION_ITEM ( '' )  );
#24723 = CARTESIAN_POINT ( 'NONE',  ( 6.000000000000103917, -1.607695154586573416, -117.1533121635129788 ) ) ;
#24724 = FACE_OUTER_BOUND ( 'NONE', #12999, .T. ) ;
#24725 = CARTESIAN_POINT ( 'NONE',  ( 140.0000000000000284, -11.45643923738959202, 5.000000000000004441 ) ) ;
#24726 = CARTESIAN_POINT ( 'NONE',  ( 115.7502832217623308, -1.308140751793585022, 1.308140751793640533 ) ) ;
#24727 = CARTESIAN_POINT ( 'NONE',  ( 2.775557561562891351E-14, -6.250000000000061284, -64.81698729810780435 ) ) ;
#24728 = CARTESIAN_POINT ( 'NONE',  ( 3.608439182435180470, -6.249999999999997335, -52.69198729810779014 ) ) ;
#24729 = CARTESIAN_POINT ( 'NONE',  ( 6.000000000000000888, -1.607695154586752384, -120.7306624327026157 ) ) ;
#24730 = DIRECTION ( 'NONE',  ( 1.000000000000000000, -5.551115123125774690E-17, -1.260129944081490338E-35 ) ) ;
#24731 = CARTESIAN_POINT ( 'NONE',  ( 3.464101615137852974, 5.999999999999884537, -55.91367513459481131 ) ) ;
#24732 = CARTESIAN_POINT ( 'NONE',  ( 6.350852961086080661, -9.614813431917819062E-14, -129.3750000000000284 ) ) ;
#24733 =( BOUNDED_CURVE ( )  B_SPLINE_CURVE ( 2, ( #11722, #20764, #2321, #16336, #9074, #18467, #13727, #8932, #25810 ),
 .UNSPECIFIED., .F., .T. ) 
 B_SPLINE_CURVE_WITH_KNOTS ( ( 3, 2, 2, 2, 3 ),
 ( 0.4416666666666667074, 0.4425925925925925930, 0.4444444444444444198, 0.4462962962962963021, 0.4472222222222221877 ),
 .UNSPECIFIED. ) 
 CURVE ( )  GEOMETRIC_REPRESENTATION_ITEM ( )  RATIONAL_B_SPLINE_CURVE ( ( 0.9330127018922194093, 0.9330127018922214077, 1.000000000000000000, 0.8660254037844388186, 1.000000000000000000, 0.8660254037844388186, 1.000000000000000000, 0.9330127018922214077, 0.9330127018922194093 ) ) 
 REPRESENTATION_ITEM ( '' )  );
#24734 = CARTESIAN_POINT ( 'NONE',  ( -5.999999999999971578, 1.607695154586715303, -50.40331216351300725 ) ) ;
#24735 = CARTESIAN_POINT ( 'NONE',  ( 104.7401757384973564, -0.2415688265503397880, -1.838109686700451384 ) ) ;
#24736 = ORIENTED_EDGE ( 'NONE', *, *, #29228, .T. ) ;
#24737 = CARTESIAN_POINT ( 'NONE',  ( 23.50000000000007816, 1.873492889145011997, -1.873492889145067508 ) ) ;
#24738 = CARTESIAN_POINT ( 'NONE',  ( 160.2113248654052313, 5.500000000000005329, 0.000000000000000000 ) ) ;
#24739 = CARTESIAN_POINT ( 'NONE',  ( 16.46132486540524553, 2.220446049250313081E-13, -2.500000000000002220 ) ) ;
#24740 = DIRECTION ( 'NONE',  ( -7.147005652999508048E-36, 5.642372883946980038E-36, 1.000000000000000000 ) ) ;
#24741 = DIRECTION ( 'NONE',  ( 0.000000000000000000, 1.000000000000000000, 0.000000000000000000 ) ) ;
#24742 = VERTEX_POINT ( 'NONE', #18831 ) ;
#24743 = CARTESIAN_POINT ( 'NONE',  ( 112.8747167782376124, 2.775557561562891351E-14, 1.849990392679634610 ) ) ;
#24744 =( NAMED_UNIT ( * ) SI_UNIT ( $, .STERADIAN. ) SOLID_ANGLE_UNIT ( ) );
#24745 = CARTESIAN_POINT ( 'NONE',  ( 3.608439182435180470, 6.249999999999982236, -115.1919872981078328 ) ) ;
#24746 = EDGE_CURVE ( 'NONE', #16950, #7068, #27196, .T. ) ;
#24747 = CARTESIAN_POINT ( 'NONE',  ( 135.0000000000000568, 5.117427953996132040, -2.736531087928903094 ) ) ;
#24748 = EDGE_CURVE ( 'NONE', #17985, #23417, #13335, .T. ) ;
#24749 = CARTESIAN_POINT ( 'NONE',  ( -5.999999999999919176, 1.607695154586804565, -90.90331216351299304 ) ) ;
#24750 = CARTESIAN_POINT ( 'NONE',  ( 114.1874999999998153, 1.035533905932779275, 2.500000000000445421 ) ) ;
#24751 = ORIENTED_EDGE ( 'NONE', *, *, #30195, .T. ) ;
#24752 = CARTESIAN_POINT ( 'NONE',  ( 159.2804190760031702, -12.03105614890318265, 3.962454373193818657 ) ) ;
#24753 = AXIS2_PLACEMENT_3D ( 'NONE', #782, #27175, #29019 ) ;
#24754 = CARTESIAN_POINT ( 'NONE',  ( 143.6250000000000284, 0.000000000000000000, -6.000000000000005329 ) ) ;
#24755 = CIRCLE ( 'NONE', #10052, 0.5000000000000004441 ) ;
#24756 = CARTESIAN_POINT ( 'NONE',  ( 3.464101615137757051, -5.999999999999979572, -138.3363248654051745 ) ) ;
#24757 = CARTESIAN_POINT ( 'NONE',  ( 0.000000000000000000, 5.499999999999991118, -51.00000000000004263 ) ) ;
#24758 = CARTESIAN_POINT ( 'NONE',  ( 159.1949251345948255, 5.500000000000012434, -2.278174593052012309 ) ) ;
#24759 = CARTESIAN_POINT ( 'NONE',  ( 5.196152422706629359, -2.999999999999988898, -59.28867513459484684 ) ) ;
#24760 = CARTESIAN_POINT ( 'NONE',  ( 0.000000000000000000, 5.999999999999977796, -61.78867513459485394 ) ) ;
#24761 = CARTESIAN_POINT ( 'NONE',  ( 2.775557561562891351E-14, 6.250000000000033751, -76.93301270189223828 ) ) ;
#24762 = CARTESIAN_POINT ( 'NONE',  ( 136.0000000000000284, -9.165151389911695645, -8.000000000000007105 ) ) ;
#24763 = CARTESIAN_POINT ( 'NONE',  ( 150.7351497308104342, 3.535533905932725318, -3.535533905932725318 ) ) ;
#24764 = DIRECTION ( 'NONE',  ( -7.147005652999508048E-36, 5.642372883946980038E-36, 1.000000000000000000 ) ) ;
#24765 =( NAMED_UNIT ( * ) SI_UNIT ( $, .STERADIAN. ) SOLID_ANGLE_UNIT ( ) );
#24766 = CARTESIAN_POINT ( 'NONE',  ( -5.999999999999963585, 8.134310703387671600E-14, -125.9136751345948397 ) ) ;
#24767 = CARTESIAN_POINT ( 'NONE',  ( -3.175426480542816066, 5.499999999999865885, -131.8750000000000284 ) ) ;
#24768 = CARTESIAN_POINT ( 'NONE',  ( 104.1247167782375556, -1.849990392679468076, 0.000000000000000000 ) ) ;
#24769 = CARTESIAN_POINT ( 'NONE',  ( -3.608439182435115633, 6.249999999999965361, -148.8080127018922667 ) ) ;
#24770 = LINE ( 'NONE', #20013, #9138 ) ;
#24771 = VERTEX_POINT ( 'NONE', #28457 ) ;
#24772 = APPLICATION_CONTEXT ( 'automotive_design' ) ;
#24773 = CARTESIAN_POINT ( 'NONE',  ( 4.763139720814407951, -2.749999999999988454, -60.50000000000000000 ) ) ;
#24774 = CARTESIAN_POINT ( 'NONE',  ( 0.000000000000000000, 5.999999999999977796, -172.2113248654052597 ) ) ;
#24775 = DIRECTION ( 'NONE',  ( -1.000000000000000000, -1.665334536937736783E-16, -2.220446049250315546E-16 ) ) ;
#24776 = ORIENTED_EDGE ( 'NONE', *, *, #3639, .T. ) ;
#24777 = CARTESIAN_POINT ( 'NONE',  ( 110.0624999999998295, 2.499999999999994671, 1.035533905932809473 ) ) ;
#24778 = CARTESIAN_POINT ( 'NONE',  ( 147.0000000000000284, 6.000000000000005329, 0.000000000000000000 ) ) ;
#24779 = CARTESIAN_POINT ( 'NONE',  ( 0.000000000000000000, 0.000000000000000000, 0.000000000000000000 ) ) ;
#24780 = SURFACE_STYLE_USAGE ( .BOTH. , #15923 ) ;
#24781 = EDGE_CURVE ( 'NONE', #269, #11050, #22726, .T. ) ;
#24782 = ORIENTED_EDGE ( 'NONE', *, *, #8154, .F. ) ;
#24783 = CARTESIAN_POINT ( 'NONE',  ( 143.4375000000000284, -4.242640687119298093, -4.242640687119298093 ) ) ;
#24784 = CARTESIAN_POINT ( 'NONE',  ( 161.1372372713044570, -1.259261447730557926, 5.503929387713502486 ) ) ;
#24785 = ORIENTED_EDGE ( 'NONE', *, *, #7678, .T. ) ;
#24786 = AXIS2_PLACEMENT_3D ( 'NONE', #19471, #10099, #21479 ) ;
#24787 = CARTESIAN_POINT ( 'NONE',  ( 6.350852961086080661, -9.614813431917819062E-14, -145.8750000000000284 ) ) ;
#24788 = ORIENTED_EDGE ( 'NONE', *, *, #28474, .T. ) ;
#24789 = CARTESIAN_POINT ( 'NONE',  ( 16.56250000000011013, -1.999999999999911626, -0.8284271247462354770 ) ) ;
#24790 = ORIENTED_EDGE ( 'NONE', *, *, #13655, .F. ) ;
#24791 = CARTESIAN_POINT ( 'NONE',  ( -3.175426480542816510, 5.499999999999865885, -71.87500000000000000 ) ) ;
#24792 = CARTESIAN_POINT ( 'NONE',  ( 2.775557561562891351E-14, -6.250000000000061284, -91.18301270189222407 ) ) ;
#24793 = ORIENTED_EDGE ( 'NONE', *, *, #18090, .F. ) ;
#24794 = PRESENTATION_STYLE_ASSIGNMENT (( #7896 ) ) ;
#24795 = CARTESIAN_POINT ( 'NONE',  ( -5.999999999999962697, 3.323446944526963891E-14, -151.4136751345948255 ) ) ;
#24796 = CARTESIAN_POINT ( 'NONE',  ( 136.0000000000000284, -8.798545334315205579, -8.160000000000000142 ) ) ;
#24797 = CARTESIAN_POINT ( 'NONE',  ( 5.196152422706629359, -2.999999999999988898, -64.71132486540520290 ) ) ;
#24798 = CARTESIAN_POINT ( 'NONE',  ( -3.175426480542816066, -5.500000000000057732, -153.8749999999999716 ) ) ;
#24799 = CARTESIAN_POINT ( 'NONE',  ( 136.8675748654052313, -5.500000000000012434, 2.278174593052012309 ) ) ;
#24800 = CARTESIAN_POINT ( 'NONE',  ( 19.58632486540529172, 1.767766952966542959, -1.767766952966431937 ) ) ;
#24801 = PRESENTATION_LAYER_ASSIGNMENT (  '', '', ( #21389 ) ) ;
#24802 = UNCERTAINTY_MEASURE_WITH_UNIT (LENGTH_MEASURE( 1.000000000000000082E-05 ), #30165, 'distance_accuracy_value', 'NONE');
#24803 = EDGE_CURVE ( 'NONE', #15423, #26042, #9001, .T. ) ;
#24804 = CARTESIAN_POINT ( 'NONE',  ( 6.350852961086080661, -9.614813431917819062E-14, -88.87500000000001421 ) ) ;
#24805 = CARTESIAN_POINT ( 'NONE',  ( -5.999999999999982236, -1.607695154586700426, -140.8466878364870354 ) ) ;
#24806 = CARTESIAN_POINT ( 'NONE',  ( 6.000000000000000888, -1.607695154586752384, -130.6533121635130215 ) ) ;
#24807 = CARTESIAN_POINT ( 'NONE',  ( 3.175426480543072749, 5.499999999999865885, -82.62500000000004263 ) ) ;
#24808 = DIRECTION ( 'NONE',  ( -7.147005652999508048E-36, 5.642372883946980038E-36, 1.000000000000000000 ) ) ;
#24809 = CARTESIAN_POINT ( 'NONE',  ( 161.5000000000000853, -2.984449860524901688, -5.205099329504969674 ) ) ;
#24810 = CARTESIAN_POINT ( 'NONE',  ( 135.3824251345948539, 5.500000000000012434, 2.278174593052012309 ) ) ;
#24811 = CARTESIAN_POINT ( 'NONE',  ( 21.93750000000006395, 2.000000000000212275, -0.8284271247462955401 ) ) ;
#24812 = CARTESIAN_POINT ( 'NONE',  ( -5.999999999999963585, -1.487416814333745711E-14, -165.8363248654052029 ) ) ;
#24813 = CARTESIAN_POINT ( 'NONE',  ( 120.0622167782374419, -1.849990392679472073, 0.7662911109078888172 ) ) ;
#24814 = CARTESIAN_POINT ( 'NONE',  ( -5.999999999999964473, 1.607695154586726405, -173.9806624327026157 ) ) ;
#24815 =( BOUNDED_CURVE ( )  B_SPLINE_CURVE ( 2, ( #12913, #1179, #29287, #8244, #24842, #17657, #26981, #15520, #5945 ),
 .UNSPECIFIED., .F., .T. ) 
 B_SPLINE_CURVE_WITH_KNOTS ( ( 3, 2, 2, 2, 3 ),
 ( 0.3027777777777777013, 0.3037037037037036979, 0.3055555555555555802, 0.3074074074074074625, 0.3083333333333333481 ),
 .UNSPECIFIED. ) 
 CURVE ( )  GEOMETRIC_REPRESENTATION_ITEM ( )  RATIONAL_B_SPLINE_CURVE ( ( 0.9330127018922194093, 0.9330127018922154125, 1.000000000000000000, 0.8660254037844388186, 1.000000000000000000, 0.8660254037844388186, 1.000000000000000000, 0.9330127018922194093, 0.9330127018922194093 ) ) 
 REPRESENTATION_ITEM ( '' )  );
#24816 = EDGE_CURVE ( 'NONE', #2367, #15417, #15041, .T. ) ;
#24817 = EDGE_LOOP ( 'NONE', ( #10572, #10448, #15378, #16491 ) ) ;
#24818 = CARTESIAN_POINT ( 'NONE',  ( 0.000000000000000000, -15.50000000000001421, 5.656854249492387687 ) ) ;
#24819 = CARTESIAN_POINT ( 'NONE',  ( 118.4377832217621034, 1.849990392679591977, 0.7662911109080090544 ) ) ;
#24820 = VECTOR ( 'NONE', #1479, 1000.000000000000000 ) ;
#24821 = DIRECTION ( 'NONE',  ( 1.000000000000000000, 0.000000000000000000, 0.000000000000000000 ) ) ;
#24822 = VERTEX_POINT ( 'NONE', #26309 ) ;
#24823 = VERTEX_POINT ( 'NONE', #19714 ) ;
#24824 = COLOUR_RGB ( '', 0.09019608, 0.27058824, 0.51372549) ;
#24825 = CARTESIAN_POINT ( 'NONE',  ( 4.763139720814407951, -2.749999999999988454, -95.00000000000002842 ) ) ;
#24826 = CARTESIAN_POINT ( 'NONE',  ( -3.464101615137725076, 5.999999999999979572, -70.66367513459481131 ) ) ;
#24827 = CARTESIAN_POINT ( 'NONE',  ( -3.608439182435052128, -6.250000000000110134, -113.8080127018922241 ) ) ;
#24828 = ORIENTED_EDGE ( 'NONE', *, *, #28948, .T. ) ;
#24829 = CARTESIAN_POINT ( 'NONE',  ( -6.000000000000000888, 1.067854986875958443E-15, 7.560779664488942560E-35 ) ) ;
#24830 = CARTESIAN_POINT ( 'NONE',  ( -5.412658773652739619, 3.124999999999975131, -54.18301270189223828 ) ) ;
#24831 = ORIENTED_EDGE ( 'NONE', *, *, #14220, .F. ) ;
#24832 = CARTESIAN_POINT ( 'NONE',  ( 0.000000000000000000, 11.00000000000001066, -3.000000000000002665 ) ) ;
#24833 = DIRECTION ( 'NONE',  ( -8.326672684688675286E-17, -2.081668171172168821E-17, 1.000000000000000000 ) ) ;
#24834 = CARTESIAN_POINT ( 'NONE',  ( -4.763139720814407951, -2.750000000000016431, -170.4999999999999716 ) ) ;
#24835 = CARTESIAN_POINT ( 'NONE',  ( 117.1874999999997726, 1.035533905932659149, 2.500000000000205169 ) ) ;
#24836 = STYLED_ITEM ( 'NONE', ( #3211 ), #13558 ) ;
#24837 = CARTESIAN_POINT ( 'NONE',  ( -3.608439182435052128, -6.250000000000110134, -158.8080127018922383 ) ) ;
#24838 = CARTESIAN_POINT ( 'NONE',  ( -0.7382520721438935452, -9.130873963928037185, 4.026027341348664912 ) ) ;
#24839 = EDGE_CURVE ( 'NONE', #25384, #26506, #10994, .T. ) ;
#24840 = CARTESIAN_POINT ( 'NONE',  ( -3.175426480542816066, 5.499999999999865885, -112.3750000000000568 ) ) ;
#24841 = CARTESIAN_POINT ( 'NONE',  ( -3.175426480542816510, 5.499999999999865885, -109.3750000000000284 ) ) ;
#24842 = CARTESIAN_POINT ( 'NONE',  ( 0.000000000000000000, -5.999999999999991118, -87.46132486540525974 ) ) ;
#24843 = CARTESIAN_POINT ( 'NONE',  ( -3.464101615137725076, 5.999999999999979572, -145.0863248654052029 ) ) ;
#24844 = VERTEX_POINT ( 'NONE', #17284 ) ;
#24845 = CARTESIAN_POINT ( 'NONE',  ( 13.93750000000008882, -1.097466725451319070, 2.649519052838238409 ) ) ;
#24846 = CARTESIAN_POINT ( 'NONE',  ( 116.9374999999998295, 2.500000000000024425, -1.035533905932629173 ) ) ;
#24847 = CARTESIAN_POINT ( 'NONE',  ( 109.4377832217621460, 1.849990392679562001, 0.7662911109080692285 ) ) ;
#24848 = ADVANCED_FACE ( 'NONE', ( #26744 ), #2814, .F. ) ;
#24849 = CARTESIAN_POINT ( 'NONE',  ( -5.999999999999956479, -1.607695154586745057, -134.2693375672974412 ) ) ;
#24850 = EDGE_CURVE ( 'NONE', #10258, #17334, #17269, .T. ) ;
#24851 = VERTEX_POINT ( 'NONE', #26556 ) ;
#24852 = CARTESIAN_POINT ( 'NONE',  ( 0.000000000000000000, 5.999999999999977796, -156.2886751345948824 ) ) ;
#24853 = CARTESIAN_POINT ( 'NONE',  ( -7.216878364870328078, 0.000000000000000000, -83.19198729810780435 ) ) ;
#24854 = CARTESIAN_POINT ( 'NONE',  ( 0.000000000000000000, -5.999999999999991118, -129.4613248654052313 ) ) ;
#24855 = VERTEX_POINT ( 'NONE', #26258 ) ;
#24856 = CARTESIAN_POINT ( 'NONE',  ( -6.000000000000007105, -1.607695154586655129, -65.84668783648703538 ) ) ;
#24857 = VERTEX_POINT ( 'NONE', #613 ) ;
#24858 = CARTESIAN_POINT ( 'NONE',  ( 154.5000000000000284, 6.000000000000005329, 0.000000000000000000 ) ) ;
#24859 =( BOUNDED_SURFACE ( )  B_SPLINE_SURFACE ( 3, 2, ( 
 ( #2107, #13978, #4846 ),
 ( #23470, #14274, #2408 ),
 ( #11820, #14423, #96 ),
 ( #19455, #19597, #21607 ),
 ( #540, #14991, #3283 ),
 ( #29084, #3429, #17459 ),
 ( #12861, #12412, #26773 ),
 ( #28626, #21756, #2844 ) ),
 .UNSPECIFIED., .F., .F., .F. ) 
 B_SPLINE_SURFACE_WITH_KNOTS ( ( 4, 2, 2, 4 ),
 ( 3, 3 ),
 ( 0.006483209092139505421, 0.007220185479624316449, 0.007957161867109126610, 0.009431114642078748667 ),
 ( 0.000000000000000000, 1.000000000000000000 ),
 .UNSPECIFIED. ) 
 GEOMETRIC_REPRESENTATION_ITEM ( )  RATIONAL_B_SPLINE_SURFACE ( (
 ( 1.000000000000000000, 0.9165151389911680990, 1.000000000000000000),
 ( 1.000000000000000000, 0.9165811099393400552, 1.000000000000000000),
 ( 1.000000000000000000, 0.9096513889650220674, 1.000000000000000000),
 ( 1.000000000000000000, 0.8858533194329228921, 1.000000000000000000),
 ( 1.000000000000000000, 0.8692663461314428242, 1.000000000000000000),
 ( 1.000000000000000000, 0.8111162787391891227, 1.000000000000000000),
 ( 1.000000000000000000, 0.7613968795875392104, 1.000000000000000000),
 ( 1.000000000000000000, 0.7050799574999858654, 1.000000000000000000) ) ) 
 REPRESENTATION_ITEM ( '' )  SURFACE ( )  );
#24860 = CARTESIAN_POINT ( 'NONE',  ( 0.000000000000000000, 5.499999999999991118, -123.0000000000000000 ) ) ;
#24861 = CARTESIAN_POINT ( 'NONE',  ( -3.608439182435115633, 6.249999999999965361, -135.3080127018922667 ) ) ;
#24862 = EDGE_LOOP ( 'NONE', ( #8823, #29727, #16375, #20559 ) ) ;
#24863 = DIRECTION ( 'NONE',  ( 0.000000000000000000, 0.000000000000000000, 1.000000000000000000 ) ) ;
#24864 = CARTESIAN_POINT ( 'NONE',  ( 5.412658773652712085, -3.125000000000086153, -123.0669872981078328 ) ) ;
#24865 = CARTESIAN_POINT ( 'NONE',  ( -4.763139720814407951, -2.750000000000016431, -170.4999999999999716 ) ) ;
#24866 = CARTESIAN_POINT ( 'NONE',  ( 159.8041075121309120, -12.29865543435749942, 3.608411551111435411 ) ) ;
#24867 = FILL_AREA_STYLE_COLOUR ( '', #6903 ) ;
#24868 = ORIENTED_EDGE ( 'NONE', *, *, #14919, .T. ) ;
#24869 = CARTESIAN_POINT ( 'NONE',  ( 12.12500000000005329, 1.414213562373201061, 1.414213562373034527 ) ) ;
#24870 = CARTESIAN_POINT ( 'NONE',  ( 114.7886751345947403, -1.999999999999946265, 0.000000000000000000 ) ) ;
#24871 = CARTESIAN_POINT ( 'NONE',  ( -5.196152422706573404, -3.000000000000002665, -117.7113248654052597 ) ) ;
#24872 = CARTESIAN_POINT ( 'NONE',  ( 139.8675748654052597, -5.500000000000012434, 2.278174593052012309 ) ) ;
#24873 = CARTESIAN_POINT ( 'NONE',  ( 0.000000000000000000, 0.000000000000000000, 0.000000000000000000 ) ) ;
#24874 = CARTESIAN_POINT ( 'NONE',  ( 112.7502832217623734, -1.308140751793640533, 1.308140751793640533 ) ) ;
#24875 = CARTESIAN_POINT ( 'NONE',  ( 2.775557561562891351E-14, 6.250000000000033751, -70.06698729810784698 ) ) ;
#24876 = DIRECTION ( 'NONE',  ( -7.147005652999508048E-36, 5.642372883946980038E-36, 1.000000000000000000 ) ) ;
#24877 = CARTESIAN_POINT ( 'NONE',  ( 4.763139720814407951, 2.750000000000002665, -48.25000000000001421 ) ) ;
#24878 = CARTESIAN_POINT ( 'NONE',  ( 119.9999999999997442, 2.445790564474693340, -0.3393521411465372783 ) ) ;
#24879 = EDGE_CURVE ( 'NONE', #23261, #27080, #4436, .T. ) ;
#24880 = DIRECTION ( 'NONE',  ( 0.000000000000000000, 0.000000000000000000, 1.000000000000000000 ) ) ;
#24881 = CARTESIAN_POINT ( 'NONE',  ( -4.763139720814407951, -2.750000000000016431, -133.0000000000000000 ) ) ;
#24882 = ORIENTED_EDGE ( 'NONE', *, *, #10693, .T. ) ;
#24883 = CARTESIAN_POINT ( 'NONE',  ( 24.62500000000020250, 2.649519052838444910, 0.000000000000000000 ) ) ;
#24884 = DIRECTION ( 'NONE',  ( -7.147005652999508048E-36, 5.642372883946980038E-36, 1.000000000000000000 ) ) ;
#24885 = CARTESIAN_POINT ( 'NONE',  ( -5.999999999999962697, 3.323446944526963891E-14, -160.4136751345948255 ) ) ;
#24886 = EDGE_CURVE ( 'NONE', #4566, #5384, #27990, .T. ) ;
#24887 = CARTESIAN_POINT ( 'NONE',  ( 141.2023502691896510, 0.000000000000000000, -5.000000000000004441 ) ) ;
#24888 = ORIENTED_EDGE ( 'NONE', *, *, #4778, .T. ) ;
#24889 = CARTESIAN_POINT ( 'NONE',  ( 6.000000000000000888, 7.762456499804235646E-14, -133.5863248654052029 ) ) ;
#24890 = CARTESIAN_POINT ( 'NONE',  ( 114.2261751345945839, 2.000000000000091926, -0.8284271247460553989 ) ) ;
#24891 = CARTESIAN_POINT ( 'NONE',  ( 2.775557561562891351E-14, -6.250000000000061284, -117.3169872981078043 ) ) ;
#24892 = CARTESIAN_POINT ( 'NONE',  ( 135.0000000000000284, 2.497680721013432859, -4.958406755811053834 ) ) ;
#24893 = CARTESIAN_POINT ( 'NONE',  ( 10.00000000000014744, 1.541898448397849286, 1.609913139633878387 ) ) ;
#24894 = ORIENTED_EDGE ( 'NONE', *, *, #7882, .F. ) ;
#24895 = CARTESIAN_POINT ( 'NONE',  ( 138.6636751345948255, 0.000000000000000000, 5.500000000000005329 ) ) ;
#24896 = CARTESIAN_POINT ( 'NONE',  ( 142.8750000000000284, 0.000000000000000000, 6.000000000000005329 ) ) ;
#24897 =( GEOMETRIC_REPRESENTATION_CONTEXT ( 3 ) GLOBAL_UNCERTAINTY_ASSIGNED_CONTEXT ( ( #28476 ) ) GLOBAL_UNIT_ASSIGNED_CONTEXT ( ( #14760, #19655, #21960 ) ) REPRESENTATION_CONTEXT ( 'NONE', 'WORKASPACE' ) );
#24898 =( BOUNDED_CURVE ( )  B_SPLINE_CURVE ( 2, ( #25828, #23539, #23687, #21082, #25353, #27954, #14348, #2478, #2624 ),
 .UNSPECIFIED., .F., .F. ) 
 B_SPLINE_CURVE_WITH_KNOTS ( ( 3, 2, 2, 2, 3 ),
 ( 0.1764705882352941291, 0.1838235294117647189, 0.1911764705882352811, 0.1985294117647058709, 0.2058823529411764608 ),
 .UNSPECIFIED. ) 
 CURVE ( )  GEOMETRIC_REPRESENTATION_ITEM ( )  RATIONAL_B_SPLINE_CURVE ( ( 1.000000000000000000, 0.9238795325112867385, 1.000000000000000000, 0.9238795325112867385, 1.000000000000000000, 0.9238795325112867385, 1.000000000000000000, 0.9238795325112867385, 1.000000000000000000 ) ) 
 REPRESENTATION_ITEM ( '' )  );
#24899 = ORIENTED_EDGE ( 'NONE', *, *, #1925, .F. ) ;
#24900 = ORIENTED_EDGE ( 'NONE', *, *, #17630, .F. ) ;
#24901 = FILL_AREA_STYLE_COLOUR ( '', #826 ) ;
#24902 = CARTESIAN_POINT ( 'NONE',  ( 0.000000000000000000, 0.000000000000000000, 0.000000000000000000 ) ) ;
#24903 = CARTESIAN_POINT ( 'NONE',  ( -5.999999999999944933, 1.607695154586759934, -119.9806624327026157 ) ) ;
#24904 = CARTESIAN_POINT ( 'NONE',  ( 1.000000000000000888, 0.000000000000000000, 0.000000000000000000 ) ) ;
#24905 = CARTESIAN_POINT ( 'NONE',  ( 2.775557561562891351E-14, 6.250000000000033751, -64.93301270189222407 ) ) ;
#24906 = CARTESIAN_POINT ( 'NONE',  ( 147.3601497308104058, -3.535533905932725318, -3.535533905932725318 ) ) ;
#24907 = CYLINDRICAL_SURFACE ( 'NONE', #23171, 6.000000000000000888 ) ;
#24908 = CARTESIAN_POINT ( 'NONE',  ( 0.000000000000000000, 0.000000000000000000, 0.000000000000000000 ) ) ;
#24909 = CARTESIAN_POINT ( 'NONE',  ( 136.0000000000000284, 1.469576158976823947E-15, 12.00000000000000178 ) ) ;
#24910 = EDGE_CURVE ( 'NONE', #14303, #9700, #11226, .T. ) ;
#24911 = ADVANCED_FACE ( 'NONE', ( #20274 ), #7266, .T. ) ;
#24912 = CARTESIAN_POINT ( 'NONE',  ( 6.350852961086080661, -9.614813431917819062E-14, -130.8750000000000284 ) ) ;
#24913 = CARTESIAN_POINT ( 'NONE',  ( 5.412658773652739619, 3.124999999999988898, -149.1830127018922667 ) ) ;
#24914 = DIRECTION ( 'NONE',  ( -1.000000000000000000, -1.665334536937736783E-16, -2.220446049250315546E-16 ) ) ;
#24915 = PRESENTATION_LAYER_ASSIGNMENT (  '', '', ( #22484 ) ) ;
#24916 = VERTEX_POINT ( 'NONE', #3960 ) ;
#24917 = CARTESIAN_POINT ( 'NONE',  ( -6.350852961085760029, -1.281975124255709124E-13, -65.62500000000002842 ) ) ;
#24918 = PLANE ( 'NONE',  #7509 ) ;
#24919 = CARTESIAN_POINT ( 'NONE',  ( -5.999999999999962697, 3.323446944526963891E-14, -149.9136751345948255 ) ) ;
#24920 = ORIENTED_EDGE ( 'NONE', *, *, #29730, .T. ) ;
#24921 = CARTESIAN_POINT ( 'NONE',  ( 110.7499999999998010, 2.775557561562891351E-14, -2.499999999999946709 ) ) ;
#24922 = CARTESIAN_POINT ( 'NONE',  ( 143.5312500000000284, -2.485281374238556218, -6.000000000000005329 ) ) ;
#24923 = CARTESIAN_POINT ( 'NONE',  ( 5.196152422706629359, -2.999999999999988898, -117.7886751345948397 ) ) ;
#24924 = CARTESIAN_POINT ( 'NONE',  ( 13.12500000000016342, 1.414213562373145550, 1.414213562373034527 ) ) ;
#24925 = CARTESIAN_POINT ( 'NONE',  ( 6.000000000000052403, -1.607695154586662678, -48.73066243270260856 ) ) ;
#24926 = ORIENTED_EDGE ( 'NONE', *, *, #12170, .T. ) ;
#24927 = CARTESIAN_POINT ( 'NONE',  ( 135.7500000000000284, -6.000000000000005329, 0.000000000000000000 ) ) ;
#24928 = CARTESIAN_POINT ( 'NONE',  ( 142.7738248654052313, -3.889087296526011706, 3.889087296526011706 ) ) ;
#24929 = ORIENTED_EDGE ( 'NONE', *, *, #28096, .F. ) ;
#24930 = CARTESIAN_POINT ( 'NONE',  ( 3.175426480543072749, 5.499999999999865885, -145.6250000000000284 ) ) ;
#24931 = CARTESIAN_POINT ( 'NONE',  ( 14.18749999999996447, 0.8284271247462955401, 2.000000000000031530 ) ) ;
#24932 = ORIENTED_EDGE ( 'NONE', *, *, #24634, .T. ) ;
#24933 = CARTESIAN_POINT ( 'NONE',  ( -4.763139720814407951, -2.750000000000016431, -70.00000000000000000 ) ) ;
#24934 = CARTESIAN_POINT ( 'NONE',  ( 14.81250000000001599, -2.649519052838238409, 1.097466725451559322 ) ) ;
#24935 = CARTESIAN_POINT ( 'NONE',  ( 5.412658773652712085, -3.125000000000086153, -92.43301270189225249 ) ) ;
#24936 = CARTESIAN_POINT ( 'NONE',  ( -5.999340830937887503, -9.219973438021447976, -24.59179872956897839 ) ) ;
#24937 = CARTESIAN_POINT ( 'NONE',  ( -5.196152422706601826, 2.999999999999975131, -106.5386751345948113 ) ) ;
#24938 = CARTESIAN_POINT ( 'NONE',  ( 106.3363248654051034, -1.414213562373228816, -1.414213562373034527 ) ) ;
#24939 = CARTESIAN_POINT ( 'NONE',  ( 3.464101615137852974, 5.999999999999884537, -98.83632486540518869 ) ) ;
#24940 = FACE_OUTER_BOUND ( 'NONE', #2394, .T. ) ;
#24941 = EDGE_CURVE ( 'NONE', #20441, #23894, #5649, .T. ) ;
#24942 = CARTESIAN_POINT ( 'NONE',  ( -4.763139720814407951, -2.750000000000016431, -160.0000000000000284 ) ) ;
#24943 = CARTESIAN_POINT ( 'NONE',  ( 0.000000000000000000, 0.000000000000000000, 0.000000000000000000 ) ) ;
#24944 = CARTESIAN_POINT ( 'NONE',  ( -4.763139720814407951, -2.750000000000016431, -85.00000000000001421 ) ) ;
#24945 = CARTESIAN_POINT ( 'NONE',  ( -4.999999999999990230, -24.99999999999999289, 8.000000000000007105 ) ) ;
#24946 = CARTESIAN_POINT ( 'NONE',  ( 101.5358983848621932, -1.203706215242021998E-32, -9.216943876758866938E-48 ) ) ;
#24947 = CARTESIAN_POINT ( 'NONE',  ( -2.775557561562891351E-14, -5.500000000000115463, -71.25000000000002842 ) ) ;
#24948 = FACE_OUTER_BOUND ( 'NONE', #15992, .T. ) ;
#24949 = CARTESIAN_POINT ( 'NONE',  ( 154.7961002691896795, 2.071067811865468400, -4.999999999999989342 ) ) ;
#24950 = CARTESIAN_POINT ( 'NONE',  ( 5.999999999999949374, 1.607695154586804565, -106.5193375672974696 ) ) ;
#24951 = DIRECTION ( 'NONE',  ( -1.000000000000000000, -1.665334536937736783E-16, -2.220446049250315546E-16 ) ) ;
#24952 = CARTESIAN_POINT ( 'NONE',  ( 5.999999999999999112, 2.951592740943527306E-14, -149.1636751345948824 ) ) ;
#24953 = CARTESIAN_POINT ( 'NONE',  ( 22.25000000000010303, 1.110223024625156540E-13, 1.999999999999946265 ) ) ;
#24954 = CARTESIAN_POINT ( 'NONE',  ( 119.7497167782375556, 1.308140751793696044, 1.308140751793862577 ) ) ;
#24955 = DIRECTION ( 'NONE',  ( 0.000000000000000000, 0.000000000000000000, -1.000000000000000000 ) ) ;
#24956 = ORIENTED_EDGE ( 'NONE', *, *, #11907, .T. ) ;
#24957 = AXIS2_PLACEMENT_3D ( 'NONE', #3042, #593, #9979 ) ;
#24958 = CARTESIAN_POINT ( 'NONE',  ( 154.5000000000000284, 6.000000000000005329, 0.000000000000000000 ) ) ;
#24959 = CARTESIAN_POINT ( 'NONE',  ( -5.999999999999963585, 1.780251999655701777E-13, -52.41367513459481842 ) ) ;
#24960 = ORIENTED_EDGE ( 'NONE', *, *, #8813, .T. ) ;
#24961 = EDGE_LOOP ( 'NONE', ( #29881, #19481, #25034, #23027 ) ) ;
#24962 = EDGE_CURVE ( 'NONE', #691, #19810, #17444, .T. ) ;
#24963 = CARTESIAN_POINT ( 'NONE',  ( -3.175426480542816510, -5.500000000000057732, -93.87500000000002842 ) ) ;
#24964 = CARTESIAN_POINT ( 'NONE',  ( 0.000000000000000000, -5.999999999999991118, -89.53867513459485394 ) ) ;
#24965 = CARTESIAN_POINT ( 'NONE',  ( 2.775557561562891351E-14, 6.250000000000033751, -114.4330127018922099 ) ) ;
#24966 = ORIENTED_EDGE ( 'NONE', *, *, #7561, .T. ) ;
#24967 = DIRECTION ( 'NONE',  ( -7.147005652999508048E-36, 5.642372883946980038E-36, 1.000000000000000000 ) ) ;
#24968 = PRESENTATION_STYLE_ASSIGNMENT (( #20693 ) ) ;
#24969 = DIRECTION ( 'NONE',  ( -1.000000000000000000, -1.665334536937731113E-16, 1.526556658859586792E-16 ) ) ;
#24970 = CARTESIAN_POINT ( 'NONE',  ( -3.608439182435115633, 6.249999999999965361, -55.80801270189227381 ) ) ;
#24971 = AXIS2_PLACEMENT_3D ( 'NONE', #20414, #3811, #6131 ) ;
#24972 = ORIENTED_EDGE ( 'NONE', *, *, #6044, .T. ) ;
#24973 =( BOUNDED_CURVE ( )  B_SPLINE_CURVE ( 2, ( #30243, #30397, #16321, #20743, #16169, #18147, #14017, #8761, #20897 ),
 .UNSPECIFIED., .F., .F. ) 
 B_SPLINE_CURVE_WITH_KNOTS ( ( 3, 2, 2, 2, 3 ),
 ( 0.1125000000000005579, 0.1187500000000003275, 0.1250000000000001110, 0.1312499999999998945, 0.1374999999999996780 ),
 .UNSPECIFIED. ) 
 CURVE ( )  GEOMETRIC_REPRESENTATION_ITEM ( )  RATIONAL_B_SPLINE_CURVE ( ( 0.9999999999999932276, 0.9238795325112935108, 1.000000000000000000, 0.9238795325112867385, 1.000000000000000000, 0.9238795325112867385, 1.000000000000000000, 0.9238795325112908463, 0.9999999999999958922 ) ) 
 REPRESENTATION_ITEM ( '' )  );
#24974 = EDGE_CURVE ( 'NONE', #651, #21812, #17681, .T. ) ;
#24975 = AXIS2_PLACEMENT_3D ( 'NONE', #22561, #4252, #15835 ) ;
#24976 = CARTESIAN_POINT ( 'NONE',  ( 146.2574251345948539, -2.278174593051733421, 5.500000000000292211 ) ) ;
#24977 = CARTESIAN_POINT ( 'NONE',  ( -4.763139720814407951, 2.749999999999946709, -160.2500000000000000 ) ) ;
#24978 = CARTESIAN_POINT ( 'NONE',  ( 115.9374999999998010, 2.500000000000055067, -1.035533905932629173 ) ) ;
#24979 = CARTESIAN_POINT ( 'NONE',  ( 5.999999999999949374, 1.607695154586804565, -108.0193375672974128 ) ) ;
#24980 = CARTESIAN_POINT ( 'NONE',  ( -3.175426480542816066, -5.500000000000057732, -105.8750000000000284 ) ) ;
#24981 = CARTESIAN_POINT ( 'NONE',  ( 160.4136751345948824, 0.000000000000000000, -5.500000000000005329 ) ) ;
#24982 = CARTESIAN_POINT ( 'NONE',  ( 4.763139720814407951, 2.750000000000002665, -97.75000000000000000 ) ) ;
#24983 =( BOUNDED_CURVE ( )  B_SPLINE_CURVE ( 2, ( #6542, #27265, #3458, #15501, #24964, #12892, #20375, #8547, #6381 ),
 .UNSPECIFIED., .F., .T. ) 
 B_SPLINE_CURVE_WITH_KNOTS ( ( 3, 2, 2, 2, 3 ),
 ( 0.6805555555555554692, 0.6814814814814814659, 0.6833333333333333481, 0.6851851851851852304, 0.6861111111111111160 ),
 .UNSPECIFIED. ) 
 CURVE ( )  GEOMETRIC_REPRESENTATION_ITEM ( )  RATIONAL_B_SPLINE_CURVE ( ( 0.9330127018922194093, 0.9330127018922154125, 1.000000000000000000, 0.8660254037844388186, 1.000000000000000000, 0.8660254037844388186, 1.000000000000000000, 0.9330127018922194093, 0.9330127018922194093 ) ) 
 REPRESENTATION_ITEM ( '' )  );
#24984 = CARTESIAN_POINT ( 'NONE',  ( -3.464101615137725076, 5.999999999999979572, -151.6636751345947971 ) ) ;
#24985 = SURFACE_STYLE_USAGE ( .BOTH. , #3635 ) ;
#24986 = CARTESIAN_POINT ( 'NONE',  ( 6.000000000000000888, 7.762456499804234384E-14, -118.5863248654052313 ) ) ;
#24987 = EDGE_LOOP ( 'NONE', ( #20335, #18514, #29924, #18286 ) ) ;
#24988 = CARTESIAN_POINT ( 'NONE',  ( 15.62500000000011013, 2.649519052838389399, -1.110223024625156540E-13 ) ) ;
#24989 = CARTESIAN_POINT ( 'NONE',  ( 115.2499999999998721, -5.551115123125782702E-14, 2.500000000000057732 ) ) ;
#24990 = CARTESIAN_POINT ( 'NONE',  ( 109.5002832217622881, 1.308140751793640533, 1.308140751793640533 ) ) ;
#24991 = DIRECTION ( 'NONE',  ( 1.260129944081490070E-35, 5.642372883946978702E-36, 1.000000000000000000 ) ) ;
#24992 = VERTEX_POINT ( 'NONE', #1673 ) ;
#24993 = CARTESIAN_POINT ( 'NONE',  ( 109.7113248654051176, 2.000000000000057288, 0.000000000000000000 ) ) ;
#24994 = CARTESIAN_POINT ( 'NONE',  ( -7.216878364870328078, 0.000000000000000000, -87.69198729810783277 ) ) ;
#24995 = CIRCLE ( 'NONE', #22054, 16.00000000000000000 ) ;
#24996 = CARTESIAN_POINT ( 'NONE',  ( -5.999999999999963585, -1.487416814333745711E-14, -167.3363248654052029 ) ) ;
#24997 = ORIENTED_EDGE ( 'NONE', *, *, #23760, .F. ) ;
#24998 = CARTESIAN_POINT ( 'NONE',  ( -1.966823652257158273, 10.82907957849943337, -30.68208441639941952 ) ) ;
#24999 = CARTESIAN_POINT ( 'NONE',  ( -4.763139720814407951, 2.749999999999946709, -151.2500000000000000 ) ) ;
#25000 = MECHANICAL_DESIGN_GEOMETRIC_PRESENTATION_REPRESENTATION (  '', ( #26946 ), #17674 ) ;
#25001 = ORIENTED_EDGE ( 'NONE', *, *, #18154, .F. ) ;
#25002 = CARTESIAN_POINT ( 'NONE',  ( 157.9687500000000284, -2.485281374238585972, 6.000000000000005329 ) ) ;
#25003 = EDGE_CURVE ( 'NONE', #9617, #28281, #19413, .T. ) ;
#25004 = CARTESIAN_POINT ( 'NONE',  ( -2.775557561562891351E-14, -5.500000000000115463, -120.7500000000000284 ) ) ;
#25005 = CARTESIAN_POINT ( 'NONE',  ( 3.608439182435180470, -6.249999999999997335, -139.0580127018922099 ) ) ;
#25006 = VERTEX_POINT ( 'NONE', #22424 ) ;
#25007 = CARTESIAN_POINT ( 'NONE',  ( 3.464101615137852974, 5.999999999999884537, -160.9136751345947971 ) ) ;
#25008 = CARTESIAN_POINT ( 'NONE',  ( 5.412658773652739619, 3.124999999999988898, -121.3169872981078043 ) ) ;
#25009 = CARTESIAN_POINT ( 'NONE',  ( 3.608439182435180470, -6.249999999999997335, -180.1919872981078186 ) ) ;
#25010 = CARTESIAN_POINT ( 'NONE',  ( 4.763139720814407951, -2.749999999999988454, -171.5000000000000000 ) ) ;
#25011 = CARTESIAN_POINT ( 'NONE',  ( 20.33632486540521001, -1.767766952966209892, -1.767766952966542959 ) ) ;
#25012 = ORIENTED_EDGE ( 'NONE', *, *, #18288, .T. ) ;
#25013 = CARTESIAN_POINT ( 'NONE',  ( 11.75000000000012079, 1.665334536937734811E-13, -2.000000000000057288 ) ) ;
#25014 = EDGE_CURVE ( 'NONE', #18697, #25268, #8902, .T. ) ;
#25015 = CARTESIAN_POINT ( 'NONE',  ( 5.999999999999999112, 2.951592740943527306E-14, -164.1636751345948824 ) ) ;
#25016 = DIRECTION ( 'NONE',  ( 1.000000000000000000, 0.000000000000000000, 0.000000000000000000 ) ) ;
#25017 = CARTESIAN_POINT ( 'NONE',  ( -5.196152422706573404, -3.000000000000002665, -55.28867513459484684 ) ) ;
#25018 = CARTESIAN_POINT ( 'NONE',  ( 23.21132486540530948, -2.499999999999891198, -1.110223024625156540E-13 ) ) ;
#25019 = CARTESIAN_POINT ( 'NONE',  ( 110.4377832217621034, 1.849990392679562001, 0.7662911109079489913 ) ) ;
#25020 = CARTESIAN_POINT ( 'NONE',  ( -7.216878364870328078, 0.000000000000000000, -71.19198729810781856 ) ) ;
#25021 = CARTESIAN_POINT ( 'NONE',  ( -7.216878364870328078, 0.000000000000000000, -51.69198729810779014 ) ) ;
#25022 = DIRECTION ( 'NONE',  ( 0.000000000000000000, 0.000000000000000000, -1.000000000000000000 ) ) ;
#25023 = CARTESIAN_POINT ( 'NONE',  ( -3.175426480542816510, 5.499999999999865885, -52.37500000000002842 ) ) ;
#25024 = CARTESIAN_POINT ( 'NONE',  ( -5.999999999999963585, -1.487416814333745711E-14, -55.41367513459483973 ) ) ;
#25025 = CARTESIAN_POINT ( 'NONE',  ( 2.775557561562891351E-14, 20.00000000000001776, -25.00000000000002132 ) ) ;
#25026 = AXIS2_PLACEMENT_3D ( 'NONE', #22426, #5658, #5971 ) ;
#25027 = CARTESIAN_POINT ( 'NONE',  ( 4.763139720814407951, 2.750000000000002665, -132.2500000000000284 ) ) ;
#25028 = DIRECTION ( 'NONE',  ( -8.326672684688675286E-17, -2.081668171172168821E-17, 1.000000000000000000 ) ) ;
#25029 = ORIENTED_EDGE ( 'NONE', *, *, #1254, .T. ) ;
#25030 = CARTESIAN_POINT ( 'NONE',  ( 23.93750000000009592, -1.097466725451379244, 2.649519052838178457 ) ) ;
#25031 = CARTESIAN_POINT ( 'NONE',  ( 159.9300748654052029, 2.278174593051865315, -5.500000000000158984 ) ) ;
#25032 = CARTESIAN_POINT ( 'NONE',  ( 0.000000000000000000, 0.000000000000000000, 0.000000000000000000 ) ) ;
#25033 = CARTESIAN_POINT ( 'NONE',  ( 137.6398502691896510, -3.535533905932752852, 3.535533905932725318 ) ) ;
#25034 = ORIENTED_EDGE ( 'NONE', *, *, #12299, .T. ) ;
#25035 = CARTESIAN_POINT ( 'NONE',  ( 110.8122167782374987, 0.7662911109077388261, 1.849990392679772278 ) ) ;
#25036 = CARTESIAN_POINT ( 'NONE',  ( 6.000000000000000888, -3.330669073875464691E-16, -7.560779664488942560E-35 ) ) ;
#25037 = CARTESIAN_POINT ( 'NONE',  ( 10.18750000000014033, 0.8284271247463557142, 2.000000000000031530 ) ) ;
#25038 = CARTESIAN_POINT ( 'NONE',  ( 3.608439182435180470, 6.249999999999982236, -112.1919872981078186 ) ) ;
#25039 = CARTESIAN_POINT ( 'NONE',  ( 135.0000000000000000, 3.024630907472011465, -4.708032601928953120 ) ) ;
#25040 = CARTESIAN_POINT ( 'NONE',  ( 10.00000000000014744, 0.7333107046349622848, 2.235284847858831636 ) ) ;
#25041 = ORIENTED_EDGE ( 'NONE', *, *, #20670, .T. ) ;
#25042 = DIRECTION ( 'NONE',  ( -7.147005652999508048E-36, 5.642372883946980038E-36, 1.000000000000000000 ) ) ;
#25043 = CARTESIAN_POINT ( 'NONE',  ( 139.4062500000000284, 6.000000000000005329, -2.485281374238555774 ) ) ;
#25044 = EDGE_CURVE ( 'NONE', #15395, #3348, #18133, .T. ) ;
#25045 = VECTOR ( 'NONE', #9055, 1000.000000000000000 ) ;
#25046 = ORIENTED_EDGE ( 'NONE', *, *, #221, .F. ) ;
#25047 = FACE_OUTER_BOUND ( 'NONE', #4640, .T. ) ;
#25048 = CARTESIAN_POINT ( 'NONE',  ( -6.350852961085760029, -1.281975124255709124E-13, -49.12500000000000711 ) ) ;
#25049 = CARTESIAN_POINT ( 'NONE',  ( 23.18750000000004619, 0.8284271247462955401, 1.999999999999851674 ) ) ;
#25050 = CARTESIAN_POINT ( 'NONE',  ( 117.4136751345946834, 1.414213562373145550, 1.414213562373034527 ) ) ;
#25051 = EDGE_CURVE ( 'NONE', #30382, #9852, #23547, .T. ) ;
#25052 = DIRECTION ( 'NONE',  ( 1.000000000000000000, 0.000000000000000000, 0.000000000000000000 ) ) ;
#25053 = CARTESIAN_POINT ( 'NONE',  ( -5.412658773652684552, -3.125000000000099920, -70.43301270189222407 ) ) ;
#25054 = EDGE_CURVE ( 'NONE', #16378, #3967, #27629, .T. ) ;
#25055 = CIRCLE ( 'NONE', #19681, 16.18577070100374726 ) ;
#25056 = CARTESIAN_POINT ( 'NONE',  ( 151.7663997308104342, -4.999999999999989342, -2.071067811865468400 ) ) ;
#25057 = DIRECTION ( 'NONE',  ( 1.000000000000000000, 0.000000000000000000, 0.000000000000000000 ) ) ;
#25058 = DIRECTION ( 'NONE',  ( -1.000000000000000000, -1.665334536937731113E-16, 1.526556658859586792E-16 ) ) ;
#25059 = CARTESIAN_POINT ( 'NONE',  ( 12.22617513459478999, 2.500000000000205169, -1.035533905932869425 ) ) ;
#25060 = CARTESIAN_POINT ( 'NONE',  ( 10.00000000000002132, 6.000000000000083489, 2.049675791781519072E-14 ) ) ;
#25061 = CARTESIAN_POINT ( 'NONE',  ( -6.350852961085760029, -1.281975124255709124E-13, -131.6250000000000284 ) ) ;
#25062 = CARTESIAN_POINT ( 'NONE',  ( 101.5358983848621932, -1.203706215242021998E-32, -9.216943876758866938E-48 ) ) ;
#25063 = CARTESIAN_POINT ( 'NONE',  ( 14.03867513459489125, 5.551115123125782702E-14, -2.500000000000057732 ) ) ;
#25064 = ORIENTED_EDGE ( 'NONE', *, *, #4604, .T. ) ;
#25065 = CARTESIAN_POINT ( 'NONE',  ( -6.350852961085760029, -1.281975124255709124E-13, -64.12500000000001421 ) ) ;
#25066 = CARTESIAN_POINT ( 'NONE',  ( 5.196152422706629359, -2.999999999999988898, -154.7113248654052313 ) ) ;
#25067 = SURFACE_STYLE_FILL_AREA ( #18051 ) ;
#25068 = FACE_OUTER_BOUND ( 'NONE', #22634, .T. ) ;
#25069 = EDGE_LOOP ( 'NONE', ( #24352, #19656, #16636, #15852 ) ) ;
#25070 = CARTESIAN_POINT ( 'NONE',  ( 110.2499999999998010, -5.551115123125782702E-14, 2.500000000000168754 ) ) ;
#25071 = CARTESIAN_POINT ( 'NONE',  ( 144.3750000000000284, 0.000000000000000000, 6.000000000000005329 ) ) ;
#25072 = CARTESIAN_POINT ( 'NONE',  ( 3.464101615137757051, -5.999999999999979572, -117.9136751345948255 ) ) ;
#25073 = CARTESIAN_POINT ( 'NONE',  ( 6.000000000000000888, 1.743066579297358182E-13, -85.58632486540523132 ) ) ;
#25074 =( BOUNDED_CURVE ( )  B_SPLINE_CURVE ( 2, ( #24685, #3473, #10579, #26973, #3931, #6102, #13218, #24979, #20251 ),
 .UNSPECIFIED., .F., .T. ) 
 B_SPLINE_CURVE_WITH_KNOTS ( ( 3, 2, 2, 2, 3 ),
 ( 0.4527777777777778345, 0.4537037037037037202, 0.4555555555555556024, 0.4574074074074073737, 0.4583333333333332593 ),
 .UNSPECIFIED. ) 
 CURVE ( )  GEOMETRIC_REPRESENTATION_ITEM ( )  RATIONAL_B_SPLINE_CURVE ( ( 0.9330127018922194093, 0.9330127018922234061, 1.000000000000000000, 0.8660254037844388186, 1.000000000000000000, 0.8660254037844388186, 1.000000000000000000, 0.9330127018922234061, 0.9330127018922194093 ) ) 
 REPRESENTATION_ITEM ( '' )  );
#25075 = ORIENTED_EDGE ( 'NONE', *, *, #13799, .T. ) ;
#25076 = CARTESIAN_POINT ( 'NONE',  ( 137.7187500000000284, 2.485281374238555774, -6.000000000000005329 ) ) ;
#25077 = CARTESIAN_POINT ( 'NONE',  ( -5.999999999999963585, 1.780251999655701777E-13, -109.4136751345948113 ) ) ;
#25078 = ORIENTED_EDGE ( 'NONE', *, *, #15702, .T. ) ;
#25079 = VECTOR ( 'NONE', #8165, 1000.000000000000114 ) ;
#25080 = ADVANCED_FACE ( 'NONE', ( #16609 ), #9357, .T. ) ;
#25081 = CARTESIAN_POINT ( 'NONE',  ( 4.763139720814407951, 2.750000000000002665, -144.2500000000000000 ) ) ;
#25082 = CARTESIAN_POINT ( 'NONE',  ( 14.68750000000004796, -0.8284271247460553989, -1.999999999999971800 ) ) ;
#25083 = ORIENTED_EDGE ( 'NONE', *, *, #28582, .F. ) ;
#25084 = CARTESIAN_POINT ( 'NONE',  ( -4.763139720814407951, 2.749999999999946709, -74.75000000000004263 ) ) ;
#25085 = AXIS2_PLACEMENT_3D ( 'NONE', #18910, #15866, #30396 ) ;
#25086 = CARTESIAN_POINT ( 'NONE',  ( -5.999999999999963585, 9.296355089585909904E-15, -164.9136751345948255 ) ) ;
#25087 = EDGE_CURVE ( 'NONE', #8567, #18033, #30389, .T. ) ;
#25088 = VERTEX_POINT ( 'NONE', #4584 ) ;
#25089 = CARTESIAN_POINT ( 'NONE',  ( -0.8083154347085889091, -10.97740844234573387, -30.95886765600326029 ) ) ;
#25090 = CARTESIAN_POINT ( 'NONE',  ( -5.630955349224697315, 2.071796769723730058, -179.9999999999999432 ) ) ;
#25091 = CARTESIAN_POINT ( 'NONE',  ( -5.196152422706573404, -3.000000000000002665, -91.28867513459482552 ) ) ;
#25092 = DIRECTION ( 'NONE',  ( 1.000000000000000000, 7.404948406885115640E-21, -2.688430705412078735E-21 ) ) ;
#25093 = CARTESIAN_POINT ( 'NONE',  ( -3.175426480542816066, 5.499999999999865885, -155.8750000000000000 ) ) ;
#25094 = CARTESIAN_POINT ( 'NONE',  ( -9.999999999999772626, -89.00000000000001421, 4.000000000000003553 ) ) ;
#25095 = CARTESIAN_POINT ( 'NONE',  ( -1.170107792542705694, 5.489964307952521771, -180.0000000000000000 ) ) ;
#25096 = CIRCLE ( 'NONE', #9427, 1.000000000000000000 ) ;
#25097 = CARTESIAN_POINT ( 'NONE',  ( 4.763139720814407951, 2.750000000000002665, -85.75000000000000000 ) ) ;
#25098 = CARTESIAN_POINT ( 'NONE',  ( 104.4372167782374277, 0.7662911109077987781, -1.849990392679231599 ) ) ;
#25099 = DIRECTION ( 'NONE',  ( 1.000000000000000000, 0.000000000000000000, 0.000000000000000000 ) ) ;
#25100 = CARTESIAN_POINT ( 'NONE',  ( -2.775557561562891351E-14, -5.500000000000115463, -69.75000000000002842 ) ) ;
#25101 = CARTESIAN_POINT ( 'NONE',  ( 135.0000000000000284, -6.982120021884474781, 8.500000000000007105 ) ) ;
#25102 = CARTESIAN_POINT ( 'NONE',  ( 148.3273502691896510, -5.000000000000004441, 0.000000000000000000 ) ) ;
#25103 = CARTESIAN_POINT ( 'NONE',  ( 0.000000000000000000, 0.000000000000000000, 0.000000000000000000 ) ) ;
#25104 = CARTESIAN_POINT ( 'NONE',  ( 6.000000000000007105, -1.607695154586741060, -174.7306624327025872 ) ) ;
#25105 = CARTESIAN_POINT ( 'NONE',  ( 0.000000000000000000, 0.000000000000000000, 0.000000000000000000 ) ) ;
#25106 = CARTESIAN_POINT ( 'NONE',  ( 6.000000000000000888, 1.743066579297358182E-13, -104.1636751345948397 ) ) ;
#25107 = LINE ( 'NONE', #8695, #24411 ) ;
#25108 = CARTESIAN_POINT ( 'NONE',  ( 139.5000000000000000, -24.99999999999999289, 7.500000000000007105 ) ) ;
#25109 = ORIENTED_EDGE ( 'NONE', *, *, #15348, .F. ) ;
#25110 = CARTESIAN_POINT ( 'NONE',  ( 158.4375000000000284, -4.242640687119298093, -4.242640687119298093 ) ) ;
#25111 = CARTESIAN_POINT ( 'NONE',  ( -6.000000000000000888, 1.067854986875958443E-15, 7.560779664488942560E-35 ) ) ;
#25112 = ADVANCED_FACE ( 'NONE', ( #26079 ), #21191, .T. ) ;
#25113 = EDGE_CURVE ( 'NONE', #605, #6232, #28396, .T. ) ;
#25114 = ORIENTED_EDGE ( 'NONE', *, *, #24622, .F. ) ;
#25115 = CARTESIAN_POINT ( 'NONE',  ( -2.775557561562891351E-14, -5.500000000000115463, -96.75000000000000000 ) ) ;
#25116 = CARTESIAN_POINT ( 'NONE',  ( 5.412658773652712085, -3.125000000000086153, -108.9330127018922667 ) ) ;
#25117 = CARTESIAN_POINT ( 'NONE',  ( 6.000000000000000888, 1.743066579297358182E-13, -94.58632486540521711 ) ) ;
#25118 = CARTESIAN_POINT ( 'NONE',  ( 0.000000000000000000, -9.500000000000008882, -5.000000000000004441 ) ) ;
#25119 = CARTESIAN_POINT ( 'NONE',  ( 139.5000000000000284, -8.798545334315205579, -8.160000000000000142 ) ) ;
#25120 = CARTESIAN_POINT ( 'NONE',  ( -2.775557561562891351E-14, -5.500000000000115463, -165.7500000000000000 ) ) ;
#25121 = CARTESIAN_POINT ( 'NONE',  ( 3.608439182435180470, -6.249999999999997335, -52.05801270189225960 ) ) ;
#25122 = PRESENTATION_STYLE_ASSIGNMENT (( #17537 ) ) ;
#25123 = VERTEX_POINT ( 'NONE', #25786 ) ;
#25124 = CARTESIAN_POINT ( 'NONE',  ( -5.999999999999962697, 3.323446944526963891E-14, -152.9136751345948255 ) ) ;
#25125 = DIRECTION ( 'NONE',  ( 1.000000000000000000, 0.000000000000000000, 0.000000000000000000 ) ) ;
#25126 = CARTESIAN_POINT ( 'NONE',  ( -4.763139720814407951, 2.749999999999946709, -161.7500000000000568 ) ) ;
#25127 = CARTESIAN_POINT ( 'NONE',  ( 116.5624999999998863, -2.499999999999844569, -1.035533905932629173 ) ) ;
#25128 = FILL_AREA_STYLE_COLOUR ( '', #9812 ) ;
#25129 = CARTESIAN_POINT ( 'NONE',  ( 0.000000000000000000, 5.499999999999991118, -106.5000000000000426 ) ) ;
#25130 = CARTESIAN_POINT ( 'NONE',  ( 105.8363248654049613, 1.414213562373201061, 1.414213562373367594 ) ) ;
#25131 = DIRECTION ( 'NONE',  ( -1.000000000000000000, -1.665334536937736783E-16, -2.220446049250315546E-16 ) ) ;
#25132 = CARTESIAN_POINT ( 'NONE',  ( -4.763139720814407951, 2.749999999999946709, -94.25000000000000000 ) ) ;
#25133 = CARTESIAN_POINT ( 'NONE',  ( 162.5773502691896510, 5.000000000000004441, 0.000000000000000000 ) ) ;
#25134 = CARTESIAN_POINT ( 'NONE',  ( 11.28867513459488947, 2.500000000000002220, 0.000000000000000000 ) ) ;
#25135 = CARTESIAN_POINT ( 'NONE',  ( 0.7667987217272868028, -15.49901228270247877, 8.125944816629214529 ) ) ;
#25136 = ORIENTED_EDGE ( 'NONE', *, *, #20072, .T. ) ;
#25137 = CARTESIAN_POINT ( 'NONE',  ( 12.43750000000001776, 1.097466725451679892, -2.649519052838238409 ) ) ;
#25138 = CARTESIAN_POINT ( 'NONE',  ( 116.8124999999998010, 1.035533905932719101, -2.499999999999784173 ) ) ;
#25139 = CARTESIAN_POINT ( 'NONE',  ( 109.3752832217621744, 1.849990392679579099, 1.110223024625156540E-13 ) ) ;
#25140 = LINE ( 'NONE', #13527, #6126 ) ;
#25141 = ORIENTED_EDGE ( 'NONE', *, *, #3057, .T. ) ;
#25142 = B_SPLINE_CURVE_WITH_KNOTS ( 'NONE', 3,
 ( #14328, #14182, #9377, #9829, #12169, #2460 ),
 .UNSPECIFIED., .F., .F.,
 ( 4, 2, 4 ),
 ( 0.000000000000000000, 0.0009337058470447063543, 0.001867411694089412709 ),
 .UNSPECIFIED. ) ;
#25143 = CARTESIAN_POINT ( 'NONE',  ( 110.0238248654050182, -0.8284271247460852639, 2.000000000000212275 ) ) ;
#25144 = CARTESIAN_POINT ( 'NONE',  ( 2.775557561562891351E-14, -6.250000000000061284, -90.31698729810783277 ) ) ;
#25145 = CARTESIAN_POINT ( 'NONE',  ( 140.5000000000000284, -10.99818166789401275, 4.799999999999998934 ) ) ;
#25146 = ORIENTED_EDGE ( 'NONE', *, *, #9858, .F. ) ;
#25147 = CARTESIAN_POINT ( 'NONE',  ( -5.197562551122842933, 9.697615191485752462, -28.02238803416286927 ) ) ;
#25148 = ADVANCED_FACE ( 'NONE', ( #4877 ), #11853, .T. ) ;
#25149 = VECTOR ( 'NONE', #1618, 1000.000000000000000 ) ;
#25150 = ORIENTED_EDGE ( 'NONE', *, *, #3388, .F. ) ;
#25151 = CARTESIAN_POINT ( 'NONE',  ( 158.3437500000000568, -6.000000000000005329, -2.485281374238555774 ) ) ;
#25152 = CARTESIAN_POINT ( 'NONE',  ( 3.175426480543072749, 5.499999999999865885, -118.6250000000000284 ) ) ;
#25153 =( BOUNDED_CURVE ( )  B_SPLINE_CURVE ( 2, ( #28053, #11681, #23180, #6723, #11838, #25769, #29494, #13836, #13995 ),
 .UNSPECIFIED., .F., .T. ) 
 B_SPLINE_CURVE_WITH_KNOTS ( ( 3, 2, 2, 2, 3 ),
 ( 0.3593750000000000000, 0.3671875000000000000, 0.3750000000000000000, 0.3828125000000000000, 0.3906250000000000000 ),
 .UNSPECIFIED. ) 
 CURVE ( )  GEOMETRIC_REPRESENTATION_ITEM ( )  RATIONAL_B_SPLINE_CURVE ( ( 1.000000000000000000, 0.9238795325112867385, 1.000000000000000000, 0.9238795325112867385, 1.000000000000000000, 0.9238795325112867385, 1.000000000000000000, 0.9238795325112867385, 1.000000000000000000 ) ) 
 REPRESENTATION_ITEM ( '' )  );
#25154 = CARTESIAN_POINT ( 'NONE',  ( 2.775557561562891351E-14, 6.250000000000033751, -136.9330127018922383 ) ) ;
#25155 = ORIENTED_EDGE ( 'NONE', *, *, #18397, .F. ) ;
#25156 = CARTESIAN_POINT ( 'NONE',  ( 0.000000000000000000, 10.00000000000000888, -3.000000000000002665 ) ) ;
#25157 = CARTESIAN_POINT ( 'NONE',  ( -3.608439182435052128, -6.250000000000110134, -124.9419872981078186 ) ) ;
#25158 = CARTESIAN_POINT ( 'NONE',  ( 5.412658773652712085, -3.125000000000086153, -180.0669872981078186 ) ) ;
#25159 = ORIENTED_EDGE ( 'NONE', *, *, #29977, .T. ) ;
#25160 = CARTESIAN_POINT ( 'NONE',  ( 12.75000000000017764, 1.665334536937734811E-13, -2.000000000000001776 ) ) ;
#25161 = CARTESIAN_POINT ( 'NONE',  ( 140.2370868712064862, -11.61854343560322533, 4.230991509104584658 ) ) ;
#25162 =( BOUNDED_CURVE ( )  B_SPLINE_CURVE ( 2, ( #5080, #21551, #19247, #24274, #28576, #26282, #21701, #17101, #12467 ),
 .UNSPECIFIED., .F., .T. ) 
 B_SPLINE_CURVE_WITH_KNOTS ( ( 3, 2, 2, 2, 3 ),
 ( 0.7861111111111110938, 0.7870370370370369795, 0.7888888888888888618, 0.7907407407407407440, 0.7916666666666666297 ),
 .UNSPECIFIED. ) 
 CURVE ( )  GEOMETRIC_REPRESENTATION_ITEM ( )  RATIONAL_B_SPLINE_CURVE ( ( 0.9330127018922194093, 0.9330127018922194093, 1.000000000000000000, 0.8660254037844388186, 1.000000000000000000, 0.8660254037844388186, 1.000000000000000000, 0.9330127018922234061, 0.9330127018922194093 ) ) 
 REPRESENTATION_ITEM ( '' )  );
#25163 = CARTESIAN_POINT ( 'NONE',  ( 159.0000000000000284, -11.07692307692307843, -4.615384615384617639 ) ) ;
#25164 = DIRECTION ( 'NONE',  ( -1.000000000000000000, -1.665334536937731113E-16, 1.526556658859586792E-16 ) ) ;
#25165 = CARTESIAN_POINT ( 'NONE',  ( 112.2113248654051176, -1.999999999999946265, 0.000000000000000000 ) ) ;
#25166 = CARTESIAN_POINT ( 'NONE',  ( 110.6877832217622739, -0.7662911109076785410, 1.849990392679712103 ) ) ;
#25167 = CARTESIAN_POINT ( 'NONE',  ( -5.412658773652739619, 3.124999999999975131, -74.31698729810781856 ) ) ;
#25168 = CARTESIAN_POINT ( 'NONE',  ( -3.608439182435052128, -6.250000000000110134, -63.44198729810784698 ) ) ;
#25169 = CARTESIAN_POINT ( 'NONE',  ( 3.464101615137852974, 5.999999999999884537, -110.8363248654052455 ) ) ;
#25170 = CARTESIAN_POINT ( 'NONE',  ( -6.350852961085760029, -1.281975124255709124E-13, -47.62500000000000000 ) ) ;
#25171 = CARTESIAN_POINT ( 'NONE',  ( 1.110223024625164183E-16, -2.000000000000012879, -1.776356839400262692E-15 ) ) ;
#25172 = CARTESIAN_POINT ( 'NONE',  ( -3.464101615137757051, -5.999999999999979572, -153.5863248654051461 ) ) ;
#25173 = CARTESIAN_POINT ( 'NONE',  ( -4.763139720814407951, 2.749999999999946709, -119.7500000000000284 ) ) ;
#25174 = AXIS2_PLACEMENT_3D ( 'NONE', #28530, #7499, #16911 ) ;
#25175 = VERTEX_POINT ( 'NONE', #4734 ) ;
#25176 = CARTESIAN_POINT ( 'NONE',  ( 135.6636751345948255, 0.000000000000000000, 5.500000000000005329 ) ) ;
#25177 = ADVANCED_FACE ( 'NONE', ( #27912 ), #30236, .F. ) ;
#25178 = CARTESIAN_POINT ( 'NONE',  ( 0.000000000000000000, 5.999999999999977796, -122.7113248654052597 ) ) ;
#25179 = CYLINDRICAL_SURFACE ( 'NONE', #19234, 2.499999999999999112 ) ;
#25180 = CARTESIAN_POINT ( 'NONE',  ( 139.3273502691896510, -5.000000000000004441, 0.000000000000000000 ) ) ;
#25181 = VERTEX_POINT ( 'NONE', #7197 ) ;
#25182 = CARTESIAN_POINT ( 'NONE',  ( 107.9997167782376835, -1.308140751793585022, 1.308140751793640533 ) ) ;
#25183 = CARTESIAN_POINT ( 'NONE',  ( 118.3988248654050182, -0.8284271247461453269, -1.999999999999791278 ) ) ;
#25184 = CARTESIAN_POINT ( 'NONE',  ( 113.9997167782376266, -1.308140751793585022, 1.308140751793862577 ) ) ;
#25185 = CARTESIAN_POINT ( 'NONE',  ( 3.608439182435180470, -6.249999999999997335, -112.6919872981078328 ) ) ;
#25186 = CARTESIAN_POINT ( 'NONE',  ( 0.000000000000000000, -5.999999999999991118, -54.46132486540522422 ) ) ;
#25187 = EDGE_CURVE ( 'NONE', #29595, #8771, #4372, .T. ) ;
#25188 = DIRECTION ( 'NONE',  ( 0.000000000000000000, 0.000000000000000000, 1.000000000000000000 ) ) ;
#25189 = ORIENTED_EDGE ( 'NONE', *, *, #5691, .T. ) ;
#25190 = CARTESIAN_POINT ( 'NONE',  ( 159.1428483359083828, -12.00649502811498515, 3.992243735981535480 ) ) ;
#25191 = CARTESIAN_POINT ( 'NONE',  ( 143.8125000000000284, 4.242640687119298093, -4.242640687119298093 ) ) ;
#25192 = CARTESIAN_POINT ( 'NONE',  ( 3.608439182435180470, 6.249999999999982236, -143.6919872981078470 ) ) ;
#25193 = ORIENTED_EDGE ( 'NONE', *, *, #20736, .T. ) ;
#25194 = AXIS2_PLACEMENT_3D ( 'NONE', #27972, #2048, #20641 ) ;
#25195 = CARTESIAN_POINT ( 'NONE',  ( 18.78867513459486815, -2.499999999999946709, -5.551115123125782702E-14 ) ) ;
#25196 = CARTESIAN_POINT ( 'NONE',  ( 5.196152422706629359, -2.999999999999988898, -93.21132486540523132 ) ) ;
#25197 = CARTESIAN_POINT ( 'NONE',  ( 23.87500000000009237, 1.414213562373256572, -1.414213562373145550 ) ) ;
#25198 = SURFACE_STYLE_FILL_AREA ( #9089 ) ;
#25199 = CARTESIAN_POINT ( 'NONE',  ( 135.7574251345947971, -2.278174593051640162, 5.500000000000382805 ) ) ;
#25200 = CARTESIAN_POINT ( 'NONE',  ( 7.216878364870455975, -6.409875621278545621E-14, -69.80801270189220986 ) ) ;
#25201 = CARTESIAN_POINT ( 'NONE',  ( 135.6737246954143643, -8.728829995092375782, -8.172675940895006264 ) ) ;
#25202 = CARTESIAN_POINT ( 'NONE',  ( 148.4851497308104342, -3.535533905932725318, 3.535533905932725318 ) ) ;
#25203 = FACE_OUTER_BOUND ( 'NONE', #1187, .T. ) ;
#25204 = CARTESIAN_POINT ( 'NONE',  ( -2.910268709469100014E-14, -10.99999999999998224, -14.99152654425661702 ) ) ;
#25205 = CARTESIAN_POINT ( 'NONE',  ( -5.196152422706573404, -3.000000000000002665, -155.7886751345948255 ) ) ;
#25206 = DIRECTION ( 'NONE',  ( 0.000000000000000000, 1.000000000000000000, 0.000000000000000000 ) ) ;
#25207 = CARTESIAN_POINT ( 'NONE',  ( 106.7886751345947403, -1.999999999999946265, 0.000000000000000000 ) ) ;
#25208 = CARTESIAN_POINT ( 'NONE',  ( -6.350852961085760029, -1.281975124255709124E-13, -121.1250000000000426 ) ) ;
#25209 = DIRECTION ( 'NONE',  ( 0.8660254037844380415, -0.5000000000000008882, -1.905606012543395233E-16 ) ) ;
#25210 = CARTESIAN_POINT ( 'NONE',  ( -5.412658773652739619, 3.124999999999975131, -144.1830127018922667 ) ) ;
#25211 = LINE ( 'NONE', #11285, #29213 ) ;
#25212 = FACE_OUTER_BOUND ( 'NONE', #5465, .T. ) ;
#25213 = ORIENTED_EDGE ( 'NONE', *, *, #27082, .T. ) ;
#25214 = EDGE_CURVE ( 'NONE', #8542, #3410, #26634, .T. ) ;
#25215 = CARTESIAN_POINT ( 'NONE',  ( -3.175426480542816066, 5.499999999999865885, -56.87500000000004263 ) ) ;
#25216 = CARTESIAN_POINT ( 'NONE',  ( 5.999999999999949374, 1.607695154586804565, -124.5193375672974412 ) ) ;
#25217 = CARTESIAN_POINT ( 'NONE',  ( -15.49999999999999289, -25.00000000000007816, 8.000000000000007105 ) ) ;
#25218 = CARTESIAN_POINT ( 'NONE',  ( 5.196152422706629359, 3.000000000000002665, -170.9613248654052313 ) ) ;
#25219 = VERTEX_POINT ( 'NONE', #3022 ) ;
#25220 = CARTESIAN_POINT ( 'NONE',  ( 119.9997167782376124, -1.308140751793529510, 1.308140751793973600 ) ) ;
#25221 = CARTESIAN_POINT ( 'NONE',  ( 148.8750000000000284, 0.000000000000000000, 6.000000000000005329 ) ) ;
#25222 = CARTESIAN_POINT ( 'NONE',  ( 160.0053871411751913, -11.56467308583480147, -3.224818504556521415 ) ) ;
#25223 = ADVANCED_FACE ( 'NONE', ( #15177 ), #9961, .T. ) ;
#25224 = CARTESIAN_POINT ( 'NONE',  ( 137.2500000000000284, -6.000000000000005329, 0.000000000000000000 ) ) ;
#25225 = CARTESIAN_POINT ( 'NONE',  ( -3.175426480542816510, 5.499999999999865885, -137.8750000000000568 ) ) ;
#25226 = CARTESIAN_POINT ( 'NONE',  ( 14.25000000000012434, 5.551115123125782702E-14, 2.000000000000001776 ) ) ;
#25227 = ORIENTED_EDGE ( 'NONE', *, *, #4426, .F. ) ;
#25228 = CARTESIAN_POINT ( 'NONE',  ( -2.775557561562891351E-14, -5.500000000000115463, -74.25000000000004263 ) ) ;
#25229 = CARTESIAN_POINT ( 'NONE',  ( -5.803206942314495187, -9.345129262100574152, -26.57517091834633050 ) ) ;
#25230 = DIRECTION ( 'NONE',  ( 1.000000000000000000, -5.551115123125773458E-17, -1.260129944081490338E-35 ) ) ;
#25231 = CARTESIAN_POINT ( 'NONE',  ( 0.000000000000000000, 0.000000000000000000, 0.000000000000000000 ) ) ;
#25232 = CARTESIAN_POINT ( 'NONE',  ( -6.000000000000000000, 1.067854986875958245E-15, -180.0000000000000568 ) ) ;
#25233 = APPLICATION_PROTOCOL_DEFINITION ( 'draft international standard', 'automotive_design', 1998, #22635 ) ;
#25234 = CARTESIAN_POINT ( 'NONE',  ( -4.763139720814407951, 2.749999999999946709, -146.7500000000000568 ) ) ;
#25235 = CARTESIAN_POINT ( 'NONE',  ( 139.6518077262924180, -8.798545368671454980, 8.159999962955303943 ) ) ;
#25236 = CIRCLE ( 'NONE', #5638, 16.50000000000000355 ) ;
#25237 = CARTESIAN_POINT ( 'NONE',  ( 6.350852961086080661, -9.614813431917819062E-14, -142.8750000000000568 ) ) ;
#25238 = LINE ( 'NONE', #4210, #15471 ) ;
#25239 = EDGE_CURVE ( 'NONE', #18212, #799, #14334, .T. ) ;
#25240 = CARTESIAN_POINT ( 'NONE',  ( 3.175426480543072749, 5.499999999999865885, -84.12499999999997158 ) ) ;
#25241 = CARTESIAN_POINT ( 'NONE',  ( 116.8363248654050039, 1.414213562373173305, 1.414213562373034527 ) ) ;
#25242 = CARTESIAN_POINT ( 'NONE',  ( 6.350852961086080661, -9.614813431917819062E-14, -75.37500000000000000 ) ) ;
#25243 =( BOUNDED_CURVE ( )  B_SPLINE_CURVE ( 2, ( #6442, #18307, #15871, #1687, #15712, #20135, #29325, #24729, #1378 ),
 .UNSPECIFIED., .F., .T. ) 
 B_SPLINE_CURVE_WITH_KNOTS ( ( 3, 2, 2, 2, 3 ),
 ( 0.4472222222222221877, 0.4481481481481481288, 0.4500000000000000111, 0.4518518518518518379, 0.4527777777777777790 ),
 .UNSPECIFIED. ) 
 CURVE ( )  GEOMETRIC_REPRESENTATION_ITEM ( )  RATIONAL_B_SPLINE_CURVE ( ( 0.9330127018922194093, 0.9330127018922174109, 1.000000000000000000, 0.8660254037844388186, 1.000000000000000000, 0.8660254037844388186, 1.000000000000000000, 0.9330127018922194093, 0.9330127018922194093 ) ) 
 REPRESENTATION_ITEM ( '' )  );
#25244 = CARTESIAN_POINT ( 'NONE',  ( -5.999999999999963585, 1.780251999655701777E-13, -74.91367513459485394 ) ) ;
#25245 = CARTESIAN_POINT ( 'NONE',  ( 148.6086002691896510, -2.071067811865468400, -4.999999999999989342 ) ) ;
#25246 = CARTESIAN_POINT ( 'NONE',  ( 3.464101615137757051, -5.999999999999979572, -87.91367513459483973 ) ) ;
#25247 = CARTESIAN_POINT ( 'NONE',  ( 135.5000000000000284, -9.047800747817580813, -8.000000000000007105 ) ) ;
#25248 = CARTESIAN_POINT ( 'NONE',  ( 18.37500000000008527, -1.414213562373090038, 1.414213562372867994 ) ) ;
#25249 = CARTESIAN_POINT ( 'NONE',  ( -5.196152422706601826, 2.999999999999975131, -54.96132486540522422 ) ) ;
#25250 = CARTESIAN_POINT ( 'NONE',  ( 118.3122167782374561, -0.7662911109076485650, -1.849990392679411677 ) ) ;
#25251 = EDGE_CURVE ( 'NONE', #8489, #15139, #1539, .T. ) ;
#25252 = CARTESIAN_POINT ( 'NONE',  ( 0.000000000000000000, 0.000000000000000000, 0.000000000000000000 ) ) ;
#25253 = VERTEX_POINT ( 'NONE', #10415 ) ;
#25254 = CARTESIAN_POINT ( 'NONE',  ( 153.7500000000000284, -6.000000000000005329, 0.000000000000000000 ) ) ;
#25255 = CARTESIAN_POINT ( 'NONE',  ( 117.6877832217621034, -0.7662911109077388261, 1.849990392679712103 ) ) ;
#25256 = CARTESIAN_POINT ( 'NONE',  ( 6.000000000000000888, 1.743066579297358182E-13, -97.58632486540524553 ) ) ;
#25257 = ORIENTED_EDGE ( 'NONE', *, *, #14025, .T. ) ;
#25258 = ORIENTED_EDGE ( 'NONE', *, *, #2146, .T. ) ;
#25259 = VERTEX_POINT ( 'NONE', #17341 ) ;
#25260 = CARTESIAN_POINT ( 'NONE',  ( -4.763139720814407951, -2.750000000000016431, -98.50000000000002842 ) ) ;
#25261 = CARTESIAN_POINT ( 'NONE',  ( 115.4613248654051318, 2.775557561562891351E-14, -2.000000000000001776 ) ) ;
#25262 = CARTESIAN_POINT ( 'NONE',  ( 3.608439182435180470, 6.249999999999982236, -107.0580127018922667 ) ) ;
#25263 = DIRECTION ( 'NONE',  ( 0.000000000000000000, 0.000000000000000000, -1.000000000000000000 ) ) ;
#25264 = LINE ( 'NONE', #9164, #1259 ) ;
#25265 = AXIS2_PLACEMENT_3D ( 'NONE', #9108, #18503, #6331 ) ;
#25266 = CARTESIAN_POINT ( 'NONE',  ( -3.175426480542816510, -5.500000000000057732, -162.8750000000000284 ) ) ;
#25267 = CARTESIAN_POINT ( 'NONE',  ( 5.196152422706629359, -2.999999999999988898, -105.7886751345948397 ) ) ;
#25268 = VERTEX_POINT ( 'NONE', #19483 ) ;
#25269 = CARTESIAN_POINT ( 'NONE',  ( -5.999999999999957367, 1.607695154586737507, -152.9806624327025872 ) ) ;
#25270 =( LENGTH_UNIT ( ) NAMED_UNIT ( * ) SI_UNIT ( .MILLI., .METRE. ) );
#25271 = CARTESIAN_POINT ( 'NONE',  ( 140.0466131354633887, -8.931230826727917460, 8.014915759236114212 ) ) ;
#25272 = CARTESIAN_POINT ( 'NONE',  ( 3.175426480543072749, -5.500000000000105693, -159.6250000000000284 ) ) ;
#25273 = CARTESIAN_POINT ( 'NONE',  ( 114.9999999999999716, 2.500000000000002220, 0.000000000000000000 ) ) ;
#25274 = B_SPLINE_CURVE_WITH_KNOTS ( 'NONE', 3,
 ( #7006, #13660, #16124, #1945, #20697, #9018, #18408, #27727, #25427, #4552, #4391, #13818, #13976, #23163, #2105, #11510, #20850, #9165, #23316, #11666, #24189, #23900, #24044, #12410, #5435, #21301, #14846, #7747, #10234, #10081, #2989, #2692, #26047, #7897, #12556, #3134, #21903, #19015, #4991, #12117, #19454, #5584, #16865, #837 ),
 .UNSPECIFIED., .F., .F.,
 ( 4, 2, 2, 2, 2, 2, 2, 2, 2, 2, 2, 2, 2, 2, 2, 2, 2, 2, 2, 2, 2, 4 ),
 ( 0.000000000000000000, 0.001197331758471049034, 0.002394663516942098069, 0.003591995275413146886, 0.004789327033884196137, 0.005387992913119717293, 0.005986658792355239317, 0.007183990550826290303, 0.008381322309297341289, 0.009578654067768392275, 0.01017731994700391690, 0.01077598582623943979, 0.01137465170547496615, 0.01197331758471049078, 0.01317064934318154697, 0.01376931522241707680, 0.01436798110165260489, 0.01556531286012365588, 0.01676264461859470686, 0.01736131049783023322, 0.01795997637706575611, 0.01915730813553680537 ),
 .UNSPECIFIED. ) ;
#25275 = EDGE_CURVE ( 'NONE', #799, #1357, #4677, .T. ) ;
#25276 = CARTESIAN_POINT ( 'NONE',  ( -3.175426480542816066, -5.500000000000057732, -110.3750000000000426 ) ) ;
#25277 = DIRECTION ( 'NONE',  ( 1.000000000000000000, -0.000000000000000000, -0.000000000000000000 ) ) ;
#25278 = CARTESIAN_POINT ( 'NONE',  ( 0.000000000000000000, -5.999999999999991118, -122.5386751345948255 ) ) ;
#25279 = EDGE_CURVE ( 'NONE', #1574, #30369, #5768, .T. ) ;
#25280 = CARTESIAN_POINT ( 'NONE',  ( -4.763139720814407951, 2.749999999999946709, -98.75000000000000000 ) ) ;
#25281 = CARTESIAN_POINT ( 'NONE',  ( 134.9999999981442045, -7.162237350910601208, 8.424967526247618466 ) ) ;
#25282 = ORIENTED_EDGE ( 'NONE', *, *, #9293, .F. ) ;
#25283 = CARTESIAN_POINT ( 'NONE',  ( 11.00000000000003730, -1.873492889144900975, 1.873492889144900975 ) ) ;
#25284 = AXIS2_PLACEMENT_3D ( 'NONE', #11664, #22844, #8551 ) ;
#25285 = CARTESIAN_POINT ( 'NONE',  ( 118.5624999999997016, -2.499999999999874767, -1.035533905932568777 ) ) ;
#25286 = DIRECTION ( 'NONE',  ( 0.000000000000000000, 0.000000000000000000, -1.000000000000000000 ) ) ;
#25287 = CARTESIAN_POINT ( 'NONE',  ( 111.6877832217621176, -0.7662911109077388261, 1.849990392679652151 ) ) ;
#25288 = CARTESIAN_POINT ( 'NONE',  ( -6.000000000000007105, -1.607695154586655129, -86.26933756729742697 ) ) ;
#25289 = ORIENTED_EDGE ( 'NONE', *, *, #6574, .T. ) ;
#25290 = CARTESIAN_POINT ( 'NONE',  ( 5.196152422706629359, -2.999999999999988898, -169.7113248654051745 ) ) ;
#25291 = CARTESIAN_POINT ( 'NONE',  ( 109.4372167782374845, 0.7662911109079189043, -1.849990392679231599 ) ) ;
#25292 =( GEOMETRIC_REPRESENTATION_CONTEXT ( 3 ) GLOBAL_UNCERTAINTY_ASSIGNED_CONTEXT ( ( #29397 ) ) GLOBAL_UNIT_ASSIGNED_CONTEXT ( ( #18830, #4819, #25715 ) ) REPRESENTATION_CONTEXT ( 'NONE', 'WORKASPACE' ) );
#25293 = CARTESIAN_POINT ( 'NONE',  ( 3.608439182435180470, -6.249999999999997335, -87.19198729810783277 ) ) ;
#25294 =( BOUNDED_CURVE ( )  B_SPLINE_CURVE ( 2, ( #5059, #26261, #16793, #5212, #21678, #2911, #19225, #14489, #7237 ),
 .UNSPECIFIED., .F., .F. ) 
 B_SPLINE_CURVE_WITH_KNOTS ( ( 3, 2, 2, 2, 3 ),
 ( 0.01562500000000000000, 0.02343750000000000000, 0.03125000000000000000, 0.03906250000000000000, 0.04687500000000000000 ),
 .UNSPECIFIED. ) 
 CURVE ( )  GEOMETRIC_REPRESENTATION_ITEM ( )  RATIONAL_B_SPLINE_CURVE ( ( 1.000000000000000000, 0.9238795325112867385, 1.000000000000000000, 0.9238795325112867385, 1.000000000000000000, 0.9238795325112867385, 1.000000000000000000, 0.9238795325112867385, 1.000000000000000000 ) ) 
 REPRESENTATION_ITEM ( '' )  );
#25295 = CARTESIAN_POINT ( 'NONE',  ( 111.0238248654050608, -0.8284271247461753029, 2.000000000000271783 ) ) ;
#25296 = ORIENTED_EDGE ( 'NONE', *, *, #6658, .F. ) ;
#25297 = CARTESIAN_POINT ( 'NONE',  ( -14.99999999999999289, -54.99999999999990763, -7.500000000000007105 ) ) ;
#25298 = ORIENTED_EDGE ( 'NONE', *, *, #2956, .F. ) ;
#25299 = ORIENTED_EDGE ( 'NONE', *, *, #9261, .F. ) ;
#25300 = CARTESIAN_POINT ( 'NONE',  ( 150.5625000000000568, -4.242640687119298093, 4.242640687119298093 ) ) ;
#25301 = EDGE_LOOP ( 'NONE', ( #4375, #772, #18096, #21958 ) ) ;
#25302 = CARTESIAN_POINT ( 'NONE',  ( 0.000000000000000000, 5.499999999999991118, -124.5000000000000568 ) ) ;
#25303 = CARTESIAN_POINT ( 'NONE',  ( 21.31250000000007105, 2.649519052838358757, -1.097466725451619718 ) ) ;
#25304 = CARTESIAN_POINT ( 'NONE',  ( 3.608439182435180470, -6.249999999999997335, -130.0580127018922383 ) ) ;
#25305 = ORIENTED_EDGE ( 'NONE', *, *, #15702, .F. ) ;
#25306 = CARTESIAN_POINT ( 'NONE',  ( 150.9449251345948539, -5.500000000000012434, 2.278174593052012309 ) ) ;
#25307 = CARTESIAN_POINT ( 'NONE',  ( 3.608439182435180470, 6.249999999999982236, -172.1919872981078470 ) ) ;
#25308 = CARTESIAN_POINT ( 'NONE',  ( 7.216878364870455975, -6.409875621278545621E-14, -179.9419872981078186 ) ) ;
#25309 = CARTESIAN_POINT ( 'NONE',  ( 159.1716635061148679, -11.33697504938031919, 3.989315678507943552 ) ) ;
#25310 = ORIENTED_EDGE ( 'NONE', *, *, #3829, .F. ) ;
#25311 = CARTESIAN_POINT ( 'NONE',  ( 0.000000000000000000, 0.000000000000000000, 0.000000000000000000 ) ) ;
#25312 = CARTESIAN_POINT ( 'NONE',  ( 0.000000000000000000, 0.000000000000000000, 0.000000000000000000 ) ) ;
#25313 = CARTESIAN_POINT ( 'NONE',  ( 112.5863248654050608, 1.414213562373145550, -1.414213562373145550 ) ) ;
#25314 = CARTESIAN_POINT ( 'NONE',  ( 110.7502832217622881, -1.308140751793585022, 1.308140751793640533 ) ) ;
#25315 = CARTESIAN_POINT ( 'NONE',  ( 2.775557561562891351E-14, 6.250000000000033751, -77.56698729810784698 ) ) ;
#25316 = CARTESIAN_POINT ( 'NONE',  ( -7.216878364870328078, 0.000000000000000000, -59.19198729810781856 ) ) ;
#25317 = CARTESIAN_POINT ( 'NONE',  ( 5.196152422706629359, -2.999999999999988898, -170.2886751345948255 ) ) ;
#25318 = CARTESIAN_POINT ( 'NONE',  ( 6.350852961086080661, -9.614813431917819062E-14, -51.37500000000002132 ) ) ;
#25319 = CARTESIAN_POINT ( 'NONE',  ( -5.999999999999963585, 1.780251999655701777E-13, -111.8363248654052313 ) ) ;
#25320 = CARTESIAN_POINT ( 'NONE',  ( 5.196152422706629359, -2.999999999999988898, -153.2113248654052313 ) ) ;
#25321 = CARTESIAN_POINT ( 'NONE',  ( 105.3511751345946124, 2.000000000000121680, 0.8284271247464761734 ) ) ;
#25322 = EDGE_CURVE ( 'NONE', #28323, #27307, #7991, .T. ) ;
#25323 = CARTESIAN_POINT ( 'NONE',  ( -3.175426480542816510, 5.499999999999865885, -121.3750000000000284 ) ) ;
#25324 = CARTESIAN_POINT ( 'NONE',  ( -4.763139720814407951, -2.750000000000016431, -157.0000000000000284 ) ) ;
#25325 = CARTESIAN_POINT ( 'NONE',  ( 153.9300748654051745, 2.278174593051810692, -5.500000000000211386 ) ) ;
#25326 = ORIENTED_EDGE ( 'NONE', *, *, #28784, .T. ) ;
#25327 = CARTESIAN_POINT ( 'NONE',  ( 20.37500000000017053, 1.665334536937734811E-13, -2.649519052838389399 ) ) ;
#25328 = CARTESIAN_POINT ( 'NONE',  ( 143.1636751345948255, 0.000000000000000000, 5.500000000000005329 ) ) ;
#25329 = STYLED_ITEM ( 'NONE', ( #7727 ), #3859 ) ;
#25330 = CARTESIAN_POINT ( 'NONE',  ( 136.4211002691896510, -4.999999999999989342, -2.071067811865468400 ) ) ;
#25331 = EDGE_LOOP ( 'NONE', ( #27877, #1856, #4032, #6470 ) ) ;
#25332 = CARTESIAN_POINT ( 'NONE',  ( 110.1872167782374703, -1.849990392679501827, -0.7662911109076485650 ) ) ;
#25333 = CARTESIAN_POINT ( 'NONE',  ( 151.3050748654052313, 5.500000000000012434, 2.278174593052012309 ) ) ;
#25334 = CARTESIAN_POINT ( 'NONE',  ( 114.0622167782374845, -1.849990392679501827, 0.7662911109078287542 ) ) ;
#25335 = CARTESIAN_POINT ( 'NONE',  ( -5.412658773652739619, 3.124999999999975131, -111.8169872981078470 ) ) ;
#25336 = CARTESIAN_POINT ( 'NONE',  ( 17.33632486540525974, -1.767766952966154381, -1.767766952966487448 ) ) ;
#25337 =( BOUNDED_SURFACE ( )  B_SPLINE_SURFACE ( 3, 2, ( 
 ( #11402, #4445, #30400 ),
 ( #30098, #29939, #4594 ),
 ( #9367, #27777, #146 ),
 ( #23210, #20748, #9063 ),
 ( #4747, #16468, #6753 ),
 ( #25797, #14173, #13713 ),
 ( #4294, #25478, #2156 ),
 ( #23511, #11865, #11558 ),
 ( #2307, #21205, #9527 ),
 ( #1840, #27465, #20903 ) ),
 .UNSPECIFIED., .F., .F., .T. ) 
 B_SPLINE_SURFACE_WITH_KNOTS ( ( 4, 2, 2, 2, 4 ),
 ( 3, 3 ),
 ( 3.141592653589793116, 3.534291735288517255, 3.926990816987241395, 4.319689898685965090, 4.712388980384689674 ),
 ( 0.000000000000000000, 1.000000000000000000 ),
 .UNSPECIFIED. ) 
 GEOMETRIC_REPRESENTATION_ITEM ( )  RATIONAL_B_SPLINE_SURFACE ( (
 ( 1.000000000000000000, 0.7071067811865475727, 1.000000000000000000),
 ( 1.000000000000000000, 0.7066757001360287616, 1.000000000000000000),
 ( 1.000000000000000000, 0.7265518147277496563, 1.000000000000000000),
 ( 1.000000000000000000, 0.7876784249694541717, 1.000000000000000000),
 ( 1.000000000000000000, 0.8282379786091766949, 1.000000000000000000),
 ( 1.000000000000000000, 0.9038128289597016085, 1.000000000000000000),
 ( 1.000000000000000000, 0.9386556746367812343, 1.000000000000000000),
 ( 1.000000000000000000, 0.9867291651255319929, 1.000000000000000000),
 ( 1.000000000000000000, 1.000158598892035622, 1.000000000000000000),
 ( 1.000000000000000000, 1.000000000000000000, 1.000000000000000000) ) ) 
 REPRESENTATION_ITEM ( '' )  SURFACE ( )  );
#25338 = CARTESIAN_POINT ( 'NONE',  ( 106.7886751345947403, -1.999999999999946265, 0.000000000000000000 ) ) ;
#25339 = COLOUR_RGB ( '', 0.31764706, 0.68627451, 0.89019608) ;
#25340 = ORIENTED_EDGE ( 'NONE', *, *, #9149, .F. ) ;
#25341 = ORIENTED_EDGE ( 'NONE', *, *, #20324, .F. ) ;
#25342 = CARTESIAN_POINT ( 'NONE',  ( 142.2187500000000284, 2.485281374238555774, -6.000000000000005329 ) ) ;
#25343 =( BOUNDED_CURVE ( )  B_SPLINE_CURVE ( 2, ( #26100, #7506, #14474, #26245, #12171, #9831, #21516, #442, #5198 ),
 .UNSPECIFIED., .F., .T. ) 
 B_SPLINE_CURVE_WITH_KNOTS ( ( 3, 2, 2, 2, 3 ),
 ( 0.6694444444444445086, 0.6703703703703703942, 0.6722222222222222765, 0.6740740740740740478, 0.6750000000000000444 ),
 .UNSPECIFIED. ) 
 CURVE ( )  GEOMETRIC_REPRESENTATION_ITEM ( )  RATIONAL_B_SPLINE_CURVE ( ( 0.9330127018922194093, 0.9330127018922234061, 1.000000000000000000, 0.8660254037844388186, 1.000000000000000000, 0.8660254037844388186, 1.000000000000000000, 0.9330127018922154125, 0.9330127018922194093 ) ) 
 REPRESENTATION_ITEM ( '' )  );
#25344 = CARTESIAN_POINT ( 'NONE',  ( 2.775557561562891351E-14, 6.250000000000033751, -151.0669872981078470 ) ) ;
#25345 = FILL_AREA_STYLE_COLOUR ( '', #9665 ) ;
#25346 = EDGE_CURVE ( 'NONE', #5496, #23148, #734, .T. ) ;
#25347 = DIRECTION ( 'NONE',  ( -0.000000000000000000, -0.000000000000000000, -1.000000000000000000 ) ) ;
#25348 = PRODUCT_DEFINITION_SHAPE ( 'NONE', 'NONE',  #30420 ) ;
#25349 = VECTOR ( 'NONE', #28320, 1000.000000000000000 ) ;
#25350 = CARTESIAN_POINT ( 'NONE',  ( 21.12500000000011724, 1.414213562373201061, 1.414213562373034527 ) ) ;
#25351 = DIRECTION ( 'NONE',  ( -1.000000000000000000, -1.665334536937731113E-16, 1.526556658859586792E-16 ) ) ;
#25352 = VECTOR ( 'NONE', #6583, 1000.000000000000000 ) ;
#25353 = CARTESIAN_POINT ( 'NONE',  ( 117.4613248654050750, 5.551115123125782702E-14, -2.000000000000001776 ) ) ;
#25354 = CARTESIAN_POINT ( 'NONE',  ( -5.412658773652739619, 3.124999999999975131, -67.68301270189225249 ) ) ;
#25355 = CARTESIAN_POINT ( 'NONE',  ( 141.6413997308104058, 2.071067811865468400, -4.999999999999989342 ) ) ;
#25356 = CARTESIAN_POINT ( 'NONE',  ( 6.000000000000052403, -1.607695154586662678, -124.6533121635129930 ) ) ;
#25357 = CARTESIAN_POINT ( 'NONE',  ( 12.53867513459494631, 1.110223024625156540E-13, 2.500000000000002220 ) ) ;
#25358 = LINE ( 'NONE', #25517, #21738 ) ;
#25359 = PLANE ( 'NONE',  #26785 ) ;
#25360 = CARTESIAN_POINT ( 'NONE',  ( 110.1249999999998437, 1.767766952966265404, 1.767766952966431937 ) ) ;
#25361 = CARTESIAN_POINT ( 'NONE',  ( -3.464101615137757051, -5.999999999999979572, -95.08632486540521711 ) ) ;
#25362 = EDGE_CURVE ( 'NONE', #14907, #17914, #29796, .T. ) ;
#25363 = CARTESIAN_POINT ( 'NONE',  ( -4.763139720814407951, 2.749999999999946709, -121.2500000000000284 ) ) ;
#25365 = CARTESIAN_POINT ( 'NONE',  ( -5.196152422706573404, -3.000000000000002665, -92.78867513459482552 ) ) ;
#25364 = CIRCLE ( 'NONE', #9716, 1.000000000000001554 ) ;
#25366 = CARTESIAN_POINT ( 'NONE',  ( 3.608439182435180470, -6.249999999999997335, -143.5580127018922667 ) ) ;
#25367 =( LENGTH_UNIT ( ) NAMED_UNIT ( * ) SI_UNIT ( .MILLI., .METRE. ) );
#25368 = CARTESIAN_POINT ( 'NONE',  ( 5.999999999999974243, 1.607695154586759934, -143.0966878364870354 ) ) ;
#25369 = VERTEX_POINT ( 'NONE', #20242 ) ;
#25370 = CARTESIAN_POINT ( 'NONE',  ( 3.175426480543072749, -5.500000000000105693, -57.62500000000004974 ) ) ;
#25371 = CARTESIAN_POINT ( 'NONE',  ( -5.999999999999962697, 3.323446944526963260E-14, -155.3363248654052313 ) ) ;
#25372 = CARTESIAN_POINT ( 'NONE',  ( -5.196152422706573404, -3.000000000000002665, -77.21132486540521711 ) ) ;
#25373 = EDGE_LOOP ( 'NONE', ( #1428, #11091, #6702, #760 ) ) ;
#25374 = CARTESIAN_POINT ( 'NONE',  ( 105.2499999999999147, -2.775557561562891351E-14, 2.499999999999946709 ) ) ;
#25375 = TOROIDAL_SURFACE ( 'NONE', #355, 13.00000000000000178, 1.000000000000000000 ) ;
#25376 = CARTESIAN_POINT ( 'NONE',  ( 139.3125000000000284, 4.242640687119298093, -4.242640687119298093 ) ) ;
#25377 = CARTESIAN_POINT ( 'NONE',  ( 13.06249999999998046, 2.000000000000151879, 0.8284271247461152399 ) ) ;
#25378 = DIRECTION ( 'NONE',  ( 1.000000000000000000, -0.000000000000000000, -0.000000000000000000 ) ) ;
#25379 = VECTOR ( 'NONE', #10443, 1000.000000000000000 ) ;
#25380 = CARTESIAN_POINT ( 'NONE',  ( 139.2187500000000000, 2.485281374238555774, -6.000000000000005329 ) ) ;
#25381 = CARTESIAN_POINT ( 'NONE',  ( 14.46132486540527218, 5.551115123125782702E-14, -2.500000000000057732 ) ) ;
#25382 = ORIENTED_EDGE ( 'NONE', *, *, #5471, .F. ) ;
#25383 = CARTESIAN_POINT ( 'NONE',  ( -2.775557561562891351E-14, -5.500000000000115463, -137.2499999999999716 ) ) ;
#25384 = VERTEX_POINT ( 'NONE', #20080 ) ;
#25385 = CARTESIAN_POINT ( 'NONE',  ( 14.62500000000008171, -1.414213562372979016, -1.414213562373145550 ) ) ;
#25386 = ORIENTED_EDGE ( 'NONE', *, *, #3016, .T. ) ;
#25387 = ADVANCED_FACE ( 'NONE', ( #22231 ), #29423, .T. ) ;
#25388 = CARTESIAN_POINT ( 'NONE',  ( 4.763139720814407951, -2.749999999999988454, -63.50000000000000000 ) ) ;
#25389 = CARTESIAN_POINT ( 'NONE',  ( 18.41367513459493566, 1.767766952966598470, 1.767766952966320915 ) ) ;
#25390 = CARTESIAN_POINT ( 'NONE',  ( 7.216878364870455975, -6.409875621278545621E-14, -89.30801270189223828 ) ) ;
#25391 = CARTESIAN_POINT ( 'NONE',  ( 3.464101615137757051, -5.999999999999979572, -113.4136751345948113 ) ) ;
#25392 = FACE_OUTER_BOUND ( 'NONE', #18892, .T. ) ;
#25393 = CARTESIAN_POINT ( 'NONE',  ( 118.0002832217622171, -1.308140751793612777, -1.308140751793418488 ) ) ;
#25394 = EDGE_CURVE ( 'NONE', #12934, #14826, #10289, .T. ) ;
#25395 = PRODUCT_CONTEXT ( 'NONE', #25767, 'mechanical' ) ;
#25396 =( GEOMETRIC_REPRESENTATION_CONTEXT ( 3 ) GLOBAL_UNCERTAINTY_ASSIGNED_CONTEXT ( ( #2564 ) ) GLOBAL_UNIT_ASSIGNED_CONTEXT ( ( #28419, #2775, #28564 ) ) REPRESENTATION_CONTEXT ( 'NONE', 'WORKASPACE' ) );
#25397 = CARTESIAN_POINT ( 'NONE',  ( 4.763139720814407951, -2.749999999999988454, -152.0000000000000284 ) ) ;
#25398 = CARTESIAN_POINT ( 'NONE',  ( 139.5000000000000000, -9.165151389911695645, 8.000000000000007105 ) ) ;
#25399 = CARTESIAN_POINT ( 'NONE',  ( -4.763139720814407951, 2.749999999999946709, -142.2500000000000000 ) ) ;
#25400 = CARTESIAN_POINT ( 'NONE',  ( 3.608439182435180470, 6.249999999999982236, -161.0580127018921814 ) ) ;
#25401 = CARTESIAN_POINT ( 'NONE',  ( -0.2003331987396294867, -9.399833400630225100, 4.385453238887281557 ) ) ;
#25402 = CARTESIAN_POINT ( 'NONE',  ( -3.175426480542816066, 5.499999999999865885, -80.87500000000002842 ) ) ;
#25403 = SURFACE_STYLE_USAGE ( .BOTH. , #6679 ) ;
#25404 = CARTESIAN_POINT ( 'NONE',  ( 6.350852961086080661, -9.614813431917819062E-14, -72.37499999999998579 ) ) ;
#25405 = CARTESIAN_POINT ( 'NONE',  ( 147.2961002691896510, 2.071067811865468400, -4.999999999999989342 ) ) ;
#25406 = CARTESIAN_POINT ( 'NONE',  ( 9.999999999999841904, 2.000000000000057288, -4.274358644806852681E-12 ) ) ;
#25407 = DIRECTION ( 'NONE',  ( 5.551115123125785167E-17, -1.000000000000000000, -8.881784197001256268E-16 ) ) ;
#25408 = CARTESIAN_POINT ( 'NONE',  ( 157.6875000000000284, 4.242640687119269671, 4.242640687119298093 ) ) ;
#25409 = SURFACE_SIDE_STYLE ('',( #18996 ) ) ;
#25410 = CARTESIAN_POINT ( 'NONE',  ( 20.87500000000014211, 1.414213562373367594, -1.414213562373145550 ) ) ;
#25411 = CARTESIAN_POINT ( 'NONE',  ( 0.000000000000000000, 5.999999999999977796, -94.78867513459482552 ) ) ;
#25412 = CARTESIAN_POINT ( 'NONE',  ( 119.5622167782373708, 1.849990392679621953, -0.7662911109075283278 ) ) ;
#25413 = CARTESIAN_POINT ( 'NONE',  ( 130.0000000000000284, -60.00000000000001421, -3.000000000000002665 ) ) ;
#25414 = ORIENTED_EDGE ( 'NONE', *, *, #12706, .F. ) ;
#25415 = CARTESIAN_POINT ( 'NONE',  ( 154.2187500000000284, 2.485281374238555774, -6.000000000000005329 ) ) ;
#25416 =( NAMED_UNIT ( * ) SI_UNIT ( $, .STERADIAN. ) SOLID_ANGLE_UNIT ( ) );
#25417 = CARTESIAN_POINT ( 'NONE',  ( 11.89882486540525797, 1.035533905932749299, 2.499999999999964473 ) ) ;
#25418 = VERTEX_POINT ( 'NONE', #11031 ) ;
#25419 = ORIENTED_EDGE ( 'NONE', *, *, #27497, .T. ) ;
#25420 = ORIENTED_EDGE ( 'NONE', *, *, #7595, .F. ) ;
#25421 = EDGE_CURVE ( 'NONE', #17415, #765, #22030, .T. ) ;
#25422 = CARTESIAN_POINT ( 'NONE',  ( -4.763139720814407951, 2.749999999999946709, -91.25000000000005684 ) ) ;
#25423 = CARTESIAN_POINT ( 'NONE',  ( -5.412658773652684552, -3.125000000000099920, -106.4330127018922667 ) ) ;
#25424 = ORIENTED_EDGE ( 'NONE', *, *, #23285, .F. ) ;
#25425 = DIRECTION ( 'NONE',  ( -1.000000000000000000, 0.000000000000000000, 0.000000000000000000 ) ) ;
#25426 = LINE ( 'NONE', #6851, #17480 ) ;
#25427 = CARTESIAN_POINT ( 'NONE',  ( 3.978158145384761202, -10.25965056898453653, -29.50791791133373820 ) ) ;
#25428 = ORIENTED_EDGE ( 'NONE', *, *, #18645, .F. ) ;
#25429 = CARTESIAN_POINT ( 'NONE',  ( 0.000000000000000000, 5.999999999999977796, -93.28867513459482552 ) ) ;
#25430 = EDGE_CURVE ( 'NONE', #10812, #30268, #20571, .T. ) ;
#25431 = CARTESIAN_POINT ( 'NONE',  ( 109.2886751345947971, 2.000000000000057288, 1.110223024625156540E-13 ) ) ;
#25432 =( BOUNDED_CURVE ( )  B_SPLINE_CURVE ( 2, ( #12183, #21069, #7515, #26107, #21670, #16926, #19368, #19216, #2755 ),
 .UNSPECIFIED., .F., .T. ) 
 B_SPLINE_CURVE_WITH_KNOTS ( ( 3, 2, 2, 2, 3 ),
 ( 0.7656250000000000000, 0.7734375000000000000, 0.7812500000000000000, 0.7890625000000000000, 0.7968750000000000000 ),
 .UNSPECIFIED. ) 
 CURVE ( )  GEOMETRIC_REPRESENTATION_ITEM ( )  RATIONAL_B_SPLINE_CURVE ( ( 1.000000000000000000, 0.9238795325112867385, 1.000000000000000000, 0.9238795325112867385, 1.000000000000000000, 0.9238795325112867385, 1.000000000000000000, 0.9238795325112867385, 1.000000000000000000 ) ) 
 REPRESENTATION_ITEM ( '' )  );
#25433 = CARTESIAN_POINT ( 'NONE',  ( 3.175426480543072749, -5.500000000000105693, -171.6250000000000000 ) ) ;
#25434 = CARTESIAN_POINT ( 'NONE',  ( 6.000000000000000888, 7.762456499804235646E-14, -127.5863248654052171 ) ) ;
#25435 = CARTESIAN_POINT ( 'NONE',  ( 4.763139720814407951, -2.749999999999988454, -162.5000000000000284 ) ) ;
#25436 = CARTESIAN_POINT ( 'NONE',  ( 115.8749999999998579, 1.767766952966431937, -1.767766952966320915 ) ) ;
#25437 = CARTESIAN_POINT ( 'NONE',  ( 0.000000000000000000, 5.499999999999991118, -105.0000000000000426 ) ) ;
#25438 =( NAMED_UNIT ( * ) SI_UNIT ( $, .STERADIAN. ) SOLID_ANGLE_UNIT ( ) );
#25439 = CARTESIAN_POINT ( 'NONE',  ( -5.999999999999956479, -1.607695154586745057, -166.3466878364870354 ) ) ;
#25440 = CARTESIAN_POINT ( 'NONE',  ( 4.763139720814407951, -2.749999999999988454, -96.50000000000002842 ) ) ;
#25441 = CARTESIAN_POINT ( 'NONE',  ( 160.9836002691896226, 4.999999999999989342, -2.071067811865468400 ) ) ;
#25442 = CARTESIAN_POINT ( 'NONE',  ( 0.7911096625681925953, -15.46436038730320206, 8.191759848737534710 ) ) ;
#25443 = ORIENTED_EDGE ( 'NONE', *, *, #10810, .T. ) ;
#25444 = CARTESIAN_POINT ( 'NONE',  ( 13.06250000000007105, -2.649519052838178457, 1.097466725451439196 ) ) ;
#25445 = CARTESIAN_POINT ( 'NONE',  ( 116.9999999999999005, 2.500000000000057732, 1.110223024625156540E-13 ) ) ;
#25446 = LINE ( 'NONE', #30219, #5542 ) ;
#25447 = CARTESIAN_POINT ( 'NONE',  ( 108.5002832217622313, 1.308140751793696044, 1.308140751793640533 ) ) ;
#25448 = CARTESIAN_POINT ( 'NONE',  ( 6.000000000000000888, 1.743066579297358182E-13, -103.5863248654052171 ) ) ;
#25449 = ORIENTED_EDGE ( 'NONE', *, *, #11257, .F. ) ;
#25450 = SURFACE_STYLE_USAGE ( .BOTH. , #4262 ) ;
#25451 = CARTESIAN_POINT ( 'NONE',  ( 105.6872167782375413, 1.849990392679591977, 0.7662911109080692285 ) ) ;
#25452 = CARTESIAN_POINT ( 'NONE',  ( -3.608439182435052128, -6.250000000000110134, -85.94198729810781856 ) ) ;
#25453 = VERTEX_POINT ( 'NONE', #10565 ) ;
#25454 = CARTESIAN_POINT ( 'NONE',  ( 140.5384615384615756, -11.53846153846155254, 4.807692307692318145 ) ) ;
#25455 = ORIENTED_EDGE ( 'NONE', *, *, #977, .T. ) ;
#25456 = CARTESIAN_POINT ( 'NONE',  ( 149.0625000000000284, -4.242640687119298093, 4.242640687119298093 ) ) ;
#25457 = ORIENTED_EDGE ( 'NONE', *, *, #27363, .T. ) ;
#25458 = EDGE_CURVE ( 'NONE', #29150, #1827, #29268, .T. ) ;
#25459 = CARTESIAN_POINT ( 'NONE',  ( -4.763139720814407951, -2.750000000000016431, -125.5000000000000568 ) ) ;
#25460 = COLOUR_RGB ( '', 0.08235294, 0.09019608, 0.10196078) ;
#25461 = CARTESIAN_POINT ( 'NONE',  ( 22.56250000000008527, 1.097466725451679892, 2.649519052838298805 ) ) ;
#25462 = EDGE_CURVE ( 'NONE', #18067, #14341, #3858, .T. ) ;
#25463 = CARTESIAN_POINT ( 'NONE',  ( -3.608439182435052128, -6.250000000000110134, -127.3080127018922383 ) ) ;
#25464 = EDGE_LOOP ( 'NONE', ( #14073, #15584, #490, #6870 ) ) ;
#25465 = CARTESIAN_POINT ( 'NONE',  ( -5.196152422706601826, 2.999999999999975131, -57.03867513459481842 ) ) ;
#25466 = CARTESIAN_POINT ( 'NONE',  ( 5.412658773652739619, 3.124999999999988898, -166.3169872981078470 ) ) ;
#25467 = CARTESIAN_POINT ( 'NONE',  ( -3.608439182435115633, 6.249999999999965361, -179.4419872981078470 ) ) ;
#25468 = CARTESIAN_POINT ( 'NONE',  ( 160.0292075518898116, -11.64910390351806946, 2.883065298126458398 ) ) ;
#25469 = CARTESIAN_POINT ( 'NONE',  ( 0.000000000000000000, 0.000000000000000000, 0.000000000000000000 ) ) ;
#25470 = VERTEX_POINT ( 'NONE', #24674 ) ;
#25471 = CARTESIAN_POINT ( 'NONE',  ( 11.18750000000003908, 0.8284271247462955401, 2.000000000000031530 ) ) ;
#25472 = CYLINDRICAL_SURFACE ( 'NONE', #8943, 6.000000000000000888 ) ;
#25473 = CARTESIAN_POINT ( 'NONE',  ( -5.999999999999944933, 1.607695154586759934, -136.4806624327025872 ) ) ;
#25474 = CARTESIAN_POINT ( 'NONE',  ( 112.7113248654049897, 2.000000000000057288, 0.000000000000000000 ) ) ;
#25475 = CARTESIAN_POINT ( 'NONE',  ( 112.1252832217621460, -5.551115123125782702E-14, -1.849990392679523588 ) ) ;
#25476 = CARTESIAN_POINT ( 'NONE',  ( 5.412658773652739619, 3.124999999999988898, -74.81698729810781856 ) ) ;
#25477 = CARTESIAN_POINT ( 'NONE',  ( -2.775557561562891351E-14, -5.500000000000115463, -50.25000000000001421 ) ) ;
#25478 = CARTESIAN_POINT ( 'NONE',  ( -0.6046674458933889440, -9.395332554106687439, -4.067501169440991049 ) ) ;
#25479 = CARTESIAN_POINT ( 'NONE',  ( -3.464101615137757051, -5.999999999999979572, -47.66367513459483973 ) ) ;
#25480 = CARTESIAN_POINT ( 'NONE',  ( -5.196152422706601826, 2.999999999999975131, -123.0386751345948255 ) ) ;
#25481 = CARTESIAN_POINT ( 'NONE',  ( 3.175426480543072749, -5.500000000000105693, -122.1250000000000284 ) ) ;
#25482 = CARTESIAN_POINT ( 'NONE',  ( 135.4072480194323020, -8.806439873276080021, -8.023362806821699778 ) ) ;
#25483 = CARTESIAN_POINT ( 'NONE',  ( 114.2886751345947971, 2.000000000000029310, 1.110223024625156540E-13 ) ) ;
#25484 = ORIENTED_EDGE ( 'NONE', *, *, #362, .T. ) ;
#25485 = CARTESIAN_POINT ( 'NONE',  ( 19.50000000000009948, 1.873492889145067508, -1.873492889145067508 ) ) ;
#25486 =( BOUNDED_CURVE ( )  B_SPLINE_CURVE ( 2, ( #9237, #27950, #25196, #21228, #23082, #28109, #21079, #9552, #23238 ),
 .UNSPECIFIED., .F., .F. ) 
 B_SPLINE_CURVE_WITH_KNOTS ( ( 3, 2, 2, 2, 3 ),
 ( 0.3472222222222222099, 0.3481481481481480955, 0.3499999999999999778, 0.3518518518518518601, 0.3527777777777778567 ),
 .UNSPECIFIED. ) 
 CURVE ( )  GEOMETRIC_REPRESENTATION_ITEM ( )  RATIONAL_B_SPLINE_CURVE ( ( 0.9330127018922194093, 0.9330127018922194093, 1.000000000000000000, 0.8660254037844388186, 1.000000000000000000, 0.8660254037844388186, 1.000000000000000000, 0.9330127018922154125, 0.9330127018922194093 ) ) 
 REPRESENTATION_ITEM ( '' )  );
#25487 = AXIS2_PLACEMENT_3D ( 'NONE', #28780, #24329, #5586 ) ;
#25488 = CARTESIAN_POINT ( 'NONE',  ( -3.464101615137725076, 5.999999999999979572, -105.1636751345948539 ) ) ;
#25489 = CARTESIAN_POINT ( 'NONE',  ( 116.3511751345946408, 2.000000000000061728, 0.8284271247464157772 ) ) ;
#25490 = AXIS2_PLACEMENT_3D ( 'NONE', #30178, #18535, #27861 ) ;
#25491 = VERTEX_POINT ( 'NONE', #22542 ) ;
#25492 = CARTESIAN_POINT ( 'NONE',  ( 109.6247167782375840, 1.849990392679634610, 1.110223024625156540E-13 ) ) ;
#25493 = LINE ( 'NONE', #2169, #18716 ) ;
#25494 = CARTESIAN_POINT ( 'NONE',  ( 112.8122167782374419, 0.7662911109079189043, 1.849990392679772278 ) ) ;
#25495 = AXIS2_PLACEMENT_3D ( 'NONE', #11739, #9556, #28114 ) ;
#25496 = CARTESIAN_POINT ( 'NONE',  ( -7.216878364870328078, 0.000000000000000000, -110.1919872981078043 ) ) ;
#25497 = CARTESIAN_POINT ( 'NONE',  ( -5.999999999999963585, -2.788906526875773208E-15, -176.9136751345948539 ) ) ;
#25498 = CARTESIAN_POINT ( 'NONE',  ( 10.00000000000012079, -0.6095397823829284967, 2.424553825692621345 ) ) ;
#25499 = ORIENTED_EDGE ( 'NONE', *, *, #2322, .T. ) ;
#25500 = VERTEX_POINT ( 'NONE', #1476 ) ;
#25501 = CARTESIAN_POINT ( 'NONE',  ( 14.53867513459486460, 1.665334536937734811E-13, 2.499999999999835687 ) ) ;
#25502 = CARTESIAN_POINT ( 'NONE',  ( 137.3437500000000568, -6.000000000000005329, -2.485281374238555774 ) ) ;
#25503 = EDGE_CURVE ( 'NONE', #20245, #16482, #16309, .T. ) ;
#25504 = ADVANCED_FACE ( 'NONE', ( #29734 ), #3616, .T. ) ;
#25505 = CARTESIAN_POINT ( 'NONE',  ( 2.775557561562891351E-14, 6.250000000000033751, -142.0669872981078470 ) ) ;
#25506 = FACE_OUTER_BOUND ( 'NONE', #26333, .T. ) ;
#25507 = CARTESIAN_POINT ( 'NONE',  ( -5.999999999999962697, 3.323446944526963260E-14, -150.8363248654052029 ) ) ;
#25508 = STYLED_ITEM ( 'NONE', ( #3813 ), #27288 ) ;
#25509 = CARTESIAN_POINT ( 'NONE',  ( 21.68750000000000711, -0.8284271247461753029, -2.000000000000031530 ) ) ;
#25510 = DIRECTION ( 'NONE',  ( -1.000000000000000000, 0.000000000000000000, 0.000000000000000000 ) ) ;
#25511 = CARTESIAN_POINT ( 'NONE',  ( 2.775557561562891351E-14, 6.250000000000033751, -67.93301270189222407 ) ) ;
#25512 = CARTESIAN_POINT ( 'NONE',  ( 135.4056618780774386, -8.496329914198520683, -8.215405480166896979 ) ) ;
#25513 = AXIS2_PLACEMENT_3D ( 'NONE', #8910, #11550, #21454 ) ;
#25514 = CARTESIAN_POINT ( 'NONE',  ( 146.7976497308104058, 0.000000000000000000, 5.000000000000004441 ) ) ;
#25515 = CARTESIAN_POINT ( 'NONE',  ( 11.66367513459487526, -1.767766952966265404, 1.767766952966376426 ) ) ;
#25516 = CARTESIAN_POINT ( 'NONE',  ( 6.000000000000000888, 1.743066579297358182E-13, -74.16367513459483973 ) ) ;
#25517 = CARTESIAN_POINT ( 'NONE',  ( -6.000000000000000888, 1.067854986875958443E-15, 7.560779664488942560E-35 ) ) ;
#25518 = CARTESIAN_POINT ( 'NONE',  ( 156.1949251345949108, 5.500000000000012434, -2.278174593052012309 ) ) ;
#25519 = DIRECTION ( 'NONE',  ( -1.000000000000000000, -1.665334536937731113E-16, 1.526556658859586792E-16 ) ) ;
#25520 = CARTESIAN_POINT ( 'NONE',  ( 109.7499999999999147, 5.551115123125782702E-14, -2.499999999999835687 ) ) ;
#25521 = CARTESIAN_POINT ( 'NONE',  ( 0.000000000000000000, -5.999999999999991118, -94.96132486540520290 ) ) ;
#25522 = CARTESIAN_POINT ( 'NONE',  ( -3.175426480542816066, 5.499999999999865885, -124.3749999999999858 ) ) ;
#25523 = PRODUCT_DEFINITION_CONTEXT ( 'detailed design', #4179, 'design' ) ;
#25524 = CARTESIAN_POINT ( 'NONE',  ( 5.412658773652739619, 3.124999999999988898, -146.1830127018922667 ) ) ;
#25525 = FILL_AREA_STYLE ('',( #21657 ) ) ;
#25526 = VERTEX_POINT ( 'NONE', #28295 ) ;
#25527 = CARTESIAN_POINT ( 'NONE',  ( 4.763139720814407951, 2.750000000000002665, -58.75000000000002132 ) ) ;
#25528 = CARTESIAN_POINT ( 'NONE',  ( 0.000000000000000000, 0.000000000000000000, 0.000000000000000000 ) ) ;
#25529 = DIRECTION ( 'NONE',  ( -8.326672684688675286E-17, -2.081668171172168821E-17, 1.000000000000000000 ) ) ;
#25530 =( BOUNDED_CURVE ( )  B_SPLINE_CURVE ( 2, ( #22867, #8098, #8421, #17826, #27146, #15528, #29610, #24849, #3798 ),
 .UNSPECIFIED., .F., .F. ) 
 B_SPLINE_CURVE_WITH_KNOTS ( ( 3, 2, 2, 2, 3 ),
 ( 0.6472222222222221433, 0.6481481481481481399, 0.6500000000000000222, 0.6518518518518519045, 0.6527777777777777901 ),
 .UNSPECIFIED. ) 
 CURVE ( )  GEOMETRIC_REPRESENTATION_ITEM ( )  RATIONAL_B_SPLINE_CURVE ( ( 0.9330127018922194093, 0.9330127018922114157, 1.000000000000000000, 0.8660254037844388186, 1.000000000000000000, 0.8660254037844388186, 1.000000000000000000, 0.9330127018922194093, 0.9330127018922194093 ) ) 
 REPRESENTATION_ITEM ( '' )  );
#25531 =( NAMED_UNIT ( * ) PLANE_ANGLE_UNIT ( ) SI_UNIT ( $, .RADIAN. ) );
#25532 = ORIENTED_EDGE ( 'NONE', *, *, #3158, .F. ) ;
#25533 = CARTESIAN_POINT ( 'NONE',  ( 107.1874999999997584, 1.035533905932779275, 2.500000000000205169 ) ) ;
#25534 = CARTESIAN_POINT ( 'NONE',  ( 142.9687500000000284, -2.485281374238585972, 6.000000000000005329 ) ) ;
#25535 = CARTESIAN_POINT ( 'NONE',  ( 160.0000000000000284, -12.58710442076092484, -3.130720585662490674 ) ) ;
#25536 = EDGE_CURVE ( 'NONE', #2534, #16280, #11772, .T. ) ;
#25537 = CARTESIAN_POINT ( 'NONE',  ( -5.412658773652684552, -3.125000000000099920, -101.0669872981078186 ) ) ;
#25538 = VECTOR ( 'NONE', #22624, 1000.000000000000000 ) ;
#25539 = CARTESIAN_POINT ( 'NONE',  ( 142.9761751345948255, 3.889087296526011706, 3.889087296526011706 ) ) ;
#25540 =( BOUNDED_CURVE ( )  B_SPLINE_CURVE ( 2, ( #4967, #9454, #23442, #16102, #4367, #16252, #68, #216, #2082 ),
 .UNSPECIFIED., .F., .T. ) 
 B_SPLINE_CURVE_WITH_KNOTS ( ( 3, 2, 2, 2, 3 ),
 ( 0.1972222222222222432, 0.1981481481481481566, 0.2000000000000000111, 0.2018518518518518656, 0.2027777777777777790 ),
 .UNSPECIFIED. ) 
 CURVE ( )  GEOMETRIC_REPRESENTATION_ITEM ( )  RATIONAL_B_SPLINE_CURVE ( ( 0.9330127018922194093, 0.9330127018922204085, 1.000000000000000000, 0.8660254037844388186, 1.000000000000000000, 0.8660254037844388186, 1.000000000000000000, 0.9330127018922194093, 0.9330127018922194093 ) ) 
 REPRESENTATION_ITEM ( '' )  );
#25541 = CARTESIAN_POINT ( 'NONE',  ( 134.2500000000000284, -6.000000000000005329, 0.000000000000000000 ) ) ;
#25542 = CARTESIAN_POINT ( 'NONE',  ( 14.27382486540519402, -2.499999999999964473, -1.035533905932749299 ) ) ;
#25543 = CARTESIAN_POINT ( 'NONE',  ( -4.763139720814407951, -2.750000000000016431, -137.5000000000000000 ) ) ;
#25544 = EDGE_CURVE ( 'NONE', #10998, #6626, #5829, .T. ) ;
#25545 = AXIS2_PLACEMENT_3D ( 'NONE', #23124, #27689, #5258 ) ;
#25546 = CARTESIAN_POINT ( 'NONE',  ( 11.75000000000012079, 1.665334536937734811E-13, -2.000000000000057288 ) ) ;
#25547 = ORIENTED_EDGE ( 'NONE', *, *, #26734, .F. ) ;
#25548 = CARTESIAN_POINT ( 'NONE',  ( -4.763139720814407951, -2.750000000000016431, -67.00000000000000000 ) ) ;
#25549 = CARTESIAN_POINT ( 'NONE',  ( 18.35117513459491434, 2.500000000000144773, 1.035533905932689347 ) ) ;
#25550 = CARTESIAN_POINT ( 'NONE',  ( 5.412658773652712085, -3.125000000000086153, -89.43301270189223828 ) ) ;
#25551 = CARTESIAN_POINT ( 'NONE',  ( 155.0699251345948255, 2.278174593052198382, 5.499999999999826805 ) ) ;
#25552 = CARTESIAN_POINT ( 'NONE',  ( 107.3747167782375840, -5.551115123125782702E-14, -1.849990392679523588 ) ) ;
#25553 = CARTESIAN_POINT ( 'NONE',  ( 140.2902754521815041, -11.64513772609104159, -4.288736938852963476 ) ) ;
#25554 = AXIS2_PLACEMENT_3D ( 'NONE', #21752, #12407, #26474 ) ;
#25555 = DIRECTION ( 'NONE',  ( -8.326672684688675286E-17, -2.081668171172168821E-17, 1.000000000000000000 ) ) ;
#25556 = CARTESIAN_POINT ( 'NONE',  ( 117.7502832217623592, -1.308140751793585022, 1.308140751793862577 ) ) ;
#25557 = CARTESIAN_POINT ( 'NONE',  ( -6.350852961085760029, -1.281975124255709124E-13, -145.1250000000000000 ) ) ;
#25558 = CARTESIAN_POINT ( 'NONE',  ( -5.999999999999963585, 8.134310703387671600E-14, -144.8363248654052029 ) ) ;
#25559 = CARTESIAN_POINT ( 'NONE',  ( -2.775557561562891351E-14, -5.500000000000115463, -135.7500000000000284 ) ) ;
#25560 = AXIS2_PLACEMENT_3D ( 'NONE', #26249, #9691, #21521 ) ;
#25561 = CARTESIAN_POINT ( 'NONE',  ( 7.216878364870455975, -6.409875621278545621E-14, -158.3080127018922667 ) ) ;
#25562 = CARTESIAN_POINT ( 'NONE',  ( -5.999999999999963585, 8.134310703387671600E-14, -116.3363248654052313 ) ) ;
#25563 = CARTESIAN_POINT ( 'NONE',  ( 105.5863248654051034, 1.414213562373090038, -1.414213562373145550 ) ) ;
#25564 = CIRCLE ( 'NONE', #20189, 1.000000000000000000 ) ;
#25565 = CARTESIAN_POINT ( 'NONE',  ( 4.763139720814407951, 2.750000000000002665, -78.25000000000004263 ) ) ;
#25566 = CARTESIAN_POINT ( 'NONE',  ( 117.1488248654051176, -1.999999999999971800, 0.8284271247462955401 ) ) ;
#25567 = CARTESIAN_POINT ( 'NONE',  ( 6.350852961086080661, -9.614813431917819062E-14, -73.87500000000000000 ) ) ;
#25568 = CARTESIAN_POINT ( 'NONE',  ( 0.000000000000000000, -5.999999999999991118, -156.4613248654052029 ) ) ;
#25569 = CARTESIAN_POINT ( 'NONE',  ( 149.8273502691896510, -5.000000000000004441, 0.000000000000000000 ) ) ;
#25570 = CARTESIAN_POINT ( 'NONE',  ( -27.00000000000002487, 2.678141147339112567E-16, 4.000000000000010658 ) ) ;
#25571 = CYLINDRICAL_SURFACE ( 'NONE', #18929, 6.000000000000000888 ) ;
#25572 = AXIS2_PLACEMENT_3D ( 'NONE', #22825, #13190, #22673 ) ;
#25573 = EDGE_CURVE ( 'NONE', #30412, #30347, #23715, .T. ) ;
#25574 = STYLED_ITEM ( 'NONE', ( #10500 ), #23989 ) ;
#25575 = CARTESIAN_POINT ( 'NONE',  ( 159.9375000000000284, -4.242640687119298093, -4.242640687119298093 ) ) ;
#25576 = CARTESIAN_POINT ( 'NONE',  ( 19.25000000000009948, 1.110223024625156540E-13, 1.999999999999946265 ) ) ;
#25577 = EDGE_CURVE ( 'NONE', #2682, #18067, #21114, .T. ) ;
#25578 = DIRECTION ( 'NONE',  ( -1.000000000000000000, -1.665334536937731113E-16, 1.526556658859586792E-16 ) ) ;
#25579 = CARTESIAN_POINT ( 'NONE',  ( -5.999999999999963585, 1.780251999655701777E-13, -98.91367513459483973 ) ) ;
#25580 = CARTESIAN_POINT ( 'NONE',  ( 116.9372167782374845, -0.7662911109078588412, 1.849990392679652151 ) ) ;
#25581 = SURFACE_STYLE_FILL_AREA ( #23146 ) ;
#25582 = ORIENTED_EDGE ( 'NONE', *, *, #29874, .F. ) ;
#25583 = CARTESIAN_POINT ( 'NONE',  ( 156.9375000000000284, -4.242640687119298093, -4.242640687119298093 ) ) ;
#25584 =( BOUNDED_CURVE ( )  B_SPLINE_CURVE ( 2, ( #11741, #16204, #25515, #23394, #9242, #21084, #13903, #16055, #21234 ),
 .UNSPECIFIED., .F., .F. ) 
 B_SPLINE_CURVE_WITH_KNOTS ( ( 3, 2, 2, 2, 3 ),
 ( 0.1093750000000000000, 0.1171875000000000000, 0.1250000000000000000, 0.1328125000000000000, 0.1406250000000000000 ),
 .UNSPECIFIED. ) 
 CURVE ( )  GEOMETRIC_REPRESENTATION_ITEM ( )  RATIONAL_B_SPLINE_CURVE ( ( 1.000000000000000000, 0.9238795325112867385, 1.000000000000000000, 0.9238795325112867385, 1.000000000000000000, 0.9238795325112867385, 1.000000000000000000, 0.9238795325112867385, 1.000000000000000000 ) ) 
 REPRESENTATION_ITEM ( '' )  );
#25585 = VECTOR ( 'NONE', #10783, 1000.000000000000000 ) ;
#25586 = CARTESIAN_POINT ( 'NONE',  ( 6.000000000000000888, -1.859271017917181981E-14, -84.66367513459482552 ) ) ;
#25587 = ORIENTED_EDGE ( 'NONE', *, *, #12299, .F. ) ;
#25588 = ORIENTED_EDGE ( 'NONE', *, *, #22890, .F. ) ;
#25589 = EDGE_CURVE ( 'NONE', #691, #25181, #23570, .T. ) ;
#25590 = EDGE_CURVE ( 'NONE', #13194, #20580, #7114, .T. ) ;
#25591 = VECTOR ( 'NONE', #5042, 1000.000000000000000 ) ;
#25592 = ORIENTED_EDGE ( 'NONE', *, *, #4629, .T. ) ;
#25593 = CARTESIAN_POINT ( 'NONE',  ( 3.175426480543072749, 5.499999999999865885, -90.12500000000001421 ) ) ;
#25594 = CARTESIAN_POINT ( 'NONE',  ( 5.412658773652712085, -3.125000000000086153, -104.4330127018922525 ) ) ;
#25595 = ORIENTED_EDGE ( 'NONE', *, *, #21814, .F. ) ;
#25596 = CARTESIAN_POINT ( 'NONE',  ( 5.382374809129858662, 9.594851770513413314, -27.68068691953152083 ) ) ;
#25597 = CARTESIAN_POINT ( 'NONE',  ( 3.464101615137852974, 5.999999999999884537, -52.33632486540523843 ) ) ;
#25598 = AXIS2_PLACEMENT_3D ( 'NONE', #23433, #8838, #18224 ) ;
#25599 = CARTESIAN_POINT ( 'NONE',  ( -2.775557561562891351E-14, -5.500000000000115463, -164.2500000000000000 ) ) ;
#25600 = CARTESIAN_POINT ( 'NONE',  ( -5.412658773652684552, -3.125000000000099920, -47.93301270189220986 ) ) ;
#25601 = VERTEX_POINT ( 'NONE', #12227 ) ;
#25602 =( NAMED_UNIT ( * ) SI_UNIT ( $, .STERADIAN. ) SOLID_ANGLE_UNIT ( ) );
#25603 = CARTESIAN_POINT ( 'NONE',  ( 6.350852961086080661, -9.614813431917819062E-14, -168.3750000000000568 ) ) ;
#25604 = CARTESIAN_POINT ( 'NONE',  ( 23.53867513459495342, 1.665334536937734811E-13, 2.499999999999835687 ) ) ;
#25605 = AXIS2_PLACEMENT_3D ( 'NONE', #13989, #23328, #9334 ) ;
#25606 = CARTESIAN_POINT ( 'NONE',  ( -3.175426480542816510, -5.500000000000057732, -162.8750000000000284 ) ) ;
#25607 = CARTESIAN_POINT ( 'NONE',  ( 111.3124999999998295, -1.035533905932629173, 2.500000000000325517 ) ) ;
#25608 = CIRCLE ( 'NONE', #105, 17.50000000000004619 ) ;
#25609 = CYLINDRICAL_SURFACE ( 'NONE', #2021, 6.000000000000005329 ) ;
#25610 = CARTESIAN_POINT ( 'NONE',  ( -2.775557561562891351E-14, -5.500000000000115463, -98.25000000000000000 ) ) ;
#25611 = CARTESIAN_POINT ( 'NONE',  ( 160.1398502691896510, -3.535533905932752852, 3.535533905932725318 ) ) ;
#25612 = FACE_OUTER_BOUND ( 'NONE', #16046, .T. ) ;
#25613 = ORIENTED_EDGE ( 'NONE', *, *, #1359, .T. ) ;
#25614 = CARTESIAN_POINT ( 'NONE',  ( 11.50000000000014921, 1.873492889145067508, -1.873492889145067508 ) ) ;
#25615 = CARTESIAN_POINT ( 'NONE',  ( 112.6249999999998437, -1.767766952966431937, -1.767766952966320915 ) ) ;
#25616 = EDGE_CURVE ( 'NONE', #5051, #30356, #28590, .T. ) ;
#25617 = CYLINDRICAL_SURFACE ( 'NONE', #1631, 6.000000000000000888 ) ;
#25618 = CARTESIAN_POINT ( 'NONE',  ( 107.3127832217622313, 1.849990392679501827, -0.7662911109076485650 ) ) ;
#25619 = CARTESIAN_POINT ( 'NONE',  ( 129.9999999999998010, -90.00000000000001421, 3.000000000000002665 ) ) ;
#25620 = ORIENTED_EDGE ( 'NONE', *, *, #2557, .F. ) ;
#25621 = CARTESIAN_POINT ( 'NONE',  ( -19.99999999999998224, -54.99999999999990763, -7.500000000000007105 ) ) ;
#25622 = DIRECTION ( 'NONE',  ( -1.000000000000000000, 0.000000000000000000, 0.000000000000000000 ) ) ;
#25623 = CARTESIAN_POINT ( 'NONE',  ( 107.6872167782374561, 1.849990392679562001, 0.7662911109080090544 ) ) ;
#25624 = AXIS2_PLACEMENT_3D ( 'NONE', #1266, #8335, #27069 ) ;
#25625 = ORIENTED_EDGE ( 'NONE', *, *, #22479, .F. ) ;
#25626 = ADVANCED_FACE ( 'NONE', ( #23424 ), #16679, .T. ) ;
#25627 = CARTESIAN_POINT ( 'NONE',  ( 0.000000000000000000, 0.000000000000000000, -180.0000000000000568 ) ) ;
#25628 = EDGE_CURVE ( 'NONE', #14042, #8327, #11306, .T. ) ;
#25629 = ORIENTED_EDGE ( 'NONE', *, *, #5887, .T. ) ;
#25630 = CARTESIAN_POINT ( 'NONE',  ( 151.5937500000000284, 6.000000000000005329, 2.485281374238585972 ) ) ;
#25631 = CARTESIAN_POINT ( 'NONE',  ( -2.775557561562891351E-14, -5.500000000000115463, -110.2500000000000142 ) ) ;
#25632 = CARTESIAN_POINT ( 'NONE',  ( 20.93749999999999289, -2.649519052838238409, -1.097466725451559322 ) ) ;
#25633 =( BOUNDED_CURVE ( )  B_SPLINE_CURVE ( 2, ( #505, #16983, #29528, #5557, #3710, #22015, #22171, #26603, #6601 ),
 .UNSPECIFIED., .F., .T. ) 
 B_SPLINE_CURVE_WITH_KNOTS ( ( 3, 2, 2, 2, 3 ),
 ( 0.1638888888888889728, 0.1648148148148148584, 0.1666666666666666297, 0.1685185185185185119, 0.1694444444444443976 ),
 .UNSPECIFIED. ) 
 CURVE ( )  GEOMETRIC_REPRESENTATION_ITEM ( )  RATIONAL_B_SPLINE_CURVE ( ( 0.9330127018922194093, 0.9330127018922234061, 1.000000000000000000, 0.8660254037844388186, 1.000000000000000000, 0.8660254037844388186, 1.000000000000000000, 0.9330127018922234061, 0.9330127018922194093 ) ) 
 REPRESENTATION_ITEM ( '' )  );
#25634 = CARTESIAN_POINT ( 'NONE',  ( 5.412658773652739619, 3.124999999999988898, -134.1830127018922667 ) ) ;
#25635 = EDGE_LOOP ( 'NONE', ( #6917, #17110, #25298, #29001, #25547, #10739, #13314, #25734, #3870, #8104, #24793, #11217, #13532, #14287, #1626, #21953, #6668, #595, #26543, #20638, #4178, #4765, #14899, #9166, #16306, #4909, #23381, #20851, #11881, #1636, #27937, #3160, #19505, #10982, #27711 ) ) ;
#25636 = CARTESIAN_POINT ( 'NONE',  ( -3.608439182435052128, -6.250000000000110134, -168.4419872981078470 ) ) ;
#25637 = CARTESIAN_POINT ( 'NONE',  ( 3.608439182435180470, 6.249999999999982236, -179.6919872981078186 ) ) ;
#25638 = CARTESIAN_POINT ( 'NONE',  ( 0.5896198263044475363, 5.540201351793478501, -180.0000000000000853 ) ) ;
#25639 = CARTESIAN_POINT ( 'NONE',  ( 0.000000000000000000, 5.999999999999977796, -133.2113248654052029 ) ) ;
#25640 = CARTESIAN_POINT ( 'NONE',  ( 140.0000000000000284, -8.500000000000007105, 8.000000000000007105 ) ) ;
#25641 = CARTESIAN_POINT ( 'NONE',  ( 108.0627832217621034, -0.7662911109077388261, -1.849990392679351725 ) ) ;
#25642 = CARTESIAN_POINT ( 'NONE',  ( -3.608439182435052128, -6.250000000000110134, -60.44198729810782567 ) ) ;
#25643 = CARTESIAN_POINT ( 'NONE',  ( 7.216878364870455975, -6.409875621278545621E-14, -174.8080127018922667 ) ) ;
#25644 = LINE ( 'NONE', #20590, #29801 ) ;
#25645 = CARTESIAN_POINT ( 'NONE',  ( 7.147005652999508048E-33, -5.642372883946980038E-33, -1183.000000000000000 ) ) ;
#25646 = CARTESIAN_POINT ( 'NONE',  ( 3.464101615137852974, 5.999999999999884537, -123.4136751345947829 ) ) ;
#25647 = CARTESIAN_POINT ( 'NONE',  ( 4.763139720814407951, -2.749999999999988454, -117.5000000000000426 ) ) ;
#25648 = CARTESIAN_POINT ( 'NONE',  ( 114.7261751345946976, -1.999999999999881650, 0.8284271247462955401 ) ) ;
#25649 = ORIENTED_EDGE ( 'NONE', *, *, #4663, .T. ) ;
#25650 = CARTESIAN_POINT ( 'NONE',  ( 20.00000000000018474, -1.873492889144789952, 1.873492889144845464 ) ) ;
#25651 = EDGE_CURVE ( 'NONE', #27766, #11375, #22268, .T. ) ;
#25652 = CARTESIAN_POINT ( 'NONE',  ( 3.464101615137852974, 5.999999999999884537, -122.8363248654051745 ) ) ;
#25653 = CYLINDRICAL_SURFACE ( 'NONE', #23641, 6.000000000000000888 ) ;
#25654 = VECTOR ( 'NONE', #25832, 1000.000000000000000 ) ;
#25655 = VERTEX_POINT ( 'NONE', #200 ) ;
#25656 = CARTESIAN_POINT ( 'NONE',  ( 110.9997167782376266, -1.308140751793585022, 1.308140751793640533 ) ) ;
#25657 = CYLINDRICAL_SURFACE ( 'NONE', #27502, 6.000000000000000888 ) ;
#25658 = CARTESIAN_POINT ( 'NONE',  ( -5.412658773652739619, 3.124999999999975131, -110.3169872981077901 ) ) ;
#25659 = CARTESIAN_POINT ( 'NONE',  ( 19.85117513459492145, -2.499999999999904521, -1.035533905932749299 ) ) ;
#25660 = EDGE_CURVE ( 'NONE', #13261, #24590, #9890, .T. ) ;
#25661 = MECHANICAL_DESIGN_GEOMETRIC_PRESENTATION_REPRESENTATION (  '', ( #28575 ), #16855 ) ;
#25662 = DIRECTION ( 'NONE',  ( -7.147005652999508048E-36, 5.642372883946980038E-36, 1.000000000000000000 ) ) ;
#25663 = ORIENTED_EDGE ( 'NONE', *, *, #7099, .T. ) ;
#25664 = ORIENTED_EDGE ( 'NONE', *, *, #3301, .F. ) ;
#25665 = CARTESIAN_POINT ( 'NONE',  ( 19.99999999999998934, 0.000000000000000000, 0.000000000000000000 ) ) ;
#25666 = CARTESIAN_POINT ( 'NONE',  ( 136.0312500000000000, -2.485281374238555774, -6.000000000000005329 ) ) ;
#25667 = CARTESIAN_POINT ( 'NONE',  ( 7.216878364870455975, -6.409875621278545621E-14, -142.4419872981078186 ) ) ;
#25668 = CARTESIAN_POINT ( 'NONE',  ( 9.875000000000078160, -2.649519052838111843, -5.551115123125782702E-14 ) ) ;
#25669 = CARTESIAN_POINT ( 'NONE',  ( 19.87500000000017053, 1.414213562373312083, -1.414213562373145550 ) ) ;
#25670 = DIRECTION ( 'NONE',  ( -7.147005652999508048E-36, 5.642372883946980038E-36, 1.000000000000000000 ) ) ;
#25671 = CARTESIAN_POINT ( 'NONE',  ( 6.000000000000000888, -1.607695154586752384, -137.2306624327026157 ) ) ;
#25672 = CARTESIAN_POINT ( 'NONE',  ( -3.608439182435052128, -6.250000000000110134, -58.30801270189222407 ) ) ;
#25673 = FACE_OUTER_BOUND ( 'NONE', #29220, .T. ) ;
#25674 = AXIS2_PLACEMENT_3D ( 'NONE', #4714, #16141, #25286 ) ;
#25675 = CARTESIAN_POINT ( 'NONE',  ( 142.3913997308104058, -2.071067811865468400, 4.999999999999989342 ) ) ;
#25676 = CARTESIAN_POINT ( 'NONE',  ( 12.60117513459493743, -1.035533905932629173, 2.499999999999844569 ) ) ;
#25677 = DIRECTION ( 'NONE',  ( -7.147005652999508048E-36, 5.642372883946980038E-36, 1.000000000000000000 ) ) ;
#25678 = CARTESIAN_POINT ( 'NONE',  ( 24.76476637266523539, -1.543174358739360041, -1.624092575704163544 ) ) ;
#25679 = CARTESIAN_POINT ( 'NONE',  ( -6.000000000000023093, 1.607695154586625819, -114.9033121635129646 ) ) ;
#25680 = CARTESIAN_POINT ( 'NONE',  ( 108.4374999999999005, -2.499999999999934719, 1.035533905932929599 ) ) ;
#25681 =( BOUNDED_CURVE ( )  B_SPLINE_CURVE ( 2, ( #15633, #27096, #29709, #18078, #27391, #6357, #29860, #28157, #4363 ),
 .UNSPECIFIED., .F., .F. ) 
 B_SPLINE_CURVE_WITH_KNOTS ( ( 3, 2, 2, 2, 3 ),
 ( 0.01944444444444448639, 0.02037037037037037202, 0.02222222222222225430, 0.02407407407407402555, 0.02499999999999991118 ),
 .UNSPECIFIED. ) 
 CURVE ( )  GEOMETRIC_REPRESENTATION_ITEM ( )  RATIONAL_B_SPLINE_CURVE ( ( 0.9330127018922194093, 0.9330127018922234061, 1.000000000000000000, 0.8660254037844388186, 1.000000000000000000, 0.8660254037844388186, 1.000000000000000000, 0.9330127018922234061, 0.9330127018922194093 ) ) 
 REPRESENTATION_ITEM ( '' )  );
#25682 = DIRECTION ( 'NONE',  ( 0.000000000000000000, 0.000000000000000000, 1.000000000000000000 ) ) ;
#25683 = CARTESIAN_POINT ( 'NONE',  ( 0.000000000000000000, -9.500000000000008882, 5.000000000000004441 ) ) ;
#25684 = VERTEX_POINT ( 'NONE', #5095 ) ;
#25685 = EDGE_CURVE ( 'NONE', #2934, #17032, #2530, .T. ) ;
#25686 = CARTESIAN_POINT ( 'NONE',  ( -6.350852961085760029, -1.281975124255709124E-13, -58.12500000000004974 ) ) ;
#25687 = PRESENTATION_STYLE_ASSIGNMENT (( #9872 ) ) ;
#25688 = EDGE_CURVE ( 'NONE', #10874, #2429, #1405, .T. ) ;
#25689 = CARTESIAN_POINT ( 'NONE',  ( -3.464101615137757051, -5.999999999999979572, -152.0863248654051461 ) ) ;
#25690 = ORIENTED_EDGE ( 'NONE', *, *, #13761, .F. ) ;
#25691 = CARTESIAN_POINT ( 'NONE',  ( 105.0624999999998437, 2.500000000000055067, 1.035533905932869425 ) ) ;
#25692 = CARTESIAN_POINT ( 'NONE',  ( 141.6562500000000284, -6.000000000000005329, 2.485281374238556218 ) ) ;
#25693 = CARTESIAN_POINT ( 'NONE',  ( 5.412658773652739619, 3.124999999999988898, -100.3169872981078470 ) ) ;
#25694 = CARTESIAN_POINT ( 'NONE',  ( -5.999999999999963585, 9.296355089585909904E-15, -164.3363248654052313 ) ) ;
#25695 = CARTESIAN_POINT ( 'NONE',  ( 134.1562500000000568, -6.000000000000005329, 2.485281374238555774 ) ) ;
#25696 = FACE_OUTER_BOUND ( 'NONE', #9952, .T. ) ;
#25697 = AXIS2_PLACEMENT_3D ( 'NONE', #3220, #12645, #28875 ) ;
#25698 = CARTESIAN_POINT ( 'NONE',  ( -2.775557561562891351E-14, -5.500000000000115463, -135.7500000000000284 ) ) ;
#25699 = ORIENTED_EDGE ( 'NONE', *, *, #29732, .F. ) ;
#25700 = VERTEX_POINT ( 'NONE', #20165 ) ;
#25701 = CARTESIAN_POINT ( 'NONE',  ( -4.763139720814407951, 2.749999999999946709, -68.75000000000002842 ) ) ;
#25702 = CARTESIAN_POINT ( 'NONE',  ( 10.00000000000015277, 0.08046688801464986496, -2.448371654002133635 ) ) ;
#25703 = CARTESIAN_POINT ( 'NONE',  ( 160.0000000000000284, -12.64911064067353408, -3.000000000000002665 ) ) ;
#25704 = CARTESIAN_POINT ( 'NONE',  ( 3.608439182435180470, 6.249999999999982236, -90.55801270189225249 ) ) ;
#25705 = CARTESIAN_POINT ( 'NONE',  ( 10.50000000000003730, -1.999999999999835243, 0.000000000000000000 ) ) ;
#25706 = CARTESIAN_POINT ( 'NONE',  ( 154.8824251345948255, 5.500000000000012434, 2.278174593052012309 ) ) ;
#25707 = CARTESIAN_POINT ( 'NONE',  ( 113.2261751345946550, 2.000000000000031530, -0.8284271247459350507 ) ) ;
#25708 = CARTESIAN_POINT ( 'NONE',  ( 0.000000000000000000, 9.000000000000007105, -5.000000000000004441 ) ) ;
#25709 = CARTESIAN_POINT ( 'NONE',  ( 119.6252832217623165, 0.000000000000000000, 1.849990392679523588 ) ) ;
#25710 =( BOUNDED_CURVE ( )  B_SPLINE_CURVE ( 2, ( #13478, #25566, #16098, #22668, #13632, #4365, #25241, #13790, #30175 ),
 .UNSPECIFIED., .F., .T. ) 
 B_SPLINE_CURVE_WITH_KNOTS ( ( 3, 2, 2, 2, 3 ),
 ( 0.2058823529411764608, 0.2132352941176470507, 0.2205882352941176405, 0.2279411764705882304, 0.2352941176470588203 ),
 .UNSPECIFIED. ) 
 CURVE ( )  GEOMETRIC_REPRESENTATION_ITEM ( )  RATIONAL_B_SPLINE_CURVE ( ( 1.000000000000000000, 0.9238795325112867385, 1.000000000000000000, 0.9238795325112867385, 1.000000000000000000, 0.9238795325112867385, 1.000000000000000000, 0.9238795325112867385, 1.000000000000000000 ) ) 
 REPRESENTATION_ITEM ( '' )  );
#25711 = CARTESIAN_POINT ( 'NONE',  ( 3.175426480543072749, 5.499999999999865885, -148.6250000000000284 ) ) ;
#25712 = DIRECTION ( 'NONE',  ( -7.147005652999508048E-36, 5.642372883946980038E-36, 1.000000000000000000 ) ) ;
#25713 = CARTESIAN_POINT ( 'NONE',  ( 0.000000000000000000, 5.499999999999991118, -138.0000000000000000 ) ) ;
#25714 = CARTESIAN_POINT ( 'NONE',  ( 5.412658773652739619, 3.124999999999988898, -158.1830127018922667 ) ) ;
#25715 =( NAMED_UNIT ( * ) SI_UNIT ( $, .STERADIAN. ) SOLID_ANGLE_UNIT ( ) );
#25716 = CARTESIAN_POINT ( 'NONE',  ( -6.000000000000000888, 1.067854986875958443E-15, 7.560779664488942560E-35 ) ) ;
#25718 = CARTESIAN_POINT ( 'NONE',  ( 4.763139720814407951, -2.749999999999988454, -75.50000000000001421 ) ) ;
#25717 = AXIS2_PLACEMENT_3D ( 'NONE', #5790, #26681, #1922 ) ;
#25719 = CARTESIAN_POINT ( 'NONE',  ( 154.5863248654052313, 0.000000000000000000, 5.500000000000005329 ) ) ;
#25720 = CARTESIAN_POINT ( 'NONE',  ( 12.96132486540529882, 1.110223024625156540E-13, 2.500000000000002220 ) ) ;
#25721 = CARTESIAN_POINT ( 'NONE',  ( -3.175426480542816510, 5.499999999999865885, -68.87500000000002842 ) ) ;
#25722 = EDGE_CURVE ( 'NONE', #14585, #11534, #2699, .T. ) ;
#25723 =( BOUNDED_CURVE ( )  B_SPLINE_CURVE ( 2, ( #28686, #14479, #2751, #21362, #12026, #3050, #16781, #19513, #10143, #7801, #26546, #16635, #5348, #14333, #9835, #23671, #28543, #12178, #303, #28395, #26250, #7374, #12323, #5201, #602, #9988, #26105, #23813, #21522, #445, #7512, #19365, #18866, #244, #14275, #7316, #9021, #26050, #9326, #4847, #28040, #16578, #1951, #2110, #7011, #11670, #14134, #30358, #21305, #4396, #20854, #30208, #18717, #16428, #9628, #6710, #13665, #13822, #23166, #25752, #16127, #25897, #28187, #19021, #21161, #4700, #11514, #25433, #16726, #23616, #2550, #11977, #23007, #11355, #23320, #20701, #30051, #2410, #18411, #7163, #23472, #18563, #99, #4556, #9168, #11822, #27731, #9483, #2264, #27887, #6858, #16284, #21012, #25603, #13980, #22050, #16870, #19598, #7900, #542, #3285, #14561, #21906, #24045, #700, #21611, #14848, #4993, #12413, #2845, #17012, #7459, #2694, #3137, #24193, #5142, #985, #9933, #12120, #28938, #10239, #21460, #10385, #21757, #19738, #17314, #28785, #10084, #17460, #29085, #23904, #19457, #26630, #23763, #12266, #12559, #5588, #14426, #839, #2992, #19307, #14992, #28627, #7599, #24331, #7749, #26341, #390, #12711, #5289, #8047, #14698, #9781, #19159, #28494, #26191, #17159, #26479, #5438, #8679, #24942, #11153, #22202, #8837, #22518, #18076, #10859, #6355, #3746, #11009, #29394, #29234, #4050, #27093, #29561, #8518, #5892, #29707, #17926, #1135, #13472, #19890, #26775, #26931, #15318, #27242, #8198, #15789, #22663, #10536, #1605, #24482, #27389, #25093, #6061, #6213, #22813, #13181, #24642, #8363, #20354, #17773, #1290, #17613, #15474, #15150, #12863, #10704, #3893, #24798, #3587, #15631, #13018, #20212, #1449, #1756, #29858, #20504, #13324, #5742, #22354, #3432, #20048, #2227, #25397, #4207, #11316, #27691, #4664, #6516, #6672, #11629, #16243, #18678, #4518, #25867, #8985, #4358, #13783, #13940, #20973, #2513, #7122, #27540, #28001, #15939, #14097, #30322, #59, #23432, #4816, #25711, #9283, #18376, #20664, #23577, #28153, #9445, #18827, #11943, #14242, #23127, #30168, #2075, #30015, #27849, #25234, #13624, #11479, #2376, #9132, #16091, #6971, #22972, #16389, #6818, #21121, #21268, #16545, #25557, #11780, #208, #18223, #1909, #20820, #18524, #23286, #2659, #19123, #26454, #28596, #5260, #17128, #16981, #5405, #28901, #3247, #19424, #5556, #12677, #17280, #26602, #26156, #7285, #3103, #14819, #12082, #810, #14960, #21422, #353, #16688, #24161, #5107, #2809, #9747, #23726, #10201, #28454, #24299, #19567, #12529, #9594, #28751, #7564, #23867, #18984, #26010, #21870, #10046, #12234, #21574, #7866, #22014, #14528, #7425, #16834, #504, #14667, #28307, #4957, #24014, #14390, #9899, #19275, #7720, #26305, #2959, #12376, #21724, #664, #5859, #8324, #3860, #5707, #18045, #15753, #20325, #10349, #1416, #19710, #3403, #29674, #27211, #15116, #6184, #29055, #1571, #8641, #10665, #3709, #27359, #17733, #19856, #12985, #15597, #26895, #22320, #15277, #24449, #20010, #10824, #26740, #29361, #24604, #24767, #27058, #25061, #20175, #4018, #8485, #12826, #6023, #24912, #15441, #13293, #22632, #10979, #29527, #13142, #8164, #6325, #13435, #948, #8022, #17580, #17893, #17426, #22480, #29202, #1255, #22170, #1105, #10502, #3555, #22937, #9823, #8958, #20469, #16768, #27965, #8804, #19200, #9100, #28529, #5034, #16211, #30138, #5189, #7498, #1877, #6789, #7362, #11121, #11282, #20940, #26094, #22782, #11598, #20791, #6642, #14467, #18349, #20635, #30290, #25522, #29980, #1726, #23800, #27662, #2734, #13750, #26236, #2192, #9251, #435, #27817, #29828, #16063, #12162, #18646, #16910, #18193, #27508, #18497, #21509, #4485, #6487, #13909, #15912, #25363, #25208, #4174, #23096, #23254, #13595, #4332, #2040, #11447, #19936, #24528, #882, #3039, #26533, #19782, #10131, #5484, #19500, #7648, #24231, #2891, #589, #28830, #22098, #14890, #17057, #15039, #9976, #28982, #3182, #17504, #3477, #12604, #3330, #5334, #1175, #26388, #29130, #26819, #7791, #12909, #8241, #22246, #8090, #747, #24386, #14601, #21947, #12456, #10280, #24089, #10583, #17653, #29282, #26977, #23953, #19353, #5782, #21799, #19643, #17206, #12311, #7949, #21654, #26673, #5634, #12757, #1032, #10432, #6105, #20389, #24840, #1956, #6558, #11361, #20706, #18265, #11200, #15976, #29601, #27576, #22557, #3788, #4094, #8722, #1488, #5942, #25276, #10899, #4247, #27279, #1645, #15364, #13669, #23011, #22705, #20253, #20546, #30055, #9025, #24688, #1337, #3630, #11043, #13067, #29746, #22398, #13360, #29899, #8561, #8409, #6396, #18110, #10749, #27136, #17966, #6253, #15830, #25129, #20093, #29437, #17816, #15671, #24980, #13516, #22854, #1794, #8877, #11518, #23621, #25437, #27891, #20859, #27735, #9634, #2269, #19027, #18721, #396, #7167, #16583, #4998, #2414, #9786, #21015, #28345, #25902, #14430, #4853, #4402, #30363, #16730, #11828, #26054, #4704, #11980, #7016, #30211, #12124, #16433, #106, #9487, #16287, #251, #18870, #2114, #21468, #13826, #23172, #9173, #28193, #14279, #18568, #4561, #2554, #13984, #21309, #23324, #25757, #14138, #23477, #21165, #15155, #5442, #7604, #705, #24336, #14706, #10091, #24050, #12272, #3290, #28943, #14564, #7753, #2996, #12565, #17164, #3436, #7905, #12867, #26635, #2853, #24196, #14996, #14853, #12716, #10392, #22055, #17319, #3142, #12417, #17464, #22207, #26779, #990, #5293, #5593, #19164, #26486, #17017, #19461, #21616, #16875, #19743, #29089, #19313, #24487, #21761, #26195, #8050, #28791, #5147, #1142, #21910, #28498, #7463, #843, #10245, #23909, #548, #28633, #19602, #9937, #26345, #20052, #8683, #13477, #10541, #29711, #8522, #3751, #22816, #27097, #29399, #18080, #13327, #17778, #17929, #24804, #19897, #17618, #4053, #11011, #13186, #22521, #1760, #29862, #6066, #8368, #15477, #13629, #20357, #27392, #18226, #15634, #22976, #1454, #11158, #6359, #27543, #15792, #29239, #10862, #25097, #29564, #27246, #20507, #8202, #6218, #24944, #6519, #3897, #22666, #1609, #8841, #15942, #25240, #15326, #4212, #26939, #5897, #24646, #3593, #13023, #22360, #1294, #10709, #7128, #9599, #9451, #2519, #213, #11635, #4668, #28312, #18683, #20825, #13946, #16551, #27854, #23291, #6824, #25402, #20981, #30021, #18380, #16249, #18832, #2233, #4364, #27696, #16395, #30328, #14246, #4964, #21272, #9289, #21127, #23134, #18988, #13789, #25872, #23582, #25565, #7290, #26015, #16693, #11949, #18531, #11787, #28007, #28159, #14395, #1915, #65, #11323, #8991, #6678, #16096, #2078, #11483, #30174, #9139, #6979, #4524, #25718, #14102, #23438, #2381, #17132, #9904, #16987, #16840, #7430, #24304, #12239, #19715, #3253, #29059, #8025, #5561, #28906, #26159, #28756, #19572, #10054, #7871, #14964, #26607, #12533, #12683, #19280, #22018, #17430, #952, #17285, #28602, #3108, #23731, #668, #21578, #5264, #5111, #21427, #21875, #813, #23872, #10354, #7571, #357, #14531, #14673, #9751, #26745, #19429, #5711, #2664, #26458, #7725, #12087, #19127, #2816, #5410, #28459, #509, #26310, #10206, #24017, #2963, #12382, #21729, #14823, #24166, #1260, #24609, #13295, #17897, #22325, #15121, #27364, #20016, #6329, #6028, #18196, #24917, #3866, #22787, #20181, #27513, #29365, #1729, #15758, #29833, #10506, #24452, #10829, #25065, #29534, #4022, #22487, #29677, #17738, #17584, #11125, #15446, #27214, #6188, #3559, #18050, #15603, #22636, #20473, #8168, #3407, #15282, #12990, #1576, #26901, #13441, #10983, #29206, #20328, #12830, #8810, #22174, #24773, #8646, #1108, #1421, #10670, #19860, #3716, #5863, #8329, #27063, #13147, #8490, #16364, #1881, #25527, #2047, #30295, #4491, #21242, #25686, #184, #14070, #23259, #25370, #18502, #16216, #9415, #18959, #4637, #25215, #21099, #23405, #11287, #13914, #11452, #9257, #2198, #9566, #2351, #6491, #11752, #20640, #11602, #27, #20944, #27668, #23553, #18352, #18802, #28128, #20796, #4788, #15917, #14212, #7097, #23101, #16515, #4180, #18652, #4335, #27823, #8963, #13598, #25841, #2490, #22942, #11913, #29987, #6648, #16067, #6793, #13755, #30144, #27971, #9106, #6946, #21697, #5229, #10320, #24271, #28425, #12348, #12502, #16663, #7403, #3219, #12644, #10172, #3078, #7838, #21548, #19541, #14504, #16811, #26426, #634, #5077, #28276, #28874, #2780, #17250, #19246, #921, #7690, #17098, #26575, #14642, #12208, #21841, #14933, #5528, #21988, #23701 ),
 .UNSPECIFIED., .F., .T. ) 
 B_SPLINE_CURVE_WITH_KNOTS ( ( 3, 2, 2, 2, 2, 2, 2, 2, 2, 2, 2, 2, 2, 2, 2, 2, 2, 2, 2, 2, 2, 2, 2, 2, 2, 2, 2, 2, 2, 2, 2, 2, 2, 2, 2, 2, 2, 2, 2, 2, 2, 2, 2, 2, 2, 2, 2, 2, 2, 2, 2, 2, 2, 2, 2, 2, 2, 2, 2, 2, 2, 2, 2, 2, 2, 2, 2, 2, 2, 2, 2, 2, 2, 2, 2, 2, 2, 2, 2, 2, 2, 2, 2, 2, 2, 2, 2, 2, 2, 2, 2, 2, 2, 2, 2, 2, 2, 2, 2, 2, 2, 2, 2, 2, 2, 2, 2, 2, 2, 2, 2, 2, 2, 2, 2, 2, 2, 2, 2, 2, 2, 2, 2, 2, 2, 2, 2, 2, 2, 2, 2, 2, 2, 2, 2, 2, 2, 2, 2, 2, 2, 2, 2, 2, 2, 2, 2, 2, 2, 2, 2, 2, 2, 2, 2, 2, 2, 2, 2, 2, 2, 2, 2, 2, 2, 2, 2, 2, 2, 2, 2, 2, 2, 2, 2, 2, 2, 2, 2, 2, 2, 2, 2, 2, 2, 2, 2, 2, 2, 2, 2, 2, 2, 2, 2, 2, 2, 2, 2, 2, 2, 2, 2, 2, 2, 2, 2, 2, 2, 2, 2, 2, 2, 2, 2, 2, 2, 2, 2, 2, 2, 2, 2, 2, 2, 2, 2, 2, 2, 2, 2, 2, 2, 2, 2, 2, 2, 2, 2, 2, 2, 2, 2, 2, 2, 2, 2, 2, 2, 2, 2, 2, 2, 2, 2, 2, 2, 2, 2, 2, 2, 2, 2, 2, 2, 2, 2, 2, 2, 2, 2, 2, 2, 2, 2, 2, 2, 2, 2, 2, 2, 2, 2, 2, 2, 2, 2, 2, 2, 2, 2, 2, 2, 2, 2, 2, 2, 2, 2, 2, 2, 2, 2, 2, 2, 2, 2, 2, 2, 2, 2, 2, 2, 2, 2, 2, 2, 2, 2, 2, 2, 2, 2, 2, 2, 2, 2, 2, 2, 2, 2, 2, 2, 2, 2, 2, 2, 2, 2, 2, 2, 2, 2, 2, 2, 2, 2, 2, 2, 2, 2, 2, 2, 2, 2, 2, 2, 2, 2, 2, 2, 2, 2, 2, 2, 2, 2, 2, 2, 2, 2, 2, 2, 2, 2, 2, 2, 2, 2, 2, 2, 2, 2, 2, 2, 2, 2, 2, 2, 2, 2, 2, 2, 2, 2, 2, 2, 2, 2, 2, 2, 2, 2, 2, 2, 2, 2, 2, 2, 2, 2, 2, 2, 2, 2, 2, 2, 2, 2, 2, 2, 2, 2, 2, 2, 2, 2, 2, 2, 2, 2, 2, 2, 2, 2, 2, 2, 2, 2, 2, 2, 2, 2, 2, 2, 2, 2, 2, 2, 2, 2, 2, 2, 2, 2, 2, 2, 2, 2, 2, 2, 2, 2, 2, 2, 2, 2, 2, 2, 2, 2, 2, 2, 2, 2, 2, 2, 2, 2, 2, 2, 2, 2, 2, 2, 2, 2, 2, 2, 2, 2, 2, 2, 2, 2, 2, 2, 2, 2, 2, 2, 2, 2, 2, 2, 2, 2, 2, 2, 2, 2, 2, 2, 2, 2, 2, 2, 2, 2, 2, 2, 2, 2, 2, 2, 2, 2, 2, 2, 2, 2, 2, 2, 2, 3 ),
 ( 0.01111111111111070908, 0.01296296296296256013, 0.01481481481481441466, 0.01666666666666626745, 0.01851851851851811850, 0.02037037037036997303, 0.02222222222222182408, 0.02407407407407367861, 0.02592592592592552619, 0.02777777777777737378, 0.02962962962962923524, 0.03148148148148108283, 0.03333333333333293735, 0.03518518518518479188, 0.03703703703703663946, 0.03888888888888849399, 0.04074074074074034851, 0.04259259259259220304, 0.04444444444444405062, 0.04629629629629590515, 0.04814814814814775967, 0.04999999999999961420, 0.05185185185185146178, 0.05370370370370331631, 0.05555555555555517083, 0.05740740740740701842, 0.05925925925925887988, 0.06111111111111072053, 0.06296296296296256811, 0.06481481481481442264, 0.06666666666666627716, 0.06851851851851813169, 0.07037037037036998621, 0.07222222222222182686, 0.07407407407407369526, 0.07592592592592554979, 0.07777777777777739043, 0.07962962962962924496, 0.08148148148148111336, 0.08333333333333295401, 0.08518518518518480853, 0.08703703703703666306, 0.08888888888888851758, 0.09074074074074037211, 0.09259259259259221275, 0.09444444444444406728, 0.09629629629629592180, 0.09814814814814777633, 0.09999999999999964473, 0.1018518518518514715, 0.1037037037037033260, 0.1055555555555551805, 0.1074074074074070489, 0.1092592592592588896, 0.1111111111111107302, 0.1129629629629625986, 0.1148148148148144532, 0.1166666666666662938, 0.1185185185185181483, 0.1203703703703700029, 0.1222222222222218574, 0.1240740740740737119, 0.1259259259259255248, 0.1277777777777774071, 0.1296296296296292616, 0.1314814814814811161, 0.1333333333333329707, 0.1351851851851848252, 0.1370370370370367075, 0.1388888888888885620, 0.1407407407407404165, 0.1425925925925922710, 0.1444444444444440701, 0.1462962962962959246, 0.1481481481481477791, 0.1499999999999996614, 0.1518518518518515159, 0.1537037037037033704, 0.1555555555555552250, 0.1574074074074070795, 0.1592592592592589340, 0.1611111111111107608, 0.1629629629629626431, 0.1648148148148144698, 0.1666666666666663243, 0.1685185185185181789, 0.1703703703703700334, 0.1722222222222218879, 0.1740740740740737424, 0.1759259259259255970, 0.1777777777777774515, 0.1796296296296293060, 0.1814814814814811605, 0.1833333333333329873, 0.1851851851851848418, 0.1870370370370366964, 0.1888888888888885786, 0.1907407407407404054, 0.1925925925925922599, 0.1944444444444441145, 0.1962962962962959690, 0.1981481481481478235, 0.1999999999999996780, 0.2018518518518515603, 0.2037037037037033871, 0.2055555555555552416, 0.2074074074074070684, 0.2092592592592589229, 0.2111111111111107774, 0.2129629629629626320, 0.2148148148148145142, 0.2166666666666663688, 0.2185185185185182233, 0.2203703703703700778, 0.2222222222222218768, 0.2240740740740737313, 0.2259259259259255859, 0.2277777777777774404, 0.2296296296296293227, 0.2314814814814811772, 0.2333333333333330317, 0.2351851851851848862, 0.2370370370370367408, 0.2388888888888885675, 0.2407407407407403943, 0.2425925925925922766, 0.2444444444444441311, 0.2462962962962959856, 0.2481481481481478402, 0.2499999999999996947, 0.2518518518518514937, 0.2537037037037033760, 0.2555555555555552028, 0.2574074074074070850, 0.2592592592592589118, 0.2611111111111107941, 0.2629629629629626208, 0.2648148148148144476, 0.2666666666666663299, 0.2685185185185181567, 0.2703703703703700389, 0.2722222222222218102, 0.2740740740740737480, 0.2759259259259255748, 0.2777777777777774015, 0.2796296296296292838, 0.2814814814814811106, 0.2833333333333329929, 0.2851851851851848196, 0.2870370370370367019, 0.2888888888888885287, 0.2907407407407404110, 0.2925925925925922377, 0.2944444444444440645, 0.2962962962962959468, 0.2981481481481477736, 0.2999999999999996558, 0.3018518518518515381, 0.3037037037037033649, 0.3055555555555552472, 0.3074074074074070739, 0.3092592592592589007, 0.3111111111111107275, 0.3129629629629626097, 0.3148148148148144920, 0.3166666666666663188, 0.3185185185185182011, 0.3203703703703700278, 0.3222222222222219101, 0.3240740740740736814, 0.3259259259259256192, 0.3277777777777774459, 0.3296296296296292727, 0.3314814814814811550, 0.3333333333333329818, 0.3351851851851848640, 0.3370370370370366908, 0.3388888888888885731, 0.3407407407407403999, 0.3425925925925922821, 0.3444444444444441089, 0.3462962962962959357, 0.3481481481481478180, 0.3499999999999996447, 0.3518518518518515270, 0.3537037037037034093, 0.3555555555555552361, 0.3574074074074070628, 0.3592592592592589451, 0.3611111111111107719, 0.3629629629629626542, 0.3648148148148144809, 0.3666666666666663632, 0.3685185185185181900, 0.3703703703703700723, 0.3722222222222218990, 0.3740740740740737258, 0.3759259259259256081, 0.3777777777777774348, 0.3796296296296293726, 0.3814814814814811439, 0.3833333333333330817, 0.3851851851851848529, 0.3870370370370366797, 0.3888888888888885620, 0.3907407407407403888, 0.3925925925925923266, 0.3944444444444440978, 0.3962962962962960356, 0.3981481481481478069, 0.3999999999999997446, 0.4018518518518515159, 0.4037037037037033982, 0.4055555555555552805, 0.4074074074074070517, 0.4092592592592589895, 0.4111111111111107608, 0.4129629629629626986, 0.4148148148148144698, 0.4166666666666664076, 0.4185185185185182344, 0.4203703703703700612, 0.4222222222222219434, 0.4240740740740737147, 0.4259259259259256525, 0.4277777777777774237, 0.4296296296296293615, 0.4314814814814811328, 0.4333333333333330151, 0.4351851851851848973, 0.4370370370370367241, 0.4388888888888886064, 0.4407407407407404332, 0.4425925925925923154, 0.4444444444444440867, 0.4462962962962960245, 0.4481481481481478513, 0.4499999999999996780, 0.4518518518518515603, 0.4537037037037033871, 0.4555555555555552694, 0.4574074074074070961, 0.4592592592592589784, 0.4611111111111108607, 0.4629629629629626875, 0.4648148148148145142, 0.4666666666666663410, 0.4685185185185182233, 0.4703703703703700501, 0.4722222222222219323, 0.4740740740740738146, 0.4759259259259256414, 0.4777777777777775237, 0.4796296296296293504, 0.4814814814814811772, 0.4833333333333330040, 0.4851851851851848862, 0.4870370370370367685, 0.4888888888888885953, 0.4907407407407404776, 0.4925925925925923043, 0.4944444444444441866, 0.4962962962962959579, 0.4981481481481478957, 0.4999999999999997224, 0.5018518518518516602, 0.5037037037037034315, 0.5055555555555553138, 0.5074074074074071961, 0.5092592592592590783, 0.5111111111111108496, 0.5129629629629627319, 0.5148148148148147252, 0.5166666666666664964, 0.5185185185185182677, 0.5203703703703702610, 0.5222222222222221433, 0.5240740740740739145, 0.5259259259259256858, 0.5277777777777775681, 0.5296296296296295614, 0.5314814814814813326, 0.5333333333333331039, 0.5351851851851849862, 0.5370370370370369795, 0.5388888888888887507, 0.5407407407407406330, 0.5425925925925924043, 0.5444444444444441755, 0.5462962962962961688, 0.5481481481481480511, 0.5499999999999999334, 0.5518518518518515936, 0.5537037037037035869, 0.5555555555555554692, 0.5574074074074073515, 0.5592592592592590117, 0.5611111111111108940, 0.5629629629629628873, 0.5648148148148146586, 0.5666666666666665408, 0.5685185185185183121, 0.5703703703703703054, 0.5722222222222220767, 0.5740740740740739589, 0.5759259259259258412, 0.5777777777777775015, 0.5796296296296294948, 0.5814814814814813770, 0.5833333333333332593, 0.5851851851851849196, 0.5870370370370369129, 0.5888888888888887951, 0.5907407407407406774, 0.5925925925925924487, 0.5944444444444442199, 0.5962962962962962132, 0.5981481481481479845, 0.5999999999999998668, 0.6018518518518516380, 0.6037037037037036313, 0.6055555555555554026, 0.6074074074074072849, 0.6092592592592591672, 0.6111111111111109384, 0.6129629629629628207, 0.6148148148148147030, 0.6166666666666665853, 0.6185185185185183565, 0.6203703703703701278, 0.6222222222222221211, 0.6240740740740740033, 0.6259259259259257746, 0.6277777777777775459, 0.6296296296296295392, 0.6314814814814814214, 0.6333333333333331927, 0.6351851851851850750, 0.6370370370370368462, 0.6388888888888887285, 0.6407407407407406108, 0.6425925925925924931, 0.6444444444444443754, 0.6462962962962961466, 0.6481481481481480289, 0.6499999999999999112, 0.6518518518518517935, 0.6537037037037034537, 0.6555555555555554470, 0.6574074074074073293, 0.6592592592592591005, 0.6611111111111109828, 0.6629629629629628651, 0.6648148148148147474, 0.6666666666666665186, 0.6685185185185184009, 0.6703703703703702832, 0.6722222222222221655, 0.6740740740740739367, 0.6759259259259258190, 0.6777777777777777013, 0.6796296296296294726, 0.6814814814814813548, 0.6833333333333332371, 0.6851851851851851194, 0.6870370370370368907, 0.6888888888888887729, 0.6907407407407406552, 0.6925925925925924265, 0.6944444444444443088, 0.6962962962962963021, 0.6981481481481480733, 0.6999999999999998446, 0.7018518518518517268, 0.7037037037037036091, 0.7055555555555554914, 0.7074074074074072627, 0.7092592592592591449, 0.7111111111111110272, 0.7129629629629629095, 0.7148148148148146808, 0.7166666666666665630, 0.7185185185185184453, 0.7203703703703702166, 0.7222222222222222099, 0.7240740740740739811, 0.7259259259259258634, 0.7277777777777776347, 0.7296296296296295170, 0.7314814814814813992, 0.7333333333333331705, 0.7351851851851850528, 0.7370370370370369351, 0.7388888888888889284, 0.7407407407407405886, 0.7425925925925924709, 0.7444444444444443532, 0.7462962962962962354, 0.7481481481481481177, 0.7499999999999998890, 0.7518518518518517713, 0.7537037037037035425, 0.7555555555555555358, 0.7574074074074073071, 0.7592592592592591894, 0.7611111111111109606, 0.7629629629629628429, 0.7648148148148148362, 0.7666666666666666075, 0.7685185185185183787, 0.7703703703703702610, 0.7722222222222222543, 0.7740740740740740256, 0.7759259259259257968, 0.7777777777777776791, 0.7796296296296295614, 0.7814814814814814437, 0.7833333333333332149, 0.7851851851851850972, 0.7870370370370369795, 0.7888888888888888618, 0.7907407407407407440, 0.7925925925925925153, 0.7944444444444442865, 0.7962962962962961688, 0.7981481481481481621, 0.8000000000000000444, 0.8018518518518517046, 0.8037037037037035869, 0.8055555555555555802, 0.8074074074074074625, 0.8092592592592591227, 0.8111111111111110050, 0.8129629629629628873, 0.8148148148148147696, 0.8166666666666666519, 0.8185185185185184231, 0.8203703703703703054, 0.8222222222222221877, 0.8240740740740740700, 0.8259259259259259522, 0.8277777777777776125, 0.8296296296296294948, 0.8314814814814814881, 0.8333333333333333703, 0.8351851851851850306, 0.8370370370370369129, 0.8388888888888887951, 0.8407407407407407884, 0.8425925925925925597, 0.8444444444444443310, 0.8462962962962962132, 0.8481481481481480955, 0.8499999999999999778, 0.8518518518518518601, 0.8537037037037036313, 0.8555555555555554026, 0.8574074074074073959, 0.8592592592592592782, 0.8611111111111110494, 0.8629629629629628207, 0.8648148148148148140, 0.8666666666666666963, 0.8685185185185184675, 0.8703703703703702388, 0.8722222222222221211, 0.8740740740740741144, 0.8759259259259258856, 0.8777777777777776569, 0.8796296296296295392, 0.8814814814814815325, 0.8833333333333333037, 0.8851851851851851860, 0.8870370370370369573, 0.8888888888888887285, 0.8907407407407407218, 0.8925925925925926041, 0.8944444444444444864, 0.8962962962962961466, 0.8981481481481481399, 0.9000000000000000222, 0.9018518518518519045, 0.9037037037037035647, 0.9055555555555554470, 0.9074074074074074403, 0.9092592592592592116, 0.9111111111111110938, 0.9129629629629628651, 0.9148148148148148584, 0.9166666666666666297, 0.9185185185185185119, 0.9203703703703703942, 0.9222222222222221655, 0.9240740740740740478, 0.9259259259259259300, 0.9277777777777778123, 0.9296296296296294726, 0.9314814814814814659, 0.9333333333333333481, 0.9351851851851852304, 0.9370370370370370017, 0.9388888888888887729, 0.9407407407407407662, 0.9425925925925925375, 0.9444444444444444198, 0.9462962962962963021, 0.9481481481481480733, 0.9499999999999999556, 0.9518518518518518379, 0.9537037037037037202, 0.9555555555555554914, 0.9574074074074073737, 0.9592592592592592560, 0.9611111111111111382, 0.9629629629629629095, 0.9648148148148146808, 0.9666666666666666741, 0.9685185185185185563, 0.9703703703703703276, 0.9722222222222222099, 0.9740740740740740922, 0.9759259259259259744, 0.9777777777777777457, 0.9796296296296296280, 0.9814814814814813992, 0.9833333333333332815, 0.9851851851851851638, 0.9870370370370370461, 0.9888888888888889284, 0.9907407407407406996, 0.9925925925925925819, 0.9944444444444444642, 0.9962962962962963465, 0.9981481481481481177, 1.000000000000000000 ),
 .UNSPECIFIED. ) 
 CURVE ( )  GEOMETRIC_REPRESENTATION_ITEM ( )  RATIONAL_B_SPLINE_CURVE ( ( 1.000000000000029088, 0.8660254037844096198, 1.000000000000000000, 0.8660254037844387076, 1.000000000000000000, 0.8660254037844387076, 1.000000000000000000, 0.8660254037844387076, 1.000000000000000000, 0.8660254037844387076, 1.000000000000000000, 0.8660254037844387076, 1.000000000000000000, 0.8660254037844387076, 1.000000000000000000, 0.8660254037844387076, 1.000000000000000000, 0.8660254037844387076, 1.000000000000000000, 0.8660254037844387076, 1.000000000000000000, 0.8660254037844387076, 1.000000000000000000, 0.8660254037844387076, 1.000000000000000000, 0.8660254037844387076, 1.000000000000000000, 0.8660254037844387076, 1.000000000000000000, 0.8660254037844387076, 1.000000000000000000, 0.8660254037844387076, 1.000000000000000000, 0.8660254037844387076, 1.000000000000000000, 0.8660254037844387076, 1.000000000000000000, 0.8660254037844387076, 1.000000000000000000, 0.8660254037844387076, 1.000000000000000000, 0.8660254037844387076, 1.000000000000000000, 0.8660254037844387076, 1.000000000000000000, 0.8660254037844387076, 1.000000000000000000, 0.8660254037844387076, 1.000000000000000000, 0.8660254037844387076, 1.000000000000000000, 0.8660254037844387076, 1.000000000000000000, 0.8660254037844387076, 1.000000000000000000, 0.8660254037844387076, 1.000000000000000000, 0.8660254037844387076, 1.000000000000000000, 0.8660254037844387076, 1.000000000000000000, 0.8660254037844387076, 1.000000000000000000, 0.8660254037844387076, 1.000000000000000000, 0.8660254037844387076, 1.000000000000000000, 0.8660254037844387076, 1.000000000000000000, 0.8660254037844387076, 1.000000000000000000, 0.8660254037844387076, 1.000000000000000000, 0.8660254037844387076, 1.000000000000000000, 0.8660254037844387076, 1.000000000000000000, 0.8660254037844387076, 1.000000000000000000, 0.8660254037844387076, 1.000000000000000000, 0.8660254037844387076, 1.000000000000000000, 0.8660254037844387076, 1.000000000000000000, 0.8660254037844387076, 1.000000000000000000, 0.8660254037844387076, 1.000000000000000000, 0.8660254037844387076, 1.000000000000000000, 0.8660254037844387076, 1.000000000000000000, 0.8660254037844387076, 1.000000000000000000, 0.8660254037844387076, 1.000000000000000000, 0.8660254037844387076, 1.000000000000000000, 0.8660254037844387076, 1.000000000000000000, 0.8660254037844387076, 1.000000000000000000, 0.8660254037844387076, 1.000000000000000000, 0.8660254037844387076, 1.000000000000000000, 0.8660254037844387076, 1.000000000000000000, 0.8660254037844387076, 1.000000000000000000, 0.8660254037844387076, 1.000000000000000000, 0.8660254037844387076, 1.000000000000000000, 0.8660254037844387076, 1.000000000000000000, 0.8660254037844387076, 1.000000000000000000, 0.8660254037844387076, 1.000000000000000000, 0.8660254037844387076, 1.000000000000000000, 0.8660254037844387076, 1.000000000000000000, 0.8660254037844387076, 1.000000000000000000, 0.8660254037844387076, 1.000000000000000000, 0.8660254037844387076, 1.000000000000000000, 0.8660254037844387076, 1.000000000000000000, 0.8660254037844387076, 1.000000000000000000, 0.8660254037844387076, 1.000000000000000000, 0.8660254037844387076, 1.000000000000000000, 0.8660254037844387076, 1.000000000000000000, 0.8660254037844387076, 1.000000000000000000, 0.8660254037844387076, 1.000000000000000000, 0.8660254037844387076, 1.000000000000000000, 0.8660254037844387076, 1.000000000000000000, 0.8660254037844387076, 1.000000000000000000, 0.8660254037844387076, 1.000000000000000000, 0.8660254037844387076, 1.000000000000000000, 0.8660254037844387076, 1.000000000000000000, 0.8660254037844387076, 1.000000000000000000, 0.8660254037844387076, 1.000000000000000000, 0.8660254037844387076, 1.000000000000000000, 0.8660254037844387076, 1.000000000000000000, 0.8660254037844387076, 1.000000000000000000, 0.8660254037844387076, 1.000000000000000000, 0.8660254037844387076, 1.000000000000000000, 0.8660254037844387076, 1.000000000000000000, 0.8660254037844387076, 1.000000000000000000, 0.8660254037844387076, 1.000000000000000000, 0.8660254037844387076, 1.000000000000000000, 0.8660254037844387076, 1.000000000000000000, 0.8660254037844387076, 1.000000000000000000, 0.8660254037844387076, 1.000000000000000000, 0.8660254037844387076, 1.000000000000000000, 0.8660254037844387076, 1.000000000000000000, 0.8660254037844387076, 1.000000000000000000, 0.8660254037844387076, 1.000000000000000000, 0.8660254037844387076, 1.000000000000000000, 0.8660254037844387076, 1.000000000000000000, 0.8660254037844387076, 1.000000000000000000, 0.8660254037844387076, 1.000000000000000000, 0.8660254037844387076, 1.000000000000000000, 0.8660254037844387076, 1.000000000000000000, 0.8660254037844387076, 1.000000000000000000, 0.8660254037844387076, 1.000000000000000000, 0.8660254037844387076, 1.000000000000000000, 0.8660254037844387076, 1.000000000000000000, 0.8660254037844387076, 1.000000000000000000, 0.8660254037844387076, 1.000000000000000000, 0.8660254037844387076, 1.000000000000000000, 0.8660254037844387076, 1.000000000000000000, 0.8660254037844387076, 1.000000000000000000, 0.8660254037844387076, 1.000000000000000000, 0.8660254037844387076, 1.000000000000000000, 0.8660254037844387076, 1.000000000000000000, 0.8660254037844387076, 1.000000000000000000, 0.8660254037844387076, 1.000000000000000000, 0.8660254037844387076, 1.000000000000000000, 0.8660254037844387076, 1.000000000000000000, 0.8660254037844387076, 1.000000000000000000, 0.8660254037844387076, 1.000000000000000000, 0.8660254037844387076, 1.000000000000000000, 0.8660254037844387076, 1.000000000000000000, 0.8660254037844387076, 1.000000000000000000, 0.8660254037844387076, 1.000000000000000000, 0.8660254037844387076, 1.000000000000000000, 0.8660254037844387076, 1.000000000000000000, 0.8660254037844387076, 1.000000000000000000, 0.8660254037844387076, 1.000000000000000000, 0.8660254037844387076, 1.000000000000000000, 0.8660254037844387076, 1.000000000000000000, 0.8660254037844387076, 1.000000000000000000, 0.8660254037844387076, 1.000000000000000000, 0.8660254037844387076, 1.000000000000000000, 0.8660254037844387076, 1.000000000000000000, 0.8660254037844387076, 1.000000000000000000, 0.8660254037844387076, 1.000000000000000000, 0.8660254037844387076, 1.000000000000000000, 0.8660254037844387076, 1.000000000000000000, 0.8660254037844387076, 1.000000000000000000, 0.8660254037844387076, 1.000000000000000000, 0.8660254037844387076, 1.000000000000000000, 0.8660254037844387076, 1.000000000000000000, 0.8660254037844387076, 1.000000000000000000, 0.8660254037844387076, 1.000000000000000000, 0.8660254037844387076, 1.000000000000000000, 0.8660254037844387076, 1.000000000000000000, 0.8660254037844387076, 1.000000000000000000, 0.8660254037844387076, 1.000000000000000000, 0.8660254037844387076, 1.000000000000000000, 0.8660254037844387076, 1.000000000000000000, 0.8660254037844387076, 1.000000000000000000, 0.8660254037844387076, 1.000000000000000000, 0.8660254037844387076, 1.000000000000000000, 0.8660254037844387076, 1.000000000000000000, 0.8660254037844387076, 1.000000000000000000, 0.8660254037844387076, 1.000000000000000000, 0.8660254037844387076, 1.000000000000000000, 0.8660254037844387076, 1.000000000000000000, 0.8660254037844387076, 1.000000000000000000, 0.8660254037844387076, 1.000000000000000000, 0.8660254037844387076, 1.000000000000000000, 0.8660254037844387076, 1.000000000000000000, 0.8660254037844387076, 1.000000000000000000, 0.8660254037844387076, 1.000000000000000000, 0.8660254037844387076, 1.000000000000000000, 0.8660254037844387076, 1.000000000000000000, 0.8660254037844387076, 1.000000000000000000, 0.8660254037844387076, 1.000000000000000000, 0.8660254037844387076, 1.000000000000000000, 0.8660254037844387076, 1.000000000000000000, 0.8660254037844387076, 1.000000000000000000, 0.8660254037844387076, 1.000000000000000000, 0.8660254037844387076, 1.000000000000000000, 0.8660254037844387076, 1.000000000000000000, 0.8660254037844387076, 1.000000000000000000, 0.8660254037844387076, 1.000000000000000000, 0.8660254037844387076, 1.000000000000000000, 0.8660254037844387076, 1.000000000000000000, 0.8660254037844387076, 1.000000000000000000, 0.8660254037844387076, 1.000000000000000000, 0.8660254037844387076, 1.000000000000000000, 0.8660254037844387076, 1.000000000000000000, 0.8660254037844387076, 1.000000000000000000, 0.8660254037844387076, 1.000000000000000000, 0.8660254037844387076, 1.000000000000000000, 0.8660254037844387076, 1.000000000000000000, 0.8660254037844387076, 1.000000000000000000, 0.8660254037844387076, 1.000000000000000000, 0.8660254037844387076, 1.000000000000000000, 0.8660254037844387076, 1.000000000000000000, 0.8660254037844387076, 1.000000000000000000, 0.8660254037844387076, 1.000000000000000000, 0.8660254037844387076, 1.000000000000000000, 0.8660254037844387076, 1.000000000000000000, 0.8660254037844387076, 1.000000000000000000, 0.8660254037844387076, 1.000000000000000000, 0.8660254037844387076, 1.000000000000000000, 0.8660254037844387076, 1.000000000000000000, 0.8660254037844387076, 1.000000000000000000, 0.8660254037844387076, 1.000000000000000000, 0.8660254037844387076, 1.000000000000000000, 0.8660254037844387076, 1.000000000000000000, 0.8660254037844387076, 1.000000000000000000, 0.8660254037844387076, 1.000000000000000000, 0.8660254037844387076, 1.000000000000000000, 0.8660254037844387076, 1.000000000000000000, 0.8660254037844387076, 1.000000000000000000, 0.8660254037844387076, 1.000000000000000000, 0.8660254037844387076, 1.000000000000000000, 0.8660254037844387076, 1.000000000000000000, 0.8660254037844387076, 1.000000000000000000, 0.8660254037844387076, 1.000000000000000000, 0.8660254037844387076, 1.000000000000000000, 0.8660254037844387076, 1.000000000000000000, 0.8660254037844387076, 1.000000000000000000, 0.8660254037844387076, 1.000000000000000000, 0.8660254037844387076, 1.000000000000000000, 0.8660254037844387076, 1.000000000000000000, 0.8660254037844387076, 1.000000000000000000, 0.8660254037844387076, 1.000000000000000000, 0.8660254037844387076, 1.000000000000000000, 0.8660254037844387076, 1.000000000000000000, 0.8660254037844387076, 1.000000000000000000, 0.8660254037844387076, 1.000000000000000000, 0.8660254037844387076, 1.000000000000000000, 0.8660254037844387076, 1.000000000000000000, 0.8660254037844387076, 1.000000000000000000, 0.8660254037844387076, 1.000000000000000000, 0.8660254037844387076, 1.000000000000000000, 0.8660254037844387076, 1.000000000000000000, 0.8660254037844387076, 1.000000000000000000, 0.8660254037844387076, 1.000000000000000000, 0.8660254037844387076, 1.000000000000000000, 0.8660254037844387076, 1.000000000000000000, 0.8660254037844387076, 1.000000000000000000, 0.8660254037844387076, 1.000000000000000000, 0.8660254037844387076, 1.000000000000000000, 0.8660254037844387076, 1.000000000000000000, 0.8660254037844387076, 1.000000000000000000, 0.8660254037844387076, 1.000000000000000000, 0.8660254037844387076, 1.000000000000000000, 0.8660254037844387076, 1.000000000000000000, 0.8660254037844387076, 1.000000000000000000, 0.8660254037844387076, 1.000000000000000000, 0.8660254037844387076, 1.000000000000000000, 0.8660254037844387076, 1.000000000000000000, 0.8660254037844387076, 1.000000000000000000, 0.8660254037844387076, 1.000000000000000000, 0.8660254037844387076, 1.000000000000000000, 0.8660254037844387076, 1.000000000000000000, 0.8660254037844387076, 1.000000000000000000, 0.8660254037844387076, 1.000000000000000000, 0.8660254037844387076, 1.000000000000000000, 0.8660254037844387076, 1.000000000000000000, 0.8660254037844387076, 1.000000000000000000, 0.8660254037844387076, 1.000000000000000000, 0.8660254037844387076, 1.000000000000000000, 0.8660254037844387076, 1.000000000000000000, 0.8660254037844387076, 1.000000000000000000, 0.8660254037844387076, 1.000000000000000000, 0.8660254037844387076, 1.000000000000000000, 0.8660254037844387076, 1.000000000000000000, 0.8660254037844387076, 1.000000000000000000, 0.8660254037844387076, 1.000000000000000000, 0.8660254037844387076, 1.000000000000000000, 0.8660254037844387076, 1.000000000000000000, 0.8660254037844387076, 1.000000000000000000, 0.8660254037844387076, 1.000000000000000000, 0.8660254037844387076, 1.000000000000000000, 0.8660254037844387076, 1.000000000000000000, 0.8660254037844387076, 1.000000000000000000, 0.8660254037844387076, 1.000000000000000000, 0.8660254037844387076, 1.000000000000000000, 0.8660254037844387076, 1.000000000000000000, 0.8660254037844387076, 1.000000000000000000, 0.8660254037844387076, 1.000000000000000000, 0.8660254037844387076, 1.000000000000000000, 0.8660254037844387076, 1.000000000000000000, 0.8660254037844387076, 1.000000000000000000, 0.8660254037844387076, 1.000000000000000000, 0.8660254037844387076, 1.000000000000000000, 0.8660254037844387076, 1.000000000000000000, 0.8660254037844387076, 1.000000000000000000, 0.8660254037844387076, 1.000000000000000000, 0.8660254037844387076, 1.000000000000000000, 0.8660254037844387076, 1.000000000000000000, 0.8660254037844387076, 1.000000000000000000, 0.8660254037844387076, 1.000000000000000000, 0.8660254037844387076, 1.000000000000000000, 0.8660254037844387076, 1.000000000000000000, 0.8660254037844387076, 1.000000000000000000, 0.8660254037844387076, 1.000000000000000000, 0.8660254037844387076, 1.000000000000000000, 0.8660254037844387076, 1.000000000000000000, 0.8660254037844387076, 1.000000000000000000, 0.8660254037844387076, 1.000000000000000000, 0.8660254037844387076, 1.000000000000000000, 0.8660254037844387076, 1.000000000000000000, 0.8660254037844387076, 1.000000000000000000, 0.8660254037844387076, 1.000000000000000000, 0.8660254037844387076, 1.000000000000000000, 0.8660254037844387076, 1.000000000000000000, 0.8660254037844387076, 1.000000000000000000, 0.8660254037844387076, 1.000000000000000000, 0.8660254037844387076, 1.000000000000000000, 0.8660254037844387076, 1.000000000000000000, 0.8660254037844387076, 1.000000000000000000, 0.8660254037844387076, 1.000000000000000000, 0.8660254037844387076, 1.000000000000000000, 0.8660254037844387076, 1.000000000000000000, 0.8660254037844387076, 1.000000000000000000, 0.8660254037844387076, 1.000000000000000000, 0.8660254037844387076, 1.000000000000000000, 0.8660254037844387076, 1.000000000000000000, 0.8660254037844387076, 1.000000000000000000, 0.8660254037844387076, 1.000000000000000000, 0.8660254037844387076, 1.000000000000000000, 0.8660254037844387076, 1.000000000000000000, 0.8660254037844387076, 1.000000000000000000, 0.8660254037844387076, 1.000000000000000000, 0.8660254037844387076, 1.000000000000000000, 0.8660254037844387076, 1.000000000000000000, 0.8660254037844387076, 1.000000000000000000, 0.8660254037844387076, 1.000000000000000000, 0.8660254037844387076, 1.000000000000000000, 0.8660254037844387076, 1.000000000000000000, 0.8660254037844387076, 1.000000000000000000, 0.8660254037844387076, 1.000000000000000000, 0.8660254037844387076, 1.000000000000000000, 0.8660254037844387076, 1.000000000000000000, 0.8660254037844387076, 1.000000000000000000, 0.8660254037844387076, 1.000000000000000000, 0.8660254037844387076, 1.000000000000000000, 0.8660254037844387076, 1.000000000000000000, 0.8660254037844387076, 1.000000000000000000, 0.8660254037844387076, 1.000000000000000000, 0.8660254037844387076, 1.000000000000000000, 0.8660254037844387076, 1.000000000000000000, 0.8660254037844387076, 1.000000000000000000, 0.8660254037844387076, 1.000000000000000000, 0.8660254037844387076, 1.000000000000000000, 0.8660254037844387076, 1.000000000000000000, 0.8660254037844387076, 1.000000000000000000, 0.8660254037844387076, 1.000000000000000000, 0.8660254037844387076, 1.000000000000000000, 0.8660254037844387076, 1.000000000000000000, 0.8660254037844387076, 1.000000000000000000, 0.8660254037844387076, 1.000000000000000000, 0.8660254037844387076, 1.000000000000000000, 0.8660254037844387076, 1.000000000000000000, 0.8660254037844387076, 1.000000000000000000, 0.8660254037844387076, 1.000000000000000000, 0.8660254037844387076, 1.000000000000000000, 0.8660254037844387076, 1.000000000000000000, 0.8660254037844387076, 1.000000000000000000, 0.8660254037844387076, 1.000000000000000000, 0.8660254037844387076, 1.000000000000000000, 0.8660254037844387076, 1.000000000000000000, 0.8660254037844387076, 1.000000000000000000, 0.8660254037844387076, 1.000000000000000000, 0.8660254037844387076, 1.000000000000000000, 0.8660254037844387076, 1.000000000000000000, 0.8660254037844387076, 1.000000000000000000, 0.8660254037844387076, 1.000000000000000000, 0.8660254037844387076, 1.000000000000000000, 0.8660254037844387076, 1.000000000000000000, 0.8660254037844387076, 1.000000000000000000, 0.8660254037844387076, 1.000000000000000000, 0.8660254037844387076, 1.000000000000000000, 0.8660254037844387076, 1.000000000000000000, 0.8660254037844387076, 1.000000000000000000, 0.8660254037844387076, 1.000000000000000000, 0.8660254037844387076, 1.000000000000000000, 0.8660254037844387076, 1.000000000000000000, 0.8660254037844387076, 1.000000000000000000, 0.8660254037844387076, 1.000000000000000000, 0.8660254037844387076, 1.000000000000000000, 0.8660254037844387076, 1.000000000000000000, 0.8660254037844387076, 1.000000000000000000, 0.8660254037844387076, 1.000000000000000000, 0.8660254037844387076, 1.000000000000000000, 0.8660254037844387076, 1.000000000000000000, 0.8660254037844387076, 1.000000000000000000, 0.8660254037844387076, 1.000000000000000000, 0.8660254037844387076, 1.000000000000000000, 0.8660254037844387076, 1.000000000000000000, 0.8660254037844387076, 1.000000000000000000, 0.8660254037844387076, 1.000000000000000000, 0.8660254037844387076, 1.000000000000000000, 0.8660254037844387076, 1.000000000000000000, 0.8660254037844387076, 1.000000000000000000, 0.8660254037844387076, 1.000000000000000000, 0.8660254037844387076, 1.000000000000000000, 0.8660254037844387076, 1.000000000000000000, 0.8660254037844387076, 1.000000000000000000, 0.8660254037844387076, 1.000000000000000000, 0.8660254037844387076, 1.000000000000000000, 0.8660254037844387076, 1.000000000000000000, 0.8660254037844387076, 1.000000000000000000, 0.8660254037844387076, 1.000000000000000000, 0.8660254037844387076, 1.000000000000000000, 0.8660254037844387076, 1.000000000000000000, 0.8660254037844387076, 1.000000000000000000, 0.8660254037844387076, 1.000000000000000000, 0.8660254037844387076, 1.000000000000000000, 0.8660254037844387076, 1.000000000000000000, 0.8660254037844387076, 1.000000000000000000, 0.8660254037844387076, 1.000000000000000000, 0.8660254037844387076, 1.000000000000000000, 0.8660254037844387076, 1.000000000000000000, 0.8660254037844387076, 1.000000000000000000, 0.8660254037844387076, 1.000000000000000000, 0.8660254037844387076, 1.000000000000000000, 0.8660254037844387076, 1.000000000000000000, 0.8660254037844387076, 1.000000000000000000, 0.8660254037844387076, 1.000000000000000000, 0.8660254037844387076, 1.000000000000000000, 0.8660254037844387076, 1.000000000000000000, 0.8660254037844387076, 1.000000000000000000, 0.8660254037844387076, 1.000000000000000000, 0.8660254037844387076, 1.000000000000000000, 0.8660254037844387076, 1.000000000000000000, 0.8660254037844387076, 1.000000000000000000, 0.8660254037844387076, 1.000000000000000000, 0.8660254037844387076, 1.000000000000000000, 0.8660254037844387076, 1.000000000000000000, 0.8660254037844387076, 1.000000000000000000, 0.8660254037844387076, 1.000000000000000000, 0.8660254037844387076, 1.000000000000000000, 0.8660254037844387076, 1.000000000000000000, 0.8660254037844387076, 1.000000000000000000, 0.8660254037844387076, 1.000000000000000000, 0.8660254037844387076, 1.000000000000000000, 0.8660254037844387076, 1.000000000000000000, 0.8660254037844387076, 1.000000000000000000, 0.8660254037844387076, 1.000000000000000000, 0.8660254037844387076, 1.000000000000000000, 0.8660254037844387076, 1.000000000000000000, 0.8660254037844387076, 1.000000000000000000, 0.8660254037844387076, 1.000000000000000000, 0.8660254037844387076, 1.000000000000000000, 0.8660254037844387076, 1.000000000000000000, 0.8660254037844387076, 1.000000000000000000, 0.8660254037844387076, 1.000000000000000000, 0.8660254037844387076, 1.000000000000000000, 0.8660254037844387076, 1.000000000000000000, 0.8660254037844387076, 1.000000000000000000, 0.8660254037844387076, 1.000000000000000000, 0.8660254037844387076, 1.000000000000000000, 0.8660254037844387076, 1.000000000000000000, 0.8660254037844387076, 1.000000000000000000, 0.8660254037844387076, 1.000000000000000000, 0.8660254037844387076, 1.000000000000000000, 0.8660254037844387076, 1.000000000000000000, 0.8660254037844387076, 1.000000000000000000, 0.8660254037844387076, 1.000000000000000000, 0.8660254037844387076, 1.000000000000000000, 0.8660254037844387076, 1.000000000000000000, 0.8660254037844387076, 1.000000000000000000, 0.8660254037844387076, 1.000000000000000000, 0.8660254037844387076, 1.000000000000000000, 0.8660254037844387076, 1.000000000000000000, 0.8660254037844387076, 1.000000000000000000, 0.8660254037844387076, 1.000000000000000000, 0.8660254037844387076, 1.000000000000000000, 0.8660254037844387076, 1.000000000000000000, 0.8660254037844387076, 1.000000000000000000, 0.8660254037844387076, 1.000000000000000000, 0.8660254037844387076, 1.000000000000000000, 0.8660254037844387076, 1.000000000000000000, 0.8660254037844387076, 1.000000000000000000, 0.8660254037844387076, 1.000000000000000000, 0.8660254037844387076, 1.000000000000000000, 0.8660254037844387076, 1.000000000000000000, 0.8660254037844387076, 1.000000000000000000, 0.8660254037844387076, 1.000000000000000000, 0.8660254037844387076, 1.000000000000000000, 0.8660254037844387076, 1.000000000000000000, 0.8660254037844387076, 1.000000000000000000, 0.8660254037844387076, 1.000000000000000000, 0.8660254037844387076, 1.000000000000000000, 0.8660254037844387076, 1.000000000000000000, 0.8660254037844387076, 1.000000000000000000, 0.8660254037844387076, 1.000000000000000000, 0.8660254037844387076, 1.000000000000000000, 0.8660254037844387076, 1.000000000000000000, 0.8660254037844387076, 1.000000000000000000, 0.8660254037844387076, 1.000000000000000000, 0.8660254037844387076, 1.000000000000000000, 0.8660254037844387076, 1.000000000000000000, 0.8660254037844387076, 1.000000000000000000, 0.8660254037844387076, 1.000000000000000000, 0.8660254037844387076, 1.000000000000000000, 0.8660254037844387076, 1.000000000000000000, 0.8660254037844387076, 1.000000000000000000, 0.8660254037844387076, 1.000000000000000000, 0.8660254037844387076, 1.000000000000000000, 0.8660254037844387076, 1.000000000000000000, 0.8660254037844387076, 1.000000000000000000, 0.8660254037844387076, 1.000000000000000000, 0.8660254037844387076, 1.000000000000000000, 0.8660254037844387076, 1.000000000000000000, 0.8660254037844387076, 1.000000000000000000, 0.8660254037844387076, 1.000000000000000000, 0.8660254037844387076, 1.000000000000000000, 0.8660254037844387076, 1.000000000000000000, 0.8660254037844387076, 1.000000000000000000, 0.8660254037844387076, 1.000000000000000000, 0.8660254037844387076, 1.000000000000000000, 0.8660254037844387076, 1.000000000000000000, 0.8660254037844387076, 1.000000000000000000, 0.8660254037844387076, 1.000000000000000000, 0.8660254037844387076, 1.000000000000000000, 0.8660254037844387076, 1.000000000000000000, 0.8660254037844387076, 1.000000000000000000, 0.8660254037844387076, 1.000000000000000000, 0.8660254037844387076, 1.000000000000000000, 0.8660254037844387076, 1.000000000000000000, 0.8660254037844387076, 1.000000000000000000, 0.8660254037844387076, 1.000000000000000000, 0.8660254037844387076, 1.000000000000000000, 0.8660254037844387076, 1.000000000000000000, 0.8660254037844387076, 1.000000000000000000, 0.8660254037844387076, 1.000000000000000000, 0.8660254037844387076, 1.000000000000000000, 0.8660254037844387076, 1.000000000000000000, 0.8660254037844387076, 1.000000000000000000, 0.8660254037844387076, 1.000000000000000000, 0.8660254037844387076, 1.000000000000000000, 0.8660254037844387076, 1.000000000000000000, 0.8660254037844387076, 1.000000000000000000, 0.8660254037844387076, 1.000000000000000000, 0.8660254037844387076, 1.000000000000000000, 0.8660254037844387076, 1.000000000000000000 ) ) 
 REPRESENTATION_ITEM ( '' )  );
#25724 = SURFACE_STYLE_FILL_AREA ( #2383 ) ;
#25725 = CARTESIAN_POINT ( 'NONE',  ( 149.5461002691896510, -2.071067811865468400, 4.999999999999989342 ) ) ;
#25726 = CARTESIAN_POINT ( 'NONE',  ( 0.000000000000000000, 0.000000000000000000, 0.000000000000000000 ) ) ;
#25727 = DIRECTION ( 'NONE',  ( -1.000000000000000000, -1.665334536937736783E-16, -2.220446049250315546E-16 ) ) ;
#25728 = CARTESIAN_POINT ( 'NONE',  ( 156.0937500000000284, 6.000000000000005329, 2.485281374238585972 ) ) ;
#25729 = FILL_AREA_STYLE_COLOUR ( '', #1557 ) ;
#25730 = CARTESIAN_POINT ( 'NONE',  ( 6.000000000000000888, -1.859271017917181981E-14, -173.1636751345948539 ) ) ;
#25731 = CARTESIAN_POINT ( 'NONE',  ( -5.999999999999963585, -1.487416814333745711E-14, -132.8363248654052597 ) ) ;
#25732 = CARTESIAN_POINT ( 'NONE',  ( 118.9372167782374277, -0.7662911109077686911, 1.849990392679652151 ) ) ;
#25733 = FACE_OUTER_BOUND ( 'NONE', #21637, .T. ) ;
#25734 = ORIENTED_EDGE ( 'NONE', *, *, #9012, .F. ) ;
#25735 = CARTESIAN_POINT ( 'NONE',  ( 148.6875000000000284, 4.242640687119269671, 4.242640687119298093 ) ) ;
#25736 = DIRECTION ( 'NONE',  ( -8.326672684688674053E-17, -2.081668171172168513E-17, 1.000000000000000000 ) ) ;
#25737 = CARTESIAN_POINT ( 'NONE',  ( 113.0627832217621886, -0.7662911109076184779, -1.849990392679291551 ) ) ;
#25738 = LINE ( 'NONE', #18549, #7260 ) ;
#25739 = EDGE_LOOP ( 'NONE', ( #20280, #27004, #27369, #3121 ) ) ;
#25740 = VERTEX_POINT ( 'NONE', #29046 ) ;
#25741 = EDGE_LOOP ( 'NONE', ( #12694, #16613, #13200, #30117 ) ) ;
#25742 = CARTESIAN_POINT ( 'NONE',  ( 6.350852961086080661, -9.614813431917819062E-14, -88.87500000000000000 ) ) ;
#25743 = CARTESIAN_POINT ( 'NONE',  ( 5.412658773652739619, 3.124999999999988898, -108.6830127018922383 ) ) ;
#25744 = VERTEX_POINT ( 'NONE', #17723 ) ;
#25745 = CARTESIAN_POINT ( 'NONE',  ( 1.971541444415901845, 10.82814027403869694, -30.68027829220103442 ) ) ;
#25746 = CARTESIAN_POINT ( 'NONE',  ( 154.7663997308104342, -4.999999999999989342, -2.071067811865468400 ) ) ;
#25747 = ADVANCED_FACE ( 'NONE', ( #941 ), #26591, .T. ) ;
#25748 = CARTESIAN_POINT ( 'NONE',  ( 4.763139720814407951, 2.750000000000002665, -166.7500000000000000 ) ) ;
#25749 = CARTESIAN_POINT ( 'NONE',  ( -5.196152422706573404, -3.000000000000002665, -106.2886751345948397 ) ) ;
#25750 = CARTESIAN_POINT ( 'NONE',  ( 3.464101615137852974, 5.999999999999884537, -46.91367513459483263 ) ) ;
#25751 = FILL_AREA_STYLE ('',( #23471 ) ) ;
#25752 = CARTESIAN_POINT ( 'NONE',  ( 3.175426480543072749, 5.499999999999865885, -172.6250000000000284 ) ) ;
#25753 = LINE ( 'NONE', #22851, #3689 ) ;
#25754 = CARTESIAN_POINT ( 'NONE',  ( 4.763139720814407951, 2.750000000000002665, -157.7500000000000568 ) ) ;
#25755 = CARTESIAN_POINT ( 'NONE',  ( 110.6874999999997868, -1.035533905932689347, -2.499999999999844569 ) ) ;
#25756 = CIRCLE ( 'NONE', #19874, 1.000000000000000888 ) ;
#25757 = CARTESIAN_POINT ( 'NONE',  ( 0.000000000000000000, 5.499999999999991118, -99.00000000000002842 ) ) ;
#25758 = CARTESIAN_POINT ( 'NONE',  ( -5.999999999999963585, 3.021315404115421074E-15, -177.8363248654052029 ) ) ;
#25759 = CARTESIAN_POINT ( 'NONE',  ( 144.6636751345948255, 0.000000000000000000, 5.500000000000005329 ) ) ;
#25760 = CARTESIAN_POINT ( 'NONE',  ( -2.775557561562891351E-14, -5.500000000000115463, -90.75000000000000000 ) ) ;
#25761 = EDGE_CURVE ( 'NONE', #3256, #20541, #16487, .T. ) ;
#25762 = CARTESIAN_POINT ( 'NONE',  ( 116.0000000000000142, 0.000000000000000000, 0.000000000000000000 ) ) ;
#25763 = CARTESIAN_POINT ( 'NONE',  ( 160.4211002691896510, -4.999999999999989342, -2.071067811865468400 ) ) ;
#25764 = CARTESIAN_POINT ( 'NONE',  ( 0.8492726096241208777, -15.39617198623466976, 8.319207606560656387 ) ) ;
#25765 = ORIENTED_EDGE ( 'NONE', *, *, #16912, .F. ) ;
#25766 = CARTESIAN_POINT ( 'NONE',  ( 10.18750000000001954, -2.649519052838298805, -1.097466725451559322 ) ) ;
#25767 = APPLICATION_CONTEXT ( 'automotive_design' ) ;
#25768 = CARTESIAN_POINT ( 'NONE',  ( 114.3124999999997726, -1.035533905932719101, 2.500000000000205169 ) ) ;
#25769 = CARTESIAN_POINT ( 'NONE',  ( 15.85117513459492145, -2.499999999999964473, -1.035533905932749299 ) ) ;
#25770 = AXIS2_PLACEMENT_3D ( 'NONE', #1312, #10879, #13041 ) ;
#25771 = CARTESIAN_POINT ( 'NONE',  ( 106.9377832217621318, -1.849990392679441875, -0.7662911109075883909 ) ) ;
#25772 = CARTESIAN_POINT ( 'NONE',  ( 24.03867513459490013, 1.665334536937734811E-13, -2.500000000000002220 ) ) ;
#25773 = VERTEX_POINT ( 'NONE', #15432 ) ;
#25774 = CARTESIAN_POINT ( 'NONE',  ( 15.14882486540524198, -2.499999999999904521, 1.035533905932749299 ) ) ;
#25775 = CARTESIAN_POINT ( 'NONE',  ( -19.49999999999998224, -24.99999999999999289, -8.000000000000007105 ) ) ;
#25776 = ORIENTED_EDGE ( 'NONE', *, *, #28436, .T. ) ;
#25777 = LINE ( 'NONE', #4724, #19406 ) ;
#25778 = ORIENTED_EDGE ( 'NONE', *, *, #4768, .F. ) ;
#25779 = CARTESIAN_POINT ( 'NONE',  ( 152.7187500000000284, 2.485281374238555774, -6.000000000000005329 ) ) ;
#25780 = ORIENTED_EDGE ( 'NONE', *, *, #11831, .F. ) ;
#25781 = CIRCLE ( 'NONE', #4675, 14.49999999999998579 ) ;
#25782 = CARTESIAN_POINT ( 'NONE',  ( 3.175426480543072749, 5.499999999999865885, -111.1249999999999716 ) ) ;
#25783 = CARTESIAN_POINT ( 'NONE',  ( 22.37500000000008882, 2.649519052838555933, -5.551115123125782702E-14 ) ) ;
#25784 = CARTESIAN_POINT ( 'NONE',  ( 5.412658773652739619, 3.124999999999988898, -132.6830127018922667 ) ) ;
#25785 = EDGE_LOOP ( 'NONE', ( #8871, #27554, #20837, #7525 ) ) ;
#25786 = CARTESIAN_POINT ( 'NONE',  ( -5.999999999999963585, 1.780251999655701777E-13, -47.33632486540523132 ) ) ;
#25787 = CARTESIAN_POINT ( 'NONE',  ( -5.412658773652739619, 3.124999999999975131, -171.8169872981077901 ) ) ;
#25788 = CARTESIAN_POINT ( 'NONE',  ( 108.3124999999997442, -1.035533905932629173, 2.500000000000205169 ) ) ;
#25789 = FILL_AREA_STYLE_COLOUR ( '', #8645 ) ;
#25790 = EDGE_CURVE ( 'NONE', #27478, #14802, #12347, .T. ) ;
#25791 = ORIENTED_EDGE ( 'NONE', *, *, #6195, .F. ) ;
#25792 = CARTESIAN_POINT ( 'NONE',  ( -6.000000000000000888, 1.067854986875958443E-15, 7.560779664488942560E-35 ) ) ;
#25793 = CARTESIAN_POINT ( 'NONE',  ( 6.000000000000000888, 7.762456499804234384E-14, -133.5863248654052029 ) ) ;
#25794 = CARTESIAN_POINT ( 'NONE',  ( 3.175426480543072749, 5.499999999999865885, -178.6250000000000284 ) ) ;
#25795 = CARTESIAN_POINT ( 'NONE',  ( 106.6252832217623023, 2.775557561562891351E-14, 1.849990392679634610 ) ) ;
#25796 = CARTESIAN_POINT ( 'NONE',  ( 7.216878364870455975, -6.409875621278545621E-14, -176.3080127018922667 ) ) ;
#25797 = CARTESIAN_POINT ( 'NONE',  ( -0.3854532388872504156, -9.307273380556397413, -4.200333198739659935 ) ) ;
#25798 = CARTESIAN_POINT ( 'NONE',  ( 6.000000000000000888, -1.859271017917181981E-14, -105.0863248654052313 ) ) ;
#25799 = CARTESIAN_POINT ( 'NONE',  ( 6.000000000000000888, 7.762456499804234384E-14, -123.6636751345948255 ) ) ;
#25800 = EDGE_CURVE ( 'NONE', #29296, #26144, #7015, .T. ) ;
#25801 = CARTESIAN_POINT ( 'NONE',  ( -3.175426480542816510, -5.500000000000057732, -119.3750000000000284 ) ) ;
#25802 = ORIENTED_EDGE ( 'NONE', *, *, #21028, .T. ) ;
#25803 = CARTESIAN_POINT ( 'NONE',  ( 22.75000000000004974, 1.873492889144956486, 1.873492889144734441 ) ) ;
#25804 = AXIS2_PLACEMENT_3D ( 'NONE', #15755, #27212, #15600 ) ;
#25805 = CARTESIAN_POINT ( 'NONE',  ( -0.07769256095283472163, -15.23231281889969146, 7.500000000000007105 ) ) ;
#25806 = CYLINDRICAL_SURFACE ( 'NONE', #23903, 0.5000000000000004441 ) ;
#25807 = CARTESIAN_POINT ( 'NONE',  ( 116.7886751345947687, -2.000000000000001776, 0.000000000000000000 ) ) ;
#25808 = ORIENTED_EDGE ( 'NONE', *, *, #29523, .T. ) ;
#25809 = DIRECTION ( 'NONE',  ( -1.000000000000000000, -1.665334536937731113E-16, 1.526556658859586792E-16 ) ) ;
#25810 = CARTESIAN_POINT ( 'NONE',  ( -5.999999999999963585, 8.134310703387671600E-14, -121.4136751345948255 ) ) ;
#25811 = CARTESIAN_POINT ( 'NONE',  ( 110.4997167782375698, 1.308140751793668288, -1.308140751793640533 ) ) ;
#25812 = CARTESIAN_POINT ( 'NONE',  ( 6.000000000000000888, 1.743066579297358182E-13, -108.6636751345948255 ) ) ;
#25813 = ORIENTED_EDGE ( 'NONE', *, *, #9633, .F. ) ;
#25814 = CARTESIAN_POINT ( 'NONE',  ( 0.000000000000000000, -5.999999999999991118, -77.53867513459483973 ) ) ;
#25815 =( BOUNDED_CURVE ( )  B_SPLINE_CURVE ( 2, ( #17962, #10575, #6392, #5934, #17496, #3928, #4090, #12903, #1024 ),
 .UNSPECIFIED., .F., .T. ) 
 B_SPLINE_CURVE_WITH_KNOTS ( ( 3, 2, 2, 2, 3 ),
 ( 0.1138888888888888173, 0.1148148148148148140, 0.1166666666666666963, 0.1185185185185184675, 0.1194444444444444642 ),
 .UNSPECIFIED. ) 
 CURVE ( )  GEOMETRIC_REPRESENTATION_ITEM ( )  RATIONAL_B_SPLINE_CURVE ( ( 0.9330127018922194093, 0.9330127018922154125, 1.000000000000000000, 0.8660254037844388186, 1.000000000000000000, 0.8660254037844388186, 1.000000000000000000, 0.9330127018922154125, 0.9330127018922194093 ) ) 
 REPRESENTATION_ITEM ( '' )  );
#25816 = DIRECTION ( 'NONE',  ( -7.147005652999508048E-36, 5.642372883946980038E-36, 1.000000000000000000 ) ) ;
#25817 = ORIENTED_EDGE ( 'NONE', *, *, #17878, .T. ) ;
#25818 = CARTESIAN_POINT ( 'NONE',  ( 3.464101615137757051, -5.999999999999979572, -141.9136751345948255 ) ) ;
#25819 = CARTESIAN_POINT ( 'NONE',  ( 137.4375000000000568, -4.242640687119298093, -4.242640687119298093 ) ) ;
#25820 = CIRCLE ( 'NONE', #9649, 0.5000000000000004441 ) ;
#25821 = ORIENTED_EDGE ( 'NONE', *, *, #13077, .T. ) ;
#25822 = CARTESIAN_POINT ( 'NONE',  ( 5.412658773652712085, -3.125000000000086153, -141.0669872981078470 ) ) ;
#25823 = CARTESIAN_POINT ( 'NONE',  ( 11.43750000000009415, 2.649519052838478661, 1.097466725451499370 ) ) ;
#25824 = VECTOR ( 'NONE', #24951, 1000.000000000000000 ) ;
#25825 = CARTESIAN_POINT ( 'NONE',  ( 136.0000000000000284, -9.165151389911695645, -8.500000000000007105 ) ) ;
#25826 = ADVANCED_FACE ( 'NONE', ( #1100 ), #17271, .T. ) ;
#25827 = CARTESIAN_POINT ( 'NONE',  ( 5.196152422706629359, -2.999999999999988898, -129.7886751345947971 ) ) ;
#25828 = CARTESIAN_POINT ( 'NONE',  ( 117.7113248654050466, 2.000000000000085265, 0.000000000000000000 ) ) ;
#25829 = CARTESIAN_POINT ( 'NONE',  ( 146.8913997308104626, -2.071067811865468400, 4.999999999999989342 ) ) ;
#25830 = DIRECTION ( 'NONE',  ( 0.000000000000000000, 0.000000000000000000, -1.000000000000000000 ) ) ;
#25831 = CARTESIAN_POINT ( 'NONE',  ( -4.999999999999886313, -69.50000000000001421, 7.500000000000007105 ) ) ;
#25832 = DIRECTION ( 'NONE',  ( 1.000000000000000000, -0.000000000000000000, -0.000000000000000000 ) ) ;
#25833 = CARTESIAN_POINT ( 'NONE',  ( 24.64495393282636115, -2.193871126647821246, 0.8697444040583612868 ) ) ;
#25834 = FACE_BOUND ( 'NONE', #5454, .T. ) ;
#25835 = CARTESIAN_POINT ( 'NONE',  ( 111.6874999999997584, -1.035533905932719101, -2.499999999999844569 ) ) ;
#25836 = EDGE_CURVE ( 'NONE', #22177, #7342, #5547, .T. ) ;
#25837 = PRESENTATION_STYLE_ASSIGNMENT (( #16512 ) ) ;
#25838 = CARTESIAN_POINT ( 'NONE',  ( 5.196152422706629359, 3.000000000000002665, -149.0386751345948539 ) ) ;
#25839 = STYLED_ITEM ( 'NONE', ( #16969 ), #6539 ) ;
#25840 = ORIENTED_EDGE ( 'NONE', *, *, #13949, .T. ) ;
#25841 = CARTESIAN_POINT ( 'NONE',  ( 3.175426480543072749, 5.499999999999865885, -52.62500000000002842 ) ) ;
#25842 = CARTESIAN_POINT ( 'NONE',  ( -9.999999999999994671, -71.00000000000002842, 4.000000000000003553 ) ) ;
#25843 = VERTEX_POINT ( 'NONE', #3239 ) ;
#25844 = CARTESIAN_POINT ( 'NONE',  ( 104.8749999999998437, 1.767766952966320915, -1.767766952966431937 ) ) ;
#25845 = CARTESIAN_POINT ( 'NONE',  ( 141.3750000000000284, 0.000000000000000000, 6.000000000000005329 ) ) ;
#25846 = CARTESIAN_POINT ( 'NONE',  ( 3.608439182435180470, 6.249999999999982236, -103.1919872981078328 ) ) ;
#25847 = CARTESIAN_POINT ( 'NONE',  ( -6.000000000000000888, 1.067854986875958443E-15, 7.560779664488942560E-35 ) ) ;
#25848 = CARTESIAN_POINT ( 'NONE',  ( 159.4538997308104058, -2.071067811865468400, -4.999999999999989342 ) ) ;
#25849 = CARTESIAN_POINT ( 'NONE',  ( 117.8124999999998437, 1.035533905932869425, -2.499999999999784173 ) ) ;
#25850 = VERTEX_POINT ( 'NONE', #12666 ) ;
#25851 = AXIS2_PLACEMENT_3D ( 'NONE', #14380, #2949, #7276 ) ;
#25852 = CARTESIAN_POINT ( 'NONE',  ( 4.763139720814407951, 2.750000000000002665, -141.2500000000000000 ) ) ;
#25853 = ORIENTED_EDGE ( 'NONE', *, *, #12260, .T. ) ;
#25854 = VERTEX_POINT ( 'NONE', #22003 ) ;
#25855 = CARTESIAN_POINT ( 'NONE',  ( -5.999999999999919176, 1.607695154586804565, -162.9033121635129646 ) ) ;
#25856 = CARTESIAN_POINT ( 'NONE',  ( -3.175426480542816510, 5.499999999999865885, -65.87500000000002842 ) ) ;
#25857 =( BOUNDED_CURVE ( )  B_SPLINE_CURVE ( 2, ( #1287, #18073, #24797, #6211, #3744, #3890, #13321, #13178, #22662 ),
 .UNSPECIFIED., .F., .F. ) 
 B_SPLINE_CURVE_WITH_KNOTS ( ( 3, 2, 2, 2, 3 ),
 ( 0.1361111111111110716, 0.1370370370370370683, 0.1388888888888888395, 0.1407407407407407218, 0.1416666666666667185 ),
 .UNSPECIFIED. ) 
 CURVE ( )  GEOMETRIC_REPRESENTATION_ITEM ( )  RATIONAL_B_SPLINE_CURVE ( ( 0.9330127018922194093, 0.9330127018922154125, 1.000000000000000000, 0.8660254037844388186, 1.000000000000000000, 0.8660254037844388186, 1.000000000000000000, 0.9330127018922154125, 0.9330127018922194093 ) ) 
 REPRESENTATION_ITEM ( '' )  );
#25858 = ADVANCED_FACE ( 'NONE', ( #11112 ), #16051, .F. ) ;
#25859 = DIRECTION ( 'NONE',  ( -7.147005652999508048E-36, 5.642372883946980038E-36, 1.000000000000000000 ) ) ;
#25860 = CARTESIAN_POINT ( 'NONE',  ( -3.464101615137725076, 5.999999999999979572, -66.16367513459479710 ) ) ;
#25861 = EDGE_CURVE ( 'NONE', #152, #12734, #5828, .T. ) ;
#25862 = CARTESIAN_POINT ( 'NONE',  ( 2.775557561562891351E-14, -6.250000000000061284, -82.18301270189220986 ) ) ;
#25863 = CARTESIAN_POINT ( 'NONE',  ( -3.464101615137757051, -5.999999999999979572, -113.6636751345948113 ) ) ;
#25864 = CARTESIAN_POINT ( 'NONE',  ( 105.1247167782375840, -1.849990392679468076, 0.000000000000000000 ) ) ;
#25865 =( NAMED_UNIT ( * ) SI_UNIT ( $, .STERADIAN. ) SOLID_ANGLE_UNIT ( ) );
#25866 = CARTESIAN_POINT ( 'NONE',  ( 120.8752832217622029, -1.849990392679523588, 0.000000000000000000 ) ) ;
#25867 = CARTESIAN_POINT ( 'NONE',  ( 3.175426480543072749, -5.500000000000105693, -150.6250000000000284 ) ) ;
#25868 = CARTESIAN_POINT ( 'NONE',  ( 140.0510979238436278, -8.941207700098154021, 8.003589737453340902 ) ) ;
#25869 = CARTESIAN_POINT ( 'NONE',  ( -3.608439182435052128, -6.250000000000110134, -164.8080127018922667 ) ) ;
#25870 = CARTESIAN_POINT ( 'NONE',  ( -5.196152422706573404, -3.000000000000002665, -149.2113248654052313 ) ) ;
#25871 = CARTESIAN_POINT ( 'NONE',  ( 105.3363248654050750, -1.414213562373256572, -1.414213562372923505 ) ) ;
#25872 = CARTESIAN_POINT ( 'NONE',  ( 4.763139720814407951, -2.749999999999988454, -78.50000000000001421 ) ) ;
#25873 = CARTESIAN_POINT ( 'NONE',  ( 4.763139720814407951, 2.750000000000002665, -69.25000000000002842 ) ) ;
#25874 = CARTESIAN_POINT ( 'NONE',  ( 155.8125000000000284, 4.242640687119298093, -4.242640687119298093 ) ) ;
#25875 =( NAMED_UNIT ( * ) SI_UNIT ( $, .STERADIAN. ) SOLID_ANGLE_UNIT ( ) );
#25876 = CARTESIAN_POINT ( 'NONE',  ( 119.7886751345947829, -1.999999999999946265, 3.330669073875469621E-13 ) ) ;
#25877 = CARTESIAN_POINT ( 'NONE',  ( 118.5622167782375698, 1.849990392679621953, -0.7662911109077087390 ) ) ;
#25878 = VERTEX_POINT ( 'NONE', #22924 ) ;
#25879 = CARTESIAN_POINT ( 'NONE',  ( 152.9062500000000000, 6.000000000000005329, -2.485281374238555774 ) ) ;
#25880 = CARTESIAN_POINT ( 'NONE',  ( 0.000000000000000000, 0.000000000000000000, -200.0000000000000000 ) ) ;
#25881 = AXIS2_PLACEMENT_3D ( 'NONE', #880, #10128, #21944 ) ;
#25882 = CARTESIAN_POINT ( 'NONE',  ( 115.6252832217622597, 0.000000000000000000, 1.849990392679523588 ) ) ;
#25883 = VERTEX_POINT ( 'NONE', #16199 ) ;
#25884 = VECTOR ( 'NONE', #27875, 1000.000000000000000 ) ;
#25885 = CARTESIAN_POINT ( 'NONE',  ( 21.81250000000009592, 0.8284271247462955401, -2.000000000000151879 ) ) ;
#25886 = CARTESIAN_POINT ( 'NONE',  ( 5.412658773652739619, 3.124999999999988898, -155.8169872981078470 ) ) ;
#25887 = EDGE_LOOP ( 'NONE', ( #12649, #25141, #1321, #19540 ) ) ;
#25888 = CARTESIAN_POINT ( 'NONE',  ( -6.350852961085760029, -1.281975124255709124E-13, -89.62500000000000000 ) ) ;
#25889 = COLOUR_RGB ( '', 0.09019608, 0.27058824, 0.51372549) ;
#25890 = AXIS2_PLACEMENT_3D ( 'NONE', #19798, #29144, #26833 ) ;
#25891 =( BOUNDED_CURVE ( )  B_SPLINE_CURVE ( 2, ( #27182, #22139, #8772, #3984, #8458, #5993, #27333, #18159, #27474 ),
 .UNSPECIFIED., .F., .F. ) 
 B_SPLINE_CURVE_WITH_KNOTS ( ( 3, 2, 2, 2, 3 ),
 ( 0.1750000000000000167, 0.1759259259259259300, 0.1777777777777777846, 0.1796296296296296391, 0.1805555555555555525 ),
 .UNSPECIFIED. ) 
 CURVE ( )  GEOMETRIC_REPRESENTATION_ITEM ( )  RATIONAL_B_SPLINE_CURVE ( ( 0.9330127018922194093, 0.9330127018922204085, 1.000000000000000000, 0.8660254037844388186, 1.000000000000000000, 0.8660254037844388186, 1.000000000000000000, 0.9330127018922205195, 0.9330127018922196314 ) ) 
 REPRESENTATION_ITEM ( '' )  );
#25892 = ADVANCED_FACE ( 'NONE', ( #1867 ), #29818, .F. ) ;
#25893 = ORIENTED_EDGE ( 'NONE', *, *, #2889, .F. ) ;
#25894 = CARTESIAN_POINT ( 'NONE',  ( 156.5476497308104342, 0.000000000000000000, -5.000000000000004441 ) ) ;
#25895 = CARTESIAN_POINT ( 'NONE',  ( 7.216878364870455975, -6.409875621278545621E-14, -47.30801270189223118 ) ) ;
#25896 =( BOUNDED_CURVE ( )  B_SPLINE_CURVE ( 2, ( #28714, #14782, #24126, #12498, #14037, #9227, #2010, #11254, #18322 ),
 .UNSPECIFIED., .F., .F. ) 
 B_SPLINE_CURVE_WITH_KNOTS ( ( 3, 2, 2, 2, 3 ),
 ( 0.4916666666666666408, 0.4925925925925925819, 0.4944444444444444642, 0.4962962962962962910, 0.4972222222222222321 ),
 .UNSPECIFIED. ) 
 CURVE ( )  GEOMETRIC_REPRESENTATION_ITEM ( )  RATIONAL_B_SPLINE_CURVE ( ( 0.9330127018922194093, 0.9330127018922174109, 1.000000000000000000, 0.8660254037844388186, 1.000000000000000000, 0.8660254037844388186, 1.000000000000000000, 0.9330127018922194093, 0.9330127018922194093 ) ) 
 REPRESENTATION_ITEM ( '' )  );
#25897 = CARTESIAN_POINT ( 'NONE',  ( -3.175426480542816066, 5.499999999999865885, -172.3750000000000568 ) ) ;
#25898 = CARTESIAN_POINT ( 'NONE',  ( -1.110223024625164676E-16, 2.000000000000012879, 2.021286199229734960E-15 ) ) ;
#25899 = AXIS2_PLACEMENT_3D ( 'NONE', #1391, #10801, #20445 ) ;
#25900 = CARTESIAN_POINT ( 'NONE',  ( 6.350852961086080661, -9.614813431917819062E-14, -157.8750000000000000 ) ) ;
#25901 = CARTESIAN_POINT ( 'NONE',  ( 113.5624999999997158, -2.499999999999964473, -1.035533905932689347 ) ) ;
#25902 = CARTESIAN_POINT ( 'NONE',  ( -4.763139720814407951, -2.750000000000016431, -103.0000000000000426 ) ) ;
#25903 = B_SPLINE_CURVE_WITH_KNOTS ( 'NONE', 3,
 ( #3777, #1478, #22695, #13658, #8712, #29735, #18251, #27418, #11348, #15819 ),
 .UNSPECIFIED., .F., .F.,
 ( 4, 2, 2, 2, 4 ),
 ( 0.000000000000000000, 0.0004454033597584232786, 0.0008908067195168465572, 0.001336210079275269944, 0.001781613439033693114 ),
 .UNSPECIFIED. ) ;
#25904 = CARTESIAN_POINT ( 'NONE',  ( 0.000000000000000000, 0.000000000000000000, 0.000000000000000000 ) ) ;
#25905 = DIRECTION ( 'NONE',  ( -2.220446049250313574E-16, 1.000000000000000000, 8.049116928532386890E-16 ) ) ;
#25907 = CARTESIAN_POINT ( 'NONE',  ( 3.175426480543072749, -5.500000000000105693, -90.62500000000001421 ) ) ;
#25906 = CARTESIAN_POINT ( 'NONE',  ( -4.763139720814407951, 2.749999999999946709, -157.2500000000000000 ) ) ;
#25908 = CARTESIAN_POINT ( 'NONE',  ( 13.96132486540527218, 1.110223024625156540E-13, 2.499999999999946709 ) ) ;
#25909 = CARTESIAN_POINT ( 'NONE',  ( 156.5773502691896510, 5.000000000000004441, 0.000000000000000000 ) ) ;
#25910 = LINE ( 'NONE', #4858, #21902 ) ;
#25911 = VERTEX_POINT ( 'NONE', #27804 ) ;
#25912 = UNCERTAINTY_MEASURE_WITH_UNIT (LENGTH_MEASURE( 1.000000000000000082E-05 ), #22010, 'distance_accuracy_value', 'NONE');
#25913 = CARTESIAN_POINT ( 'NONE',  ( 111.4999999999998863, -2.499999999999946709, 1.110223024625156540E-13 ) ) ;
#25914 = CARTESIAN_POINT ( 'NONE',  ( 0.000000000000000000, 5.499999999999991118, -46.49999999999998579 ) ) ;
#25915 = CARTESIAN_POINT ( 'NONE',  ( 106.3127832217621318, 1.849990392679501827, -0.7662911109075883909 ) ) ;
#25916 = CARTESIAN_POINT ( 'NONE',  ( 6.000000000000000888, -3.330669073875464691E-16, -7.560779664488942560E-35 ) ) ;
#25917 = EDGE_LOOP ( 'NONE', ( #3810, #30186, #19229, #24404 ) ) ;
#25918 = CARTESIAN_POINT ( 'NONE',  ( 15.46132486540530238, 1.110223024625156540E-13, -2.500000000000057732 ) ) ;
#25919 = CARTESIAN_POINT ( 'NONE',  ( -0.07852715771744070428, -14.93815133716600307, -8.093175384816596818 ) ) ;
#25920 = CARTESIAN_POINT ( 'NONE',  ( 105.7497167782376266, 1.308140751793696044, 1.308140751793640533 ) ) ;
#25921 = ADVANCED_FACE ( 'NONE', ( #20779 ), #6629, .T. ) ;
#25922 = DIRECTION ( 'NONE',  ( 1.000000000000000000, 0.000000000000000000, 0.000000000000000000 ) ) ;
#25923 = ORIENTED_EDGE ( 'NONE', *, *, #17599, .T. ) ;
#25924 = CARTESIAN_POINT ( 'NONE',  ( 149.5312500000000284, -2.485281374238555774, -6.000000000000005329 ) ) ;
#25925 = CARTESIAN_POINT ( 'NONE',  ( 3.175426480543072749, 5.499999999999865885, -117.1250000000000142 ) ) ;
#25926 = CARTESIAN_POINT ( 'NONE',  ( 22.18750000000000000, 1.097466725451559322, -2.649519052838298805 ) ) ;
#25927 = ADVANCED_FACE ( 'NONE', ( #20622 ), #11269, .T. ) ;
#25928 = CARTESIAN_POINT ( 'NONE',  ( -7.216878364870328078, 0.000000000000000000, -130.5580127018922383 ) ) ;
#25929 = ORIENTED_EDGE ( 'NONE', *, *, #5311, .F. ) ;
#25930 = SURFACE_SIDE_STYLE ('',( #6737 ) ) ;
#25931 = CARTESIAN_POINT ( 'NONE',  ( 2.775557561562891351E-14, -6.250000000000061284, -168.3169872981078470 ) ) ;
#25932 = CARTESIAN_POINT ( 'NONE',  ( 108.7499999999998579, 8.326672684688674053E-14, -2.499999999999835687 ) ) ;
#25933 = CARTESIAN_POINT ( 'NONE',  ( 133.1101497308104342, 3.535533905932725318, 3.535533905932725318 ) ) ;
#25934 = EDGE_LOOP ( 'NONE', ( #113, #8924, #2862, #23077 ) ) ;
#25935 = CARTESIAN_POINT ( 'NONE',  ( 3.464101615137852974, 5.999999999999884537, -95.83632486540517448 ) ) ;
#25936 = FILL_AREA_STYLE_COLOUR ( '', #2045 ) ;
#25937 = FACE_OUTER_BOUND ( 'NONE', #14628, .T. ) ;
#25938 = CARTESIAN_POINT ( 'NONE',  ( 109.0627832217621176, -0.7662911109076785410, -1.849990392679171425 ) ) ;
#25939 = CARTESIAN_POINT ( 'NONE',  ( -3.608439182435115633, 6.249999999999965361, -180.3080127018922667 ) ) ;
#25940 = DIRECTION ( 'NONE',  ( 5.551115123125783935E-17, -1.000000000000000000, -8.881784197001254296E-16 ) ) ;
#25941 = FILL_AREA_STYLE_COLOUR ( '', #10319 ) ;
#25942 = CARTESIAN_POINT ( 'NONE',  ( 136.0000000000000284, 0.000000000000000000, 0.000000000000000000 ) ) ;
#25943 = UNCERTAINTY_MEASURE_WITH_UNIT (LENGTH_MEASURE( 1.000000000000000082E-05 ), #4123, 'distance_accuracy_value', 'NONE');
#25944 = CARTESIAN_POINT ( 'NONE',  ( -6.350852961085760029, -1.281975124255709124E-13, -110.6249999999999858 ) ) ;
#25945 = CARTESIAN_POINT ( 'NONE',  ( 134.9999999999992895, -7.147597648790188885, -8.399649850026122522 ) ) ;
#25946 = CARTESIAN_POINT ( 'NONE',  ( 0.000000000000000000, 0.000000000000000000, 0.000000000000000000 ) ) ;
#25947 = EDGE_LOOP ( 'NONE', ( #9348, #333, #8354, #6234, #9256, #13881, #20330, #18848, #24972, #29063, #24250, #5910, #14270, #18210, #15539, #414, #6490, #7380, #18624, #28441, #19103, #23200, #5428, #4261, #14376, #6537, #14839, #7835, #11181, #17598, #13160, #25193, #19690, #19825, #23488, #26802, #2421, #17947, #4612 ) ) ;
#25948 = CARTESIAN_POINT ( 'NONE',  ( 21.50000000000018474, 1.873492889145067508, -1.873492889145123019 ) ) ;
#25949 = CARTESIAN_POINT ( 'NONE',  ( 0.7669223171414829565, -15.58766199952932396, -7.954545454545463912 ) ) ;
#25950 = DIRECTION ( 'NONE',  ( 5.551115123125785167E-17, -1.000000000000000000, -8.881784197001256268E-16 ) ) ;
#25951 = ORIENTED_EDGE ( 'NONE', *, *, #18288, .F. ) ;
#25952 = DIRECTION ( 'NONE',  ( 0.000000000000000000, 1.000000000000000000, 0.000000000000000000 ) ) ;
#25953 = CARTESIAN_POINT ( 'NONE',  ( 17.10117513459487171, 1.035533905932929599, -2.499999999999964473 ) ) ;
#25954 = ADVANCED_FACE ( 'NONE', ( #13282 ), #23240, .T. ) ;
#25955 = AXIS2_PLACEMENT_3D ( 'NONE', #7711, #28444, #4656 ) ;
#25956 = CARTESIAN_POINT ( 'NONE',  ( -4.999999999999990230, -55.00000000000002132, 8.000000000000007105 ) ) ;
#25957 = VERTEX_POINT ( 'NONE', #29663 ) ;
#25958 =( GEOMETRIC_REPRESENTATION_CONTEXT ( 3 ) GLOBAL_UNCERTAINTY_ASSIGNED_CONTEXT ( ( #17777 ) ) GLOBAL_UNIT_ASSIGNED_CONTEXT ( ( #11908, #14359, #631 ) ) REPRESENTATION_CONTEXT ( 'NONE', 'WORKASPACE' ) );
#25959 = CARTESIAN_POINT ( 'NONE',  ( -6.000000000000000888, 1.067854986875958443E-15, 7.560779664488942560E-35 ) ) ;
#25960 = ORIENTED_EDGE ( 'NONE', *, *, #15046, .F. ) ;
#25961 = VERTEX_POINT ( 'NONE', #8632 ) ;
#25962 = CARTESIAN_POINT ( 'NONE',  ( 5.196152422706629359, -2.999999999999988898, -141.7886751345947971 ) ) ;
#25963 = CARTESIAN_POINT ( 'NONE',  ( 134.7187500000000284, 2.485281374238555774, -6.000000000000005329 ) ) ;
#25964 = EDGE_CURVE ( 'NONE', #22143, #29510, #28790, .T. ) ;
#25965 = EDGE_CURVE ( 'NONE', #12143, #20807, #14494, .T. ) ;
#25966 = VERTEX_POINT ( 'NONE', #2767 ) ;
#25967 = CARTESIAN_POINT ( 'NONE',  ( 5.412658773652739619, 3.124999999999988898, -142.3169872981078186 ) ) ;
#25968 = CARTESIAN_POINT ( 'NONE',  ( 116.0000000000000142, 0.000000000000000000, 0.000000000000000000 ) ) ;
#25969 = EDGE_CURVE ( 'NONE', #7855, #8435, #25973, .T. ) ;
#25970 = DIRECTION ( 'NONE',  ( 1.000000000000000000, -5.551115123125773458E-17, -1.260129944081490338E-35 ) ) ;
#25971 = CARTESIAN_POINT ( 'NONE',  ( 21.46132486540527751, 5.551115123125782702E-14, -2.500000000000002220 ) ) ;
#25972 = CARTESIAN_POINT ( 'NONE',  ( 18.62500000000003197, -1.414213562373034527, -1.414213562373090038 ) ) ;
#25973 = LINE ( 'NONE', #9707, #22572 ) ;
#25974 = DIRECTION ( 'NONE',  ( 7.147005652999508048E-36, -5.642372883946980038E-36, -1.000000000000000000 ) ) ;
#25975 = DIRECTION ( 'NONE',  ( -1.000000000000000000, -1.665334536937731113E-16, 1.526556658859586792E-16 ) ) ;
#25976 = CARTESIAN_POINT ( 'NONE',  ( 139.2976497308104058, 0.000000000000000000, 5.000000000000004441 ) ) ;
#25977 = CARTESIAN_POINT ( 'NONE',  ( 6.000000000000000888, 1.743066579297358182E-13, -99.66367513459479710 ) ) ;
#25978 = CARTESIAN_POINT ( 'NONE',  ( 5.196152422706629359, -2.999999999999988898, -160.7113248654052313 ) ) ;
#25979 = CARTESIAN_POINT ( 'NONE',  ( -19.49999999999998224, -54.99999999999992184, 7.500000000000007105 ) ) ;
#25980 = CARTESIAN_POINT ( 'NONE',  ( 0.000000000000000000, -5.999999999999991118, -69.46132486540523132 ) ) ;
#25981 = CARTESIAN_POINT ( 'NONE',  ( 110.6874999999997868, -1.035533905932689347, -2.499999999999844569 ) ) ;
#25982 = CARTESIAN_POINT ( 'NONE',  ( 6.000000000000103917, -1.607695154586573416, -142.6533121635129646 ) ) ;
#25983 = AXIS2_PLACEMENT_3D ( 'NONE', #8121, #27317, #27167 ) ;
#25984 = CARTESIAN_POINT ( 'NONE',  ( 0.000000000000000000, 5.999999999999977796, -112.7886751345948397 ) ) ;
#25985 = ORIENTED_EDGE ( 'NONE', *, *, #26398, .T. ) ;
#25986 = CARTESIAN_POINT ( 'NONE',  ( 3.464101615137757051, -5.999999999999979572, -106.8363248654052313 ) ) ;
#25987 = CARTESIAN_POINT ( 'NONE',  ( 3.464101615137852974, 5.999999999999884537, -52.91367513459480421 ) ) ;
#25988 =( BOUNDED_CURVE ( )  B_SPLINE_CURVE ( 2, ( #5470, #8397, #17803, #15505, #12898, #14878, #1018, #27121, #6093 ),
 .UNSPECIFIED., .F., .T. ) 
 B_SPLINE_CURVE_WITH_KNOTS ( ( 3, 2, 2, 2, 3 ),
 ( 0.8750000000000000000, 0.8759259259259258856, 0.8777777777777777679, 0.8796296296296296502, 0.8805555555555555358 ),
 .UNSPECIFIED. ) 
 CURVE ( )  GEOMETRIC_REPRESENTATION_ITEM ( )  RATIONAL_B_SPLINE_CURVE ( ( 0.9330127018922194093, 0.9330127018922194093, 1.000000000000000000, 0.8660254037844388186, 1.000000000000000000, 0.8660254037844388186, 1.000000000000000000, 0.9330127018922234061, 0.9330127018922194093 ) ) 
 REPRESENTATION_ITEM ( '' )  );
#25989 = CARTESIAN_POINT ( 'NONE',  ( -5.999999999999963585, -1.487416814333745711E-14, -170.9136751345948255 ) ) ;
#25990 = ORIENTED_EDGE ( 'NONE', *, *, #9598, .F. ) ;
#25991 = CARTESIAN_POINT ( 'NONE',  ( 116.6872167782373708, 1.849990392679501827, 0.7662911109079489913 ) ) ;
#25992 = CARTESIAN_POINT ( 'NONE',  ( 138.8437500000000568, -6.000000000000005329, -2.485281374238556218 ) ) ;
#25993 = ADVANCED_FACE ( 'NONE', ( #12195 ), #2623, .T. ) ;
#25994 = CARTESIAN_POINT ( 'NONE',  ( 135.1875000000000568, 4.242640687119269671, 4.242640687119298093 ) ) ;
#25995 = AXIS2_PLACEMENT_3D ( 'NONE', #23315, #657, #2259 ) ;
#25996 = EDGE_CURVE ( 'NONE', #11247, #14299, #16702, .T. ) ;
#25997 = CARTESIAN_POINT ( 'NONE',  ( 3.175426480543072749, -5.500000000000105693, -128.1249999999999716 ) ) ;
#25998 = ADVANCED_FACE ( 'NONE', ( #9554 ), #12179, .T. ) ;
#25999 = EDGE_LOOP ( 'NONE', ( #14763, #28292, #15216, #11076 ) ) ;
#26000 = ORIENTED_EDGE ( 'NONE', *, *, #6659, .T. ) ;
#26001 = CARTESIAN_POINT ( 'NONE',  ( 6.350852961086080661, -9.614813431917819062E-14, -67.87500000000002842 ) ) ;
#26002 = CARTESIAN_POINT ( 'NONE',  ( 6.000000000000001776, 5.345404176511898156E-15, -179.1636751345948255 ) ) ;
#26003 = CARTESIAN_POINT ( 'NONE',  ( 159.8150495723242557, -12.30910372856451396, -3.593108990249125778 ) ) ;
#26004 = CARTESIAN_POINT ( 'NONE',  ( -5.412658773652684552, -3.125000000000099920, -79.43301270189223828 ) ) ;
#26005 = UNCERTAINTY_MEASURE_WITH_UNIT (LENGTH_MEASURE( 1.000000000000000082E-05 ), #6212, 'distance_accuracy_value', 'NONE');
#26006 = CARTESIAN_POINT ( 'NONE',  ( 154.6011751345948539, 3.889087296526011706, -3.889087296526011706 ) ) ;
#26007 = CARTESIAN_POINT ( 'NONE',  ( 104.2497167782374845, -1.308140751793640533, -1.308140751793640533 ) ) ;
#26008 = DIRECTION ( 'NONE',  ( 0.000000000000000000, 0.000000000000000000, -1.000000000000000000 ) ) ;
#26009 = DIRECTION ( 'NONE',  ( 1.000000000000000000, -0.000000000000000000, -0.000000000000000000 ) ) ;
#26010 = CARTESIAN_POINT ( 'NONE',  ( -6.350852961085760029, -1.281975124255709124E-13, -139.1250000000000000 ) ) ;
#26011 = CARTESIAN_POINT ( 'NONE',  ( 140.3936200311551374, -9.249647488735854850, 7.646135955868133216 ) ) ;
#26012 = CARTESIAN_POINT ( 'NONE',  ( 7.216878364870455975, -6.409875621278545621E-14, -152.3080127018922099 ) ) ;
#26013 = SURFACE_STYLE_USAGE ( .BOTH. , #28310 ) ;
#26014 = AXIS2_PLACEMENT_3D ( 'NONE', #19377, #7524, #7673 ) ;
#26015 = CARTESIAN_POINT ( 'NONE',  ( 0.000000000000000000, 5.499999999999991118, -78.00000000000001421 ) ) ;
#26016 = DIRECTION ( 'NONE',  ( 1.000000000000000000, -0.000000000000000000, -0.000000000000000000 ) ) ;
#26017 = CARTESIAN_POINT ( 'NONE',  ( 6.350852961086080661, -9.614813431917819062E-14, -67.87500000000002842 ) ) ;
#26018 = CARTESIAN_POINT ( 'NONE',  ( 139.6831941873303720, -9.225388190634568275, 7.967326043633793375 ) ) ;
#26019 = CARTESIAN_POINT ( 'NONE',  ( 146.1711002691896226, 4.999999999999989342, 2.071067811865468400 ) ) ;
#26020 = CARTESIAN_POINT ( 'NONE',  ( 108.6011751345945697, -0.8284271247461453269, 2.000000000000332179 ) ) ;
#26021 = CARTESIAN_POINT ( 'NONE',  ( 160.7812500000000284, 2.485281374238585972, 6.000000000000005329 ) ) ;
#26022 = PLANE ( 'NONE',  #20214 ) ;
#26023 = CARTESIAN_POINT ( 'NONE',  ( 16.81250000000007816, 0.8284271247462955401, -2.000000000000091926 ) ) ;
#26024 = DIRECTION ( 'NONE',  ( 0.000000000000000000, 0.000000000000000000, -1.000000000000000000 ) ) ;
#26025 = EDGE_CURVE ( 'NONE', #27786, #20871, #15299, .T. ) ;
#26026 = CARTESIAN_POINT ( 'NONE',  ( 0.000000000000000000, 0.000000000000000000, 0.000000000000000000 ) ) ;
#26027 = CARTESIAN_POINT ( 'NONE',  ( 3.464101615137757051, -5.999999999999979572, -144.9136751345948255 ) ) ;
#26028 = EDGE_LOOP ( 'NONE', ( #16447, #7929, #13373, #3128 ) ) ;
#26029 = CARTESIAN_POINT ( 'NONE',  ( 153.0937500000000284, 6.000000000000005329, 2.485281374238585972 ) ) ;
#26030 = DIRECTION ( 'NONE',  ( -0.000000000000000000, -0.000000000000000000, -1.000000000000000000 ) ) ;
#26031 = CARTESIAN_POINT ( 'NONE',  ( 113.8752832217622313, -1.849990392679523588, 0.000000000000000000 ) ) ;
#26032 = FILL_AREA_STYLE_COLOUR ( '', #30300 ) ;
#26033 = ADVANCED_FACE ( 'NONE', ( #5065 ), #23686, .T. ) ;
#26034 = LINE ( 'NONE', #827, #27056 ) ;
#26035 = CARTESIAN_POINT ( 'NONE',  ( 19.31250000000010303, -0.8284271247459350507, 2.000000000000091926 ) ) ;
#26036 = EDGE_LOOP ( 'NONE', ( #520, #21042, #10920, #28331 ) ) ;
#26037 = CARTESIAN_POINT ( 'NONE',  ( 3.608439182435180470, -6.249999999999997335, -154.6919872981078470 ) ) ;
#26038 = ORIENTED_EDGE ( 'NONE', *, *, #24941, .F. ) ;
#26039 = CARTESIAN_POINT ( 'NONE',  ( 0.000000000000000000, 5.499999999999991118, -91.50000000000002842 ) ) ;
#26040 =( GEOMETRIC_REPRESENTATION_CONTEXT ( 3 ) GLOBAL_UNCERTAINTY_ASSIGNED_CONTEXT ( ( #148 ) ) GLOBAL_UNIT_ASSIGNED_CONTEXT ( ( #22122, #8593, #8271 ) ) REPRESENTATION_CONTEXT ( 'NONE', 'WORKASPACE' ) );
#26041 = CARTESIAN_POINT ( 'NONE',  ( 5.412658773652739619, 3.124999999999988898, -99.68301270189222407 ) ) ;
#26042 = VERTEX_POINT ( 'NONE', #26266 ) ;
#26043 = VECTOR ( 'NONE', #16435, 1000.000000000000000 ) ;
#26044 = AXIS2_PLACEMENT_3D ( 'NONE', #22259, #1349, #26545 ) ;
#26045 = CARTESIAN_POINT ( 'NONE',  ( 155.2351497308104058, 3.535533905932725318, -3.535533905932725318 ) ) ;
#26046 = DIRECTION ( 'NONE',  ( 0.000000000000000000, 0.8570991287109669399, -0.5151515151515151381 ) ) ;
#26047 = CARTESIAN_POINT ( 'NONE',  ( 4.380587382795412488, -10.09118633559234190, -20.89546095134608805 ) ) ;
#26048 = CARTESIAN_POINT ( 'NONE',  ( -3.464101615137725076, 5.999999999999979572, -93.16367513459479710 ) ) ;
#26049 =( NAMED_UNIT ( * ) PLANE_ANGLE_UNIT ( ) SI_UNIT ( $, .RADIAN. ) );
#26050 = CARTESIAN_POINT ( 'NONE',  ( -3.175426480542816066, 5.499999999999865885, -175.3750000000000568 ) ) ;
#26051 = CARTESIAN_POINT ( 'NONE',  ( -5.999999999999963585, 1.780251999655701777E-13, -57.83632486540521711 ) ) ;
#26052 = CARTESIAN_POINT ( 'NONE',  ( 4.763139720814407951, -2.749999999999988454, -156.5000000000000284 ) ) ;
#26053 = CARTESIAN_POINT ( 'NONE',  ( 112.6249999999998437, -1.767766952966431937, -1.767766952966320915 ) ) ;
#26054 = CARTESIAN_POINT ( 'NONE',  ( 3.175426480543072749, 5.499999999999865885, -102.1250000000000142 ) ) ;
#26055 = FACE_OUTER_BOUND ( 'NONE', #11698, .T. ) ;
#26056 = CARTESIAN_POINT ( 'NONE',  ( -3.175426480542816510, -5.500000000000057732, -86.37500000000005684 ) ) ;
#26057 = CARTESIAN_POINT ( 'NONE',  ( 155.5461002691896510, -2.071067811865468400, 4.999999999999989342 ) ) ;
#26058 = CARTESIAN_POINT ( 'NONE',  ( 107.2261751345946550, 2.000000000000031530, -0.8284271247458748766 ) ) ;
#26059 = ORIENTED_EDGE ( 'NONE', *, *, #25544, .F. ) ;
#26060 = CARTESIAN_POINT ( 'NONE',  ( 9.312500000000124345, -1.097466725451499370, -2.649519052838358757 ) ) ;
#26061 = CARTESIAN_POINT ( 'NONE',  ( 112.9374999999997868, 2.500000000000114575, -1.035533905932448873 ) ) ;
#26062 = AXIS2_PLACEMENT_3D ( 'NONE', #25831, #18491, #18343 ) ;
#26063 = EDGE_CURVE ( 'NONE', #13036, #17687, #14631, .T. ) ;
#26064 = CARTESIAN_POINT ( 'NONE',  ( 105.1877832217621176, 0.7662911109078588412, -1.849990392679291551 ) ) ;
#26065 = EDGE_CURVE ( 'NONE', #14802, #11050, #18633, .T. ) ;
#26066 = ORIENTED_EDGE ( 'NONE', *, *, #24672, .T. ) ;
#26067 = DIRECTION ( 'NONE',  ( 1.000000000000000000, -5.551115123125773458E-17, -1.260129944081490338E-35 ) ) ;
#26068 = CARTESIAN_POINT ( 'NONE',  ( -0.06536716197634070968, -14.68492711179653121, -8.235952467655341280 ) ) ;
#26069 = VECTOR ( 'NONE', #4896, 1000.000000000000000 ) ;
#26070 = CARTESIAN_POINT ( 'NONE',  ( 107.3747167782375840, -5.551115123125782702E-14, -1.849990392679523588 ) ) ;
#26071 = ORIENTED_EDGE ( 'NONE', *, *, #26369, .T. ) ;
#26072 =( BOUNDED_CURVE ( )  B_SPLINE_CURVE ( 2, ( #26793, #24662, #17633, #20068, #29256, #3449, #19613, #5457, #17793 ),
 .UNSPECIFIED., .F., .T. ) 
 B_SPLINE_CURVE_WITH_KNOTS ( ( 3, 2, 2, 2, 3 ),
 ( 0.2941176470588234837, 0.3014705882352941568, 0.3088235294117647189, 0.3161764705882352811, 0.3235294117647058432 ),
 .UNSPECIFIED. ) 
 CURVE ( )  GEOMETRIC_REPRESENTATION_ITEM ( )  RATIONAL_B_SPLINE_CURVE ( ( 1.000000000000000000, 0.9238795325112867385, 1.000000000000000000, 0.9238795325112867385, 1.000000000000000000, 0.9238795325112867385, 1.000000000000000000, 0.9238795325112867385, 1.000000000000000000 ) ) 
 REPRESENTATION_ITEM ( '' )  );
#26073 = ORIENTED_EDGE ( 'NONE', *, *, #5508, .T. ) ;
#26074 = EDGE_LOOP ( 'NONE', ( #18936, #24462, #3764, #26112 ) ) ;
#26075 = CARTESIAN_POINT ( 'NONE',  ( 3.175426480543072749, -5.500000000000105693, -113.1250000000000000 ) ) ;
#26076 = CARTESIAN_POINT ( 'NONE',  ( 17.56250000000009592, 1.097466725451619718, 2.649519052838298805 ) ) ;
#26077 = CARTESIAN_POINT ( 'NONE',  ( 5.412658773652712085, -3.125000000000086153, -120.9330127018922667 ) ) ;
#26078 = ORIENTED_EDGE ( 'NONE', *, *, #11223, .T. ) ;
#26079 = FACE_OUTER_BOUND ( 'NONE', #26366, .T. ) ;
#26080 = CARTESIAN_POINT ( 'NONE',  ( 2.775557561562891351E-14, -6.250000000000061284, -159.3169872981078470 ) ) ;
#26081 = CARTESIAN_POINT ( 'NONE',  ( 107.8124999999997442, 1.035533905932809473, -2.499999999999784173 ) ) ;
#26082 = AXIS2_PLACEMENT_3D ( 'NONE', #707, #12569, #19746 ) ;
#26083 = CARTESIAN_POINT ( 'NONE',  ( -8.673617379884035472E-16, -9.500000000000008882, 4.414213562373099364 ) ) ;
#26084 = AXIS2_PLACEMENT_3D ( 'NONE', #26229, #5181, #2883 ) ;
#26085 = EDGE_LOOP ( 'NONE', ( #22192, #14471, #6582, #31 ) ) ;
#26086 = CARTESIAN_POINT ( 'NONE',  ( -3.027755249632137158, 10.58056329815972241, -19.80527582512399931 ) ) ;
#26087 = CARTESIAN_POINT ( 'NONE',  ( -5.999999999999963585, -1.487416814333745711E-14, -137.3363248654052313 ) ) ;
#26088 = CARTESIAN_POINT ( 'NONE',  ( -3.175426480542816510, -5.500000000000057732, -180.8750000000000000 ) ) ;
#26089 = CARTESIAN_POINT ( 'NONE',  ( 107.5627832217621744, 0.7662911109077987781, 1.849990392679772278 ) ) ;
#26090 = CARTESIAN_POINT ( 'NONE',  ( 152.3363248654052029, 0.000000000000000000, -5.500000000000005329 ) ) ;
#26091 = CARTESIAN_POINT ( 'NONE',  ( 5.412658773652739619, 3.124999999999988898, -177.6830127018922383 ) ) ;
#26092 = CARTESIAN_POINT ( 'NONE',  ( -3.464101615137725076, 5.999999999999979572, -76.08632486540520290 ) ) ;
#26093 = FACE_OUTER_BOUND ( 'NONE', #24623, .T. ) ;
#26094 = CARTESIAN_POINT ( 'NONE',  ( -4.763139720814407951, -2.750000000000016431, -125.5000000000000568 ) ) ;
#26095 = CARTESIAN_POINT ( 'NONE',  ( 6.000000000000000888, 1.607695154586715303, -159.5966878364870922 ) ) ;
#26096 = CARTESIAN_POINT ( 'NONE',  ( 0.000000000000000000, 5.499999999999991118, -112.5000000000000426 ) ) ;
#26097 = ORIENTED_EDGE ( 'NONE', *, *, #24781, .T. ) ;
#26098 = CARTESIAN_POINT ( 'NONE',  ( 16.81250000000011013, 1.097466725451619718, 2.649519052838358757 ) ) ;
#26099 = LINE ( 'NONE', #7368, #25591 ) ;
#26100 = CARTESIAN_POINT ( 'NONE',  ( 6.000000000000000888, -1.859271017917181981E-14, -136.5863248654051745 ) ) ;
#26101 = CYLINDRICAL_SURFACE ( 'NONE', #5954, 6.000000000000000888 ) ;
#26102 = EDGE_CURVE ( 'NONE', #18315, #21672, #8824, .T. ) ;
#26103 = ORIENTED_EDGE ( 'NONE', *, *, #29167, .F. ) ;
#26104 = CARTESIAN_POINT ( 'NONE',  ( 6.000000000000000888, -1.607695154586752384, -126.1533121635130072 ) ) ;
#26105 = CARTESIAN_POINT ( 'NONE',  ( -4.763139720814407951, 2.749999999999946709, -176.7500000000000284 ) ) ;
#26106 = ORIENTED_EDGE ( 'NONE', *, *, #362, .F. ) ;
#26107 = CARTESIAN_POINT ( 'NONE',  ( 22.22617513459494987, 2.500000000000084821, -1.035533905932869425 ) ) ;
#26108 = ORIENTED_EDGE ( 'NONE', *, *, #18120, .F. ) ;
#26109 = ORIENTED_EDGE ( 'NONE', *, *, #12576, .F. ) ;
#26110 = CARTESIAN_POINT ( 'NONE',  ( 20.78867513459484329, -2.499999999999891198, -2.220446049250313081E-13 ) ) ;
#26111 = CARTESIAN_POINT ( 'NONE',  ( 134.4375000000000568, -4.242640687119298093, -4.242640687119298093 ) ) ;
#26112 = ORIENTED_EDGE ( 'NONE', *, *, #2216, .F. ) ;
#26113 = CARTESIAN_POINT ( 'NONE',  ( -7.216878364870328078, 0.000000000000000000, -137.1919872981078186 ) ) ;
#26114 = CARTESIAN_POINT ( 'NONE',  ( -6.000000000000000888, 1.067854986875958443E-15, 7.560779664488942560E-35 ) ) ;
#26115 = CARTESIAN_POINT ( 'NONE',  ( 12.12500000000007994, 1.110223024625156540E-13, -2.649519052838444910 ) ) ;
#26116 = CARTESIAN_POINT ( 'NONE',  ( 19.46132486540541606, 1.665334536937734811E-13, -2.500000000000002220 ) ) ;
#26117 = VERTEX_POINT ( 'NONE', #10155 ) ;
#26118 = CARTESIAN_POINT ( 'NONE',  ( 17.43750000000012790, -1.999999999999851674, 0.8284271247463557142 ) ) ;
#26119 = CARTESIAN_POINT ( 'NONE',  ( 0.000000000000000000, 0.000000000000000000, 0.000000000000000000 ) ) ;
#26120 = CARTESIAN_POINT ( 'NONE',  ( -5.999999999999963585, -1.487416814333745711E-14, -92.33632486540518869 ) ) ;
#26121 = CARTESIAN_POINT ( 'NONE',  ( -0.7071067811865487940, -9.585786437626913070, 4.000000000000004441 ) ) ;
#26122 = CARTESIAN_POINT ( 'NONE',  ( 136.4851497308104058, -3.535533905932725318, 3.535533905932725318 ) ) ;
#26123 = CARTESIAN_POINT ( 'NONE',  ( 116.2261751345945129, 2.000000000000031530, -0.8284271247459350507 ) ) ;
#26124 = LINE ( 'NONE', #625, #16316 ) ;
#26125 = FILL_AREA_STYLE ('',( #9245 ) ) ;
#26126 = EDGE_CURVE ( 'NONE', #16271, #29296, #15108, .T. ) ;
#26127 = CARTESIAN_POINT ( 'NONE',  ( 24.59383218691901263, -1.521799583385193166, 1.870049939131334549 ) ) ;
#26128 = CARTESIAN_POINT ( 'NONE',  ( 106.8749999999998437, 1.767766952966320915, -1.767766952966320915 ) ) ;
#26129 = DIRECTION ( 'NONE',  ( -0.000000000000000000, -0.000000000000000000, -1.000000000000000000 ) ) ;
#26130 = ORIENTED_EDGE ( 'NONE', *, *, #12067, .T. ) ;
#26131 = CARTESIAN_POINT ( 'NONE',  ( 6.000000000000000888, 1.743066579297358182E-13, -106.5863248654052313 ) ) ;
#26132 = CARTESIAN_POINT ( 'NONE',  ( -5.999999999999963585, 1.780251999655701777E-13, -52.41367513459481842 ) ) ;
#26133 = DIRECTION ( 'NONE',  ( 8.326672684688674053E-17, 2.081668171172168513E-17, -1.000000000000000000 ) ) ;
#26134 = EDGE_CURVE ( 'NONE', #6918, #4026, #27934, .T. ) ;
#26135 = EDGE_LOOP ( 'NONE', ( #20874, #22736, #10595, #5014 ) ) ;
#26136 = CARTESIAN_POINT ( 'NONE',  ( 116.3122167782374845, -0.7662911109077388261, -1.849990392679351725 ) ) ;
#26137 = LINE ( 'NONE', #5234, #21328 ) ;
#26138 = CARTESIAN_POINT ( 'NONE',  ( -7.216878364870328078, 0.000000000000000000, -101.1919872981078328 ) ) ;
#26139 = CARTESIAN_POINT ( 'NONE',  ( -3.464101615137725076, 5.999999999999979572, -172.6636751345947687 ) ) ;
#26140 = CARTESIAN_POINT ( 'NONE',  ( 134.7187500000000284, 2.485281374238555774, -6.000000000000005329 ) ) ;
#26141 = CARTESIAN_POINT ( 'NONE',  ( 118.2499999999997584, -8.326672684688674053E-14, 2.500000000000057732 ) ) ;
#26142 = CARTESIAN_POINT ( 'NONE',  ( -4.763139720814407951, -2.750000000000016431, -133.0000000000000000 ) ) ;
#26143 = STYLED_ITEM ( 'NONE', ( #11903 ), #22780 ) ;
#26144 = VERTEX_POINT ( 'NONE', #24257 ) ;
#26145 = CARTESIAN_POINT ( 'NONE',  ( -4.763139720814407951, -2.750000000000016431, -55.00000000000004974 ) ) ;
#26146 = CARTESIAN_POINT ( 'NONE',  ( 6.000000000000000888, 1.743066579297358182E-13, -81.08632486540518869 ) ) ;
#26147 = DIRECTION ( 'NONE',  ( 1.000000000000000000, -0.000000000000000000, -0.000000000000000000 ) ) ;
#26148 =( BOUNDED_CURVE ( )  B_SPLINE_CURVE ( 2, ( #9645, #28355, #16738, #3443, #1305, #20227, #29250, #8532, #1460 ),
 .UNSPECIFIED., .F., .T. ) 
 B_SPLINE_CURVE_WITH_KNOTS ( ( 3, 2, 2, 2, 3 ),
 ( 0.5000000000000000000, 0.5073529411764705621, 0.5147058823529411242, 0.5220588235294117974, 0.5294117647058823595 ),
 .UNSPECIFIED. ) 
 CURVE ( )  GEOMETRIC_REPRESENTATION_ITEM ( )  RATIONAL_B_SPLINE_CURVE ( ( 1.000000000000000000, 0.9238795325112867385, 1.000000000000000000, 0.9238795325112867385, 1.000000000000000000, 0.9238795325112867385, 1.000000000000000000, 0.9238795325112867385, 1.000000000000000000 ) ) 
 REPRESENTATION_ITEM ( '' )  );
#26149 = CARTESIAN_POINT ( 'NONE',  ( 5.412658773652712085, -3.125000000000086153, -83.43301270189223828 ) ) ;
#26150 = DIRECTION ( 'NONE',  ( 1.000000000000000000, -5.551115123125773458E-17, -1.260129944081490338E-35 ) ) ;
#26151 = ADVANCED_FACE ( 'NONE', ( #8119 ), #19381, .T. ) ;
#26152 = CARTESIAN_POINT ( 'NONE',  ( 105.8122167782375129, 0.7662911109077987781, 1.849990392679652151 ) ) ;
#26153 = CARTESIAN_POINT ( 'NONE',  ( 140.5000000000000284, -10.99818166789401275, 4.799999999999998934 ) ) ;
#26154 = CARTESIAN_POINT ( 'NONE',  ( 115.5627832217620892, 0.7662911109077987781, 1.849990392679772278 ) ) ;
#26155 =( BOUNDED_CURVE ( )  B_SPLINE_CURVE ( 2, ( #26552, #453, #19520, #12327, #3055, #19219, #26404, #21673, #28694 ),
 .UNSPECIFIED., .F., .T. ) 
 B_SPLINE_CURVE_WITH_KNOTS ( ( 3, 2, 2, 2, 3 ),
 ( 0.2861111111111112049, 0.2870370370370370905, 0.2888888888888888618, 0.2907407407407407440, 0.2916666666666666297 ),
 .UNSPECIFIED. ) 
 CURVE ( )  GEOMETRIC_REPRESENTATION_ITEM ( )  RATIONAL_B_SPLINE_CURVE ( ( 0.9330127018922194093, 0.9330127018922234061, 1.000000000000000000, 0.8660254037844388186, 1.000000000000000000, 0.8660254037844388186, 1.000000000000000000, 0.9330127018922234061, 0.9330127018922194093 ) ) 
 REPRESENTATION_ITEM ( '' )  );
#26156 = CARTESIAN_POINT ( 'NONE',  ( -4.763139720814407951, 2.749999999999946709, -142.2500000000000000 ) ) ;
#26157 = CARTESIAN_POINT ( 'NONE',  ( -5.412658773652684552, -3.125000000000099920, -151.4330127018922383 ) ) ;
#26158 = CARTESIAN_POINT ( 'NONE',  ( -4.999999999999920952, -65.50000000000001421, 8.000000000000007105 ) ) ;
#26159 = CARTESIAN_POINT ( 'NONE',  ( -3.175426480542816066, 5.499999999999865885, -73.37500000000000000 ) ) ;
#26160 = CARTESIAN_POINT ( 'NONE',  ( 145.4925748654052029, 2.278174593052012309, 5.500000000000012434 ) ) ;
#26161 = EDGE_CURVE ( 'NONE', #4004, #1664, #30409, .T. ) ;
#26162 = CARTESIAN_POINT ( 'NONE',  ( 3.175426480543072749, 5.499999999999865885, -69.12500000000002842 ) ) ;
#26163 = ADVANCED_FACE ( 'NONE', ( #19964 ), #1723, .T. ) ;
#26164 = CARTESIAN_POINT ( 'NONE',  ( 6.000000000000000888, 1.607695154586715303, -54.01933756729742697 ) ) ;
#26165 = CARTESIAN_POINT ( 'NONE',  ( 144.9523502691896510, 0.000000000000000000, 5.000000000000004441 ) ) ;
#26166 = CARTESIAN_POINT ( 'NONE',  ( 104.9349859426397273, -1.403591609995181955, -1.388700252127261336 ) ) ;
#26167 = PRESENTATION_LAYER_ASSIGNMENT (  '', '', ( #6546 ) ) ;
#26168 = CARTESIAN_POINT ( 'NONE',  ( 152.9062500000000568, 6.000000000000005329, -2.485281374238556218 ) ) ;
#26169 = CARTESIAN_POINT ( 'NONE',  ( 5.196152422706629359, 3.000000000000002665, -127.4613248654052313 ) ) ;
#26170 = LINE ( 'NONE', #11646, #7220 ) ;
#26171 = CARTESIAN_POINT ( 'NONE',  ( 114.1872167782375413, -1.849990392679411677, -0.7662911109076485650 ) ) ;
#26172 = CARTESIAN_POINT ( 'NONE',  ( 6.000000000000026645, -1.607695154586707753, -144.7306624327026157 ) ) ;
#26173 = VERTEX_POINT ( 'NONE', #24118 ) ;
#26174 = CARTESIAN_POINT ( 'NONE',  ( 152.2500000000000284, -6.000000000000005329, 0.000000000000000000 ) ) ;
#26175 = CARTESIAN_POINT ( 'NONE',  ( 112.7502832217623734, -1.308140751793640533, 1.308140751793640533 ) ) ;
#26176 =( LENGTH_UNIT ( ) NAMED_UNIT ( * ) SI_UNIT ( .MILLI., .METRE. ) );
#26177 = CARTESIAN_POINT ( 'NONE',  ( 6.000000000000000000, 2.951592740943527306E-14, -154.5863248654052029 ) ) ;
#26178 = CARTESIAN_POINT ( 'NONE',  ( 22.68750000000017764, -0.8284271247460553989, -2.000000000000031530 ) ) ;
#26179 = ORIENTED_EDGE ( 'NONE', *, *, #1620, .T. ) ;
#26180 = CARTESIAN_POINT ( 'NONE',  ( -3.608439182435052128, -6.250000000000110134, -153.4419872981078470 ) ) ;
#26181 = ORIENTED_EDGE ( 'NONE', *, *, #13913, .T. ) ;
#26182 = CARTESIAN_POINT ( 'NONE',  ( -2.775557561562891351E-14, -5.500000000000115463, -83.25000000000004263 ) ) ;
#26183 = CARTESIAN_POINT ( 'NONE',  ( 5.412658773652712085, -3.125000000000086153, -99.93301270189225249 ) ) ;
#26184 = EDGE_LOOP ( 'NONE', ( #10755, #24000, #16600, #17266, #17645 ) ) ;
#26185 = CARTESIAN_POINT ( 'NONE',  ( 0.000000000000000000, 5.999999999999977796, -147.2886751345948824 ) ) ;
#26186 = EDGE_CURVE ( 'NONE', #22716, #6411, #12490, .T. ) ;
#26187 = CARTESIAN_POINT ( 'NONE',  ( 129.9999999999998010, -90.00000000000001421, 4.000000000000003553 ) ) ;
#26188 = CARTESIAN_POINT ( 'NONE',  ( 6.000000000000000888, -1.859271017917181981E-14, -59.16367513459483263 ) ) ;
#26189 =( NAMED_UNIT ( * ) SI_UNIT ( $, .STERADIAN. ) SOLID_ANGLE_UNIT ( ) );
#26190 = CARTESIAN_POINT ( 'NONE',  ( 140.0000000000000284, -11.48520880827722124, 4.868161254798543780 ) ) ;
#26191 = CARTESIAN_POINT ( 'NONE',  ( 3.175426480543072749, 5.499999999999865885, -160.6250000000000284 ) ) ;
#26192 = CARTESIAN_POINT ( 'NONE',  ( -5.999999999999963585, 1.780251999655701777E-13, -60.83632486540522422 ) ) ;
#26193 = CARTESIAN_POINT ( 'NONE',  ( -2.775557561562891351E-14, -5.500000000000115463, -152.2500000000000000 ) ) ;
#26194 = CARTESIAN_POINT ( 'NONE',  ( 114.1874999999998295, 1.035533905932779275, 2.500000000000445421 ) ) ;
#26195 = CARTESIAN_POINT ( 'NONE',  ( -6.350852961085760029, -1.281975124255709124E-13, -92.62500000000001421 ) ) ;
#26196 = CARTESIAN_POINT ( 'NONE',  ( 24.28867513459498184, 2.500000000000057732, -2.220446049250313081E-13 ) ) ;
#26197 = EDGE_CURVE ( 'NONE', #4156, #234, #23062, .T. ) ;
#26198 = CARTESIAN_POINT ( 'NONE',  ( -6.350852961085760029, -1.281975124255709124E-13, -92.62500000000001421 ) ) ;
#26199 = CARTESIAN_POINT ( 'NONE',  ( 13.46132486540532724, 1.665334536937734811E-13, -2.500000000000057732 ) ) ;
#26200 = CARTESIAN_POINT ( 'NONE',  ( 156.4836002691896795, 4.999999999999989342, -2.071067811865468400 ) ) ;
#26201 = CYLINDRICAL_SURFACE ( 'NONE', #3233, 6.000000000000000888 ) ;
#26202 = CARTESIAN_POINT ( 'NONE',  ( 24.31250000000015632, -0.8284271247461152399, 2.000000000000031530 ) ) ;
#26203 = CARTESIAN_POINT ( 'NONE',  ( 113.8749999999998721, 1.767766952966431937, -1.767766952966209892 ) ) ;
#26204 = CARTESIAN_POINT ( 'NONE',  ( 107.7113248654050892, 2.000000000000057288, 0.000000000000000000 ) ) ;
#26205 = CARTESIAN_POINT ( 'NONE',  ( 112.7113248654049897, 2.000000000000057288, 0.000000000000000000 ) ) ;
#26206 = VERTEX_POINT ( 'NONE', #29781 ) ;
#26207 = DIRECTION ( 'NONE',  ( 0.000000000000000000, 0.9730085108210397848, -0.2307692307692307265 ) ) ;
#26208 = CARTESIAN_POINT ( 'NONE',  ( 0.000000000000000000, 0.000000000000000000, 0.000000000000000000 ) ) ;
#26209 = CARTESIAN_POINT ( 'NONE',  ( 119.7502832217622455, -1.308140751793501755, 1.308140751793751555 ) ) ;
#26210 = ORIENTED_EDGE ( 'NONE', *, *, #28278, .T. ) ;
#26211 = CARTESIAN_POINT ( 'NONE',  ( 145.5937500000000284, 6.000000000000005329, 2.485281374238585972 ) ) ;
#26212 = CARTESIAN_POINT ( 'NONE',  ( 4.763139720814407951, 2.750000000000002665, -114.2500000000000142 ) ) ;
#26213 = CARTESIAN_POINT ( 'NONE',  ( 19.56250000000012790, 1.097466725451739622, 2.649519052838298805 ) ) ;
#26214 = CARTESIAN_POINT ( 'NONE',  ( 3.608439182435180470, -6.249999999999997335, -127.0580127018922525 ) ) ;
#26215 = UNCERTAINTY_MEASURE_WITH_UNIT (LENGTH_MEASURE( 1.000000000000000082E-05 ), #8737, 'distance_accuracy_value', 'NONE');
#26216 = ORIENTED_EDGE ( 'NONE', *, *, #29723, .T. ) ;
#26217 = CARTESIAN_POINT ( 'NONE',  ( -5.196152422706573404, -3.000000000000002665, -61.28867513459484684 ) ) ;
#26218 = CARTESIAN_POINT ( 'NONE',  ( 3.608439182435180470, -6.249999999999997335, -159.1919872981078470 ) ) ;
#26219 = CARTESIAN_POINT ( 'NONE',  ( 108.9374999999997442, 2.500000000000114575, -1.035533905932508825 ) ) ;
#26220 = CARTESIAN_POINT ( 'NONE',  ( 132.2663997308104342, -4.999999999999989342, -2.071067811865468400 ) ) ;
#26221 = TOROIDAL_SURFACE ( 'NONE', #20858, 14.49999999999999822, 0.5000000000000000000 ) ;
#26222 = ADVANCED_FACE ( 'NONE', ( #13547 ), #547, .T. ) ;
#26223 = CARTESIAN_POINT ( 'NONE',  ( -3.608439182435115633, 6.249999999999965361, -61.80801270189223828 ) ) ;
#26224 = ORIENTED_EDGE ( 'NONE', *, *, #10188, .F. ) ;
#26225 = CARTESIAN_POINT ( 'NONE',  ( 0.8492607147730748540, -15.39618690451816008, -8.319180134514111202 ) ) ;
#26226 = EDGE_CURVE ( 'NONE', #12504, #11496, #15489, .T. ) ;
#26227 = PRODUCT_RELATED_PRODUCT_CATEGORY ( 'part', '', ( #30020 ) ) ;
#26228 = CARTESIAN_POINT ( 'NONE',  ( -6.000249633052390230, 9.219381998443786586, -24.80704692217342355 ) ) ;
#26229 = CARTESIAN_POINT ( 'NONE',  ( -19.99999999999998224, -54.99999999999990763, 8.000000000000007105 ) ) ;
#26230 = CARTESIAN_POINT ( 'NONE',  ( -3.175426480542816510, -5.500000000000057732, -176.3750000000000284 ) ) ;
#26231 = CARTESIAN_POINT ( 'NONE',  ( 106.5627832217621602, 0.7662911109078588412, 1.849990392679712103 ) ) ;
#26232 = DIRECTION ( 'NONE',  ( -8.326672684688675286E-17, -2.081668171172168821E-17, 1.000000000000000000 ) ) ;
#26233 = CARTESIAN_POINT ( 'NONE',  ( 5.412658773652712085, -3.125000000000086153, -176.4330127018922667 ) ) ;
#26234 = CARTESIAN_POINT ( 'NONE',  ( 113.5386751345947687, 5.551115123125782702E-14, 2.000000000000001776 ) ) ;
#26235 = DIRECTION ( 'NONE',  ( -1.000000000000000000, 0.000000000000000000, 0.000000000000000000 ) ) ;
#26236 = CARTESIAN_POINT ( 'NONE',  ( 4.763139720814407951, -2.749999999999988454, -123.5000000000000568 ) ) ;
#26237 = CARTESIAN_POINT ( 'NONE',  ( 6.000000000000000888, -1.859271017917181981E-14, -84.66367513459482552 ) ) ;
#26238 = CARTESIAN_POINT ( 'NONE',  ( 6.350852961086080661, -9.614813431917819062E-14, -109.8750000000000426 ) ) ;
#26239 = VECTOR ( 'NONE', #18625, 1000.000000000000000 ) ;
#26240 = CARTESIAN_POINT ( 'NONE',  ( 16.21132486540519224, -2.499999999999835687, -1.110223024625156540E-13 ) ) ;
#26241 = ORIENTED_EDGE ( 'NONE', *, *, #30327, .T. ) ;
#26242 = CARTESIAN_POINT ( 'NONE',  ( 18.12500000000011369, -2.649519052838111843, 0.000000000000000000 ) ) ;
#26243 = B_SPLINE_CURVE_WITH_KNOTS ( 'NONE', 3,
 ( #29893, #27573, #6553, #15973, #25271, #13666, #23008, #11356 ),
 .UNSPECIFIED., .F., .F.,
 ( 4, 2, 2, 4 ),
 ( 0.000000000000000000, 0.0008823129044422798641, 0.001323469356663417628, 0.001764625808884555391 ),
 .UNSPECIFIED. ) ;
#26244 = DIRECTION ( 'NONE',  ( 1.000000000000000000, -5.551115123125774690E-17, 0.000000000000000000 ) ) ;
#26245 = CARTESIAN_POINT ( 'NONE',  ( 3.464101615137757051, -5.999999999999979572, -136.8363248654052313 ) ) ;
#26246 =( BOUNDED_CURVE ( )  B_SPLINE_CURVE ( 2, ( #13862, #18754, #20741, #7203, #11860, #1986, #28229, #30091, #16615 ),
 .UNSPECIFIED., .F., .T. ) 
 B_SPLINE_CURVE_WITH_KNOTS ( ( 3, 2, 2, 2, 3 ),
 ( 0.2647058823529411242, 0.2720588235294117974, 0.2794117647058823595, 0.2867647058823529216, 0.2941176470588234837 ),
 .UNSPECIFIED. ) 
 CURVE ( )  GEOMETRIC_REPRESENTATION_ITEM ( )  RATIONAL_B_SPLINE_CURVE ( ( 1.000000000000000000, 0.9238795325112867385, 1.000000000000000000, 0.9238795325112867385, 1.000000000000000000, 0.9238795325112867385, 1.000000000000000000, 0.9238795325112867385, 1.000000000000000000 ) ) 
 REPRESENTATION_ITEM ( '' )  );
#26247 = ORIENTED_EDGE ( 'NONE', *, *, #13988, .T. ) ;
#26248 = MECHANICAL_DESIGN_GEOMETRIC_PRESENTATION_REPRESENTATION (  '', ( #6122 ), #3316 ) ;
#26249 = CARTESIAN_POINT ( 'NONE',  ( 19.99999999999998934, 0.000000000000000000, 0.000000000000000000 ) ) ;
#26250 = CARTESIAN_POINT ( 'NONE',  ( 4.763139720814407951, -2.749999999999988454, -177.5000000000000000 ) ) ;
#26251 = ORIENTED_EDGE ( 'NONE', *, *, #8517, .F. ) ;
#26252 = FACE_OUTER_BOUND ( 'NONE', #5057, .T. ) ;
#26253 = ORIENTED_EDGE ( 'NONE', *, *, #30040, .F. ) ;
#26254 = ORIENTED_EDGE ( 'NONE', *, *, #15154, .F. ) ;
#26255 = CARTESIAN_POINT ( 'NONE',  ( 132.8437500000000284, -6.000000000000005329, -2.485281374238555774 ) ) ;
#26256 = CARTESIAN_POINT ( 'NONE',  ( 132.9523502691896510, 0.000000000000000000, 5.000000000000004441 ) ) ;
#26257 = VERTEX_POINT ( 'NONE', #5623 ) ;
#26258 = CARTESIAN_POINT ( 'NONE',  ( 139.4136751345948539, 0.000000000000000000, -5.500000000000005329 ) ) ;
#26259 = VECTOR ( 'NONE', #1329, 1000.000000000000000 ) ;
#26260 = CARTESIAN_POINT ( 'NONE',  ( 5.412658773652739619, 3.124999999999988898, -131.8169872981078186 ) ) ;
#26261 = CARTESIAN_POINT ( 'NONE',  ( 24.39882486540525974, -1.035533905932568999, -2.499999999999964473 ) ) ;
#26262 = CARTESIAN_POINT ( 'NONE',  ( 12.31250000000017053, 2.649519052838419153, -1.097466725451619718 ) ) ;
#26263 = DIRECTION ( 'NONE',  ( -7.147005652999508048E-36, 5.642372883946980038E-36, 1.000000000000000000 ) ) ;
#26264 = VERTEX_POINT ( 'NONE', #14593 ) ;
#26265 = CARTESIAN_POINT ( 'NONE',  ( 20.87500000000014211, 1.414213562373367594, -1.414213562373145550 ) ) ;
#26266 = CARTESIAN_POINT ( 'NONE',  ( 6.000000000000000888, -1.859271017917181981E-14, -67.58632486540523132 ) ) ;
#26267 = CARTESIAN_POINT ( 'NONE',  ( 149.8199251345948824, -2.278174593051981223, -5.500000000000041744 ) ) ;
#26268 = ADVANCED_FACE ( 'NONE', ( #15184 ), #26808, .T. ) ;
#26269 = CARTESIAN_POINT ( 'NONE',  ( 138.3601497308104058, -3.535533905932725318, -3.535533905932725318 ) ) ;
#26270 = CARTESIAN_POINT ( 'NONE',  ( 152.3363248654052029, 0.000000000000000000, -5.500000000000005329 ) ) ;
#26271 = AXIS2_PLACEMENT_3D ( 'NONE', #25252, #6530, #1928 ) ;
#26272 = LINE ( 'NONE', #5222, #4738 ) ;
#26273 = CARTESIAN_POINT ( 'NONE',  ( 0.000000000000000000, 0.000000000000000000, 0.000000000000000000 ) ) ;
#26274 = CARTESIAN_POINT ( 'NONE',  ( 104.6249999999999005, -1.767766952966376426, -1.767766952966320915 ) ) ;
#26275 = CARTESIAN_POINT ( 'NONE',  ( -3.175426480542816510, 5.499999999999865885, -139.3750000000000568 ) ) ;
#26276 = DIRECTION ( 'NONE',  ( -8.326672684688675286E-17, -2.081668171172168821E-17, 1.000000000000000000 ) ) ;
#26277 = CARTESIAN_POINT ( 'NONE',  ( 104.7401757384973848, 1.791171210506977474, -0.4782956395680261763 ) ) ;
#26278 = VERTEX_POINT ( 'NONE', #5475 ) ;
#26279 = CARTESIAN_POINT ( 'NONE',  ( 107.9136751345947260, -1.414213562373256572, -1.414213562373034527 ) ) ;
#26280 = CARTESIAN_POINT ( 'NONE',  ( 5.196152422706629359, 3.000000000000002665, -53.03867513459481131 ) ) ;
#26281 = CARTESIAN_POINT ( 'NONE',  ( 118.2261751345946408, 2.000000000000091926, -0.8284271247458748766 ) ) ;
#26282 = CARTESIAN_POINT ( 'NONE',  ( 3.464101615137852974, 5.999999999999884537, -152.8363248654051745 ) ) ;
#26283 = ORIENTED_EDGE ( 'NONE', *, *, #6647, .F. ) ;
#26284 = CARTESIAN_POINT ( 'NONE',  ( 118.8122167782374987, 0.7662911109078287542, 1.849990392679712103 ) ) ;
#26285 = CARTESIAN_POINT ( 'NONE',  ( 136.6875000000000284, 4.242640687119269671, 4.242640687119298093 ) ) ;
#26286 = CARTESIAN_POINT ( 'NONE',  ( -5.412658773652739619, 3.124999999999975131, -95.31698729810783277 ) ) ;
#26287 = CARTESIAN_POINT ( 'NONE',  ( 6.000000000000000888, 1.743066579297358182E-13, -50.16367513459482552 ) ) ;
#26288 =( NAMED_UNIT ( * ) SI_UNIT ( $, .STERADIAN. ) SOLID_ANGLE_UNIT ( ) );
#26289 = DIRECTION ( 'NONE',  ( -0.000000000000000000, -0.000000000000000000, -1.000000000000000000 ) ) ;
#26290 = VECTOR ( 'NONE', #30102, 1000.000000000000000 ) ;
#26291 = ADVANCED_FACE ( 'NONE', ( #3172 ), #15211, .T. ) ;
#26292 = CARTESIAN_POINT ( 'NONE',  ( -3.175426480542816510, -5.500000000000057732, -131.3750000000000000 ) ) ;
#26293 = ORIENTED_EDGE ( 'NONE', *, *, #10984, .T. ) ;
#26294 = CARTESIAN_POINT ( 'NONE',  ( 4.763139720814407951, -2.749999999999988454, -59.00000000000004974 ) ) ;
#26295 = PLANE ( 'NONE',  #20455 ) ;
#26296 = DIRECTION ( 'NONE',  ( -7.147005652999508048E-36, 5.642372883946980038E-36, 1.000000000000000000 ) ) ;
#26297 = CARTESIAN_POINT ( 'NONE',  ( 5.197786390520589883, 9.697480688945329774, -28.02189831943640996 ) ) ;
#26298 = CARTESIAN_POINT ( 'NONE',  ( 7.216878364870455975, -6.409875621278545621E-14, -84.80801270189222407 ) ) ;
#26299 = EDGE_CURVE ( 'NONE', #17999, #27945, #29120, .T. ) ;
#26300 = DIRECTION ( 'NONE',  ( 1.000000000000000000, 6.938893903907221278E-15, 0.000000000000000000 ) ) ;
#26301 = FACE_OUTER_BOUND ( 'NONE', #7215, .T. ) ;
#26302 = CARTESIAN_POINT ( 'NONE',  ( 1.000000000000000888, 2.143131898507868643E-15, -17.50000000000000355 ) ) ;
#26303 = DIRECTION ( 'NONE',  ( -0.000000000000000000, 1.000000000000000000, -0.000000000000000000 ) ) ;
#26304 = CARTESIAN_POINT ( 'NONE',  ( 116.2502832217621886, 1.308140751793612777, -1.308140751793418488 ) ) ;
#26305 = CARTESIAN_POINT ( 'NONE',  ( 4.763139720814407951, 2.750000000000002665, -136.7500000000000284 ) ) ;
#26306 = CARTESIAN_POINT ( 'NONE',  ( -4.999999999999886313, -10.00000000000000888, 8.000000000000007105 ) ) ;
#26307 = CARTESIAN_POINT ( 'NONE',  ( -7.216878364870328078, 0.000000000000000000, -151.5580127018922099 ) ) ;
#26308 = CARTESIAN_POINT ( 'NONE',  ( 5.196152422706629359, 3.000000000000002665, -158.9613248654052597 ) ) ;
#26309 = CARTESIAN_POINT ( 'NONE',  ( 20.46132486540533435, 1.110223024625156540E-13, -2.500000000000057732 ) ) ;
#26310 = CARTESIAN_POINT ( 'NONE',  ( 4.763139720814407951, -2.749999999999988454, -68.00000000000000000 ) ) ;
#26311 = CARTESIAN_POINT ( 'NONE',  ( 4.763139720814407951, 2.750000000000002665, -63.25000000000002842 ) ) ;
#26312 = SURFACE_STYLE_USAGE ( .BOTH. , #22176 ) ;
#26313 = CARTESIAN_POINT ( 'NONE',  ( 154.0312500000000284, -2.485281374238556218, -6.000000000000005329 ) ) ;
#26314 = CARTESIAN_POINT ( 'NONE',  ( 135.0000000000000000, -8.132390304760285460, -7.784889480266582673 ) ) ;
#26315 = CARTESIAN_POINT ( 'NONE',  ( -3.464101615137757051, -5.999999999999979572, -104.6636751345948539 ) ) ;
#26316 = CARTESIAN_POINT ( 'NONE',  ( 115.3122167782374845, -0.7662911109077388261, -1.849990392679291551 ) ) ;
#26317 = CARTESIAN_POINT ( 'NONE',  ( 5.196152422706629359, -2.999999999999988898, -144.7886751345948255 ) ) ;
#26318 = ORIENTED_EDGE ( 'NONE', *, *, #24312, .F. ) ;
#26319 = CARTESIAN_POINT ( 'NONE',  ( 148.2187500000000568, 2.485281374238555774, -6.000000000000005329 ) ) ;
#26320 = EDGE_CURVE ( 'NONE', #3131, #8715, #21790, .T. ) ;
#26321 = UNCERTAINTY_MEASURE_WITH_UNIT (LENGTH_MEASURE( 1.000000000000000082E-05 ), #12459, 'distance_accuracy_value', 'NONE');
#26322 =( BOUNDED_CURVE ( )  B_SPLINE_CURVE ( 2, ( #27024, #19973, #8129, #15406, #29327, #18011, #8453, #20137, #18153 ),
 .UNSPECIFIED., .F., .T. ) 
 B_SPLINE_CURVE_WITH_KNOTS ( ( 3, 2, 2, 2, 3 ),
 ( 0.5124999999999990674, 0.5187499999999993783, 0.5249999999999995781, 0.5312499999999997780, 0.5374999999999999778 ),
 .UNSPECIFIED. ) 
 CURVE ( )  GEOMETRIC_REPRESENTATION_ITEM ( )  RATIONAL_B_SPLINE_CURVE ( ( 1.000000000000010880, 0.9238795325112759693, 1.000000000000000000, 0.9238795325112867385, 1.000000000000000000, 0.9238795325112867385, 1.000000000000000000, 0.9238795325112867385, 1.000000000000000000 ) ) 
 REPRESENTATION_ITEM ( '' )  );
#26323 = CARTESIAN_POINT ( 'NONE',  ( 0.000000000000000000, -5.999999999999991118, -158.5386751345948539 ) ) ;
#26324 = CARTESIAN_POINT ( 'NONE',  ( -3.175426480542816510, 5.499999999999865885, -179.8750000000000000 ) ) ;
#26325 = CIRCLE ( 'NONE', #16086, 2.000000000000003109 ) ;
#26326 = CARTESIAN_POINT ( 'NONE',  ( 20.43750000000014566, -1.999999999999911626, 0.8284271247462354770 ) ) ;
#26327 = ORIENTED_EDGE ( 'NONE', *, *, #18747, .T. ) ;
#26328 = VERTEX_POINT ( 'NONE', #8233 ) ;
#26329 = CARTESIAN_POINT ( 'NONE',  ( -3.175426480542816510, 5.499999999999865885, -85.37500000000004263 ) ) ;
#26330 = EDGE_CURVE ( 'NONE', #5324, #11924, #24676, .T. ) ;
#26331 = CARTESIAN_POINT ( 'NONE',  ( 2.775557561562891351E-14, 6.250000000000033751, -99.43301270189225249 ) ) ;
#26332 =( BOUNDED_CURVE ( )  B_SPLINE_CURVE ( 2, ( #16340, #4761, #25336, #4311, #13730, #23073, #18470, #6768, #20917 ),
 .UNSPECIFIED., .F., .T. ) 
 B_SPLINE_CURVE_WITH_KNOTS ( ( 3, 2, 2, 2, 3 ),
 ( 0.4531250000000000000, 0.4609375000000000000, 0.4687500000000000000, 0.4765625000000000000, 0.4843750000000000000 ),
 .UNSPECIFIED. ) 
 CURVE ( )  GEOMETRIC_REPRESENTATION_ITEM ( )  RATIONAL_B_SPLINE_CURVE ( ( 1.000000000000000000, 0.9238795325112867385, 1.000000000000000000, 0.9238795325112867385, 1.000000000000000000, 0.9238795325112867385, 1.000000000000000000, 0.9238795325112867385, 1.000000000000000000 ) ) 
 REPRESENTATION_ITEM ( '' )  );
#26333 = EDGE_LOOP ( 'NONE', ( #20688, #15970, #25990, #2868 ) ) ;
#26334 = CARTESIAN_POINT ( 'NONE',  ( 119.9999999999998579, 1.988103546247746323, 1.253414257839255752 ) ) ;
#26335 = FILL_AREA_STYLE_COLOUR ( '', #14756 ) ;
#26336 = CYLINDRICAL_SURFACE ( 'NONE', #3770, 2.000000000000012879 ) ;
#26337 = CARTESIAN_POINT ( 'NONE',  ( 119.9999999999998437, 2.000000000000057288, 0.000000000000000000 ) ) ;
#26338 = CARTESIAN_POINT ( 'NONE',  ( 140.5126264503616085, -11.05212133306724276, 4.674908800638664097 ) ) ;
#26339 = VECTOR ( 'NONE', #8820, 1000.000000000000000 ) ;
#26340 = SURFACE_STYLE_USAGE ( .BOTH. , #24641 ) ;
#26341 = CARTESIAN_POINT ( 'NONE',  ( -4.763139720814407951, 2.749999999999946709, -161.7500000000000568 ) ) ;
#26342 = LINE ( 'NONE', #7901, #28228 ) ;
#26343 = CARTESIAN_POINT ( 'NONE',  ( -2.775557561562891351E-14, -5.500000000000115463, -158.2500000000000000 ) ) ;
#26344 = CARTESIAN_POINT ( 'NONE',  ( 117.1636751345947545, 1.414213562373201061, -1.414213562373145550 ) ) ;
#26345 = CARTESIAN_POINT ( 'NONE',  ( -2.775557561562891351E-14, -5.500000000000115463, -90.75000000000000000 ) ) ;
#26346 = FACE_OUTER_BOUND ( 'NONE', #18780, .T. ) ;
#26347 = LINE ( 'NONE', #23479, #4941 ) ;
#26348 = CARTESIAN_POINT ( 'NONE',  ( 3.175426480543072749, -5.500000000000105693, -92.12500000000001421 ) ) ;
#26349 = CARTESIAN_POINT ( 'NONE',  ( 157.1398502691896510, -3.535533905932752852, 3.535533905932725318 ) ) ;
#26350 = CARTESIAN_POINT ( 'NONE',  ( 6.000000000000000888, 1.743066579297358182E-13, -65.16367513459479710 ) ) ;
#26351 = CARTESIAN_POINT ( 'NONE',  ( 22.93749999999995737, 1.999999999999971800, -0.8284271247462354770 ) ) ;
#26352 = CARTESIAN_POINT ( 'NONE',  ( 110.5624999999998295, -2.499999999999994671, -1.035533905932568777 ) ) ;
#26353 = CARTESIAN_POINT ( 'NONE',  ( -1.000000000000000888, 9.000000000000007105, -3.000000000000002665 ) ) ;
#26354 =( NAMED_UNIT ( * ) SI_UNIT ( $, .STERADIAN. ) SOLID_ANGLE_UNIT ( ) );
#26355 = DIRECTION ( 'NONE',  ( -7.147005652999508048E-36, 5.642372883946980038E-36, 1.000000000000000000 ) ) ;
#26356 = ORIENTED_EDGE ( 'NONE', *, *, #30191, .F. ) ;
#26357 = CARTESIAN_POINT ( 'NONE',  ( 135.0000000000000284, -8.798545334315205579, 8.160000000000000142 ) ) ;
#26358 = FACE_OUTER_BOUND ( 'NONE', #7039, .T. ) ;
#26359 = VECTOR ( 'NONE', #21291, 1000.000000000000000 ) ;
#26360 = CARTESIAN_POINT ( 'NONE',  ( 105.0622167782375840, -1.849990392679501827, 0.7662911109077686911 ) ) ;
#26361 = ADVANCED_FACE ( 'NONE', ( #12302 ), #19345, .T. ) ;
#26362 = ORIENTED_EDGE ( 'NONE', *, *, #9953, .T. ) ;
#26363 = TOROIDAL_SURFACE ( 'NONE', #358, 11.00000000000000355, 1.000000000000000000 ) ;
#26364 = ORIENTED_EDGE ( 'NONE', *, *, #25536, .T. ) ;
#26365 = CARTESIAN_POINT ( 'NONE',  ( 147.4687500000000853, -2.485281374238585972, 6.000000000000005329 ) ) ;
#26366 = EDGE_LOOP ( 'NONE', ( #18480, #29306, #5604, #16590 ) ) ;
#26367 = CARTESIAN_POINT ( 'NONE',  ( 0.000000000000000000, 5.499999999999991118, -105.0000000000000426 ) ) ;
#26368 = CARTESIAN_POINT ( 'NONE',  ( 19.00000000000018474, -1.873492889144845464, -1.873492889145123019 ) ) ;
#26369 = EDGE_CURVE ( 'NONE', #13111, #11998, #18619, .T. ) ;
#26370 = CARTESIAN_POINT ( 'NONE',  ( -3.608439182435052128, -6.250000000000110134, -119.8080127018922667 ) ) ;
#26371 = ORIENTED_EDGE ( 'NONE', *, *, #1744, .T. ) ;
#26372 = CARTESIAN_POINT ( 'NONE',  ( 3.608439182435180470, -6.249999999999997335, -163.6919872981078754 ) ) ;
#26373 = FACE_OUTER_BOUND ( 'NONE', #15803, .T. ) ;
#26374 = FILL_AREA_STYLE ('',( #25789 ) ) ;
#26375 =( BOUNDED_CURVE ( )  B_SPLINE_CURVE ( 2, ( #5220, #2772, #14923, #12199, #12047, #3208, #17240, #14634, #7682 ),
 .UNSPECIFIED., .F., .F. ) 
 B_SPLINE_CURVE_WITH_KNOTS ( ( 3, 2, 2, 2, 3 ),
 ( 0.3916666666666666075, 0.3925925925925926041, 0.3944444444444444864, 0.3962962962962962576, 0.3972222222222222543 ),
 .UNSPECIFIED. ) 
 CURVE ( )  GEOMETRIC_REPRESENTATION_ITEM ( )  RATIONAL_B_SPLINE_CURVE ( ( 0.9330127018922194093, 0.9330127018922154125, 1.000000000000000000, 0.8660254037844388186, 1.000000000000000000, 0.8660254037844388186, 1.000000000000000000, 0.9330127018922154125, 0.9330127018922194093 ) ) 
 REPRESENTATION_ITEM ( '' )  );
#26376 = CARTESIAN_POINT ( 'NONE',  ( -5.412658773652684552, -3.125000000000099920, -58.43301270189227381 ) ) ;
#26377 = ORIENTED_EDGE ( 'NONE', *, *, #17630, .T. ) ;
#26378 = CARTESIAN_POINT ( 'NONE',  ( -2.145494852022792998, 10.79031218954990479, -19.39330237445248528 ) ) ;
#26379 = DIRECTION ( 'NONE',  ( -7.147005652999508048E-36, 5.642372883946980038E-36, 1.000000000000000000 ) ) ;
#26380 = CARTESIAN_POINT ( 'NONE',  ( -5.196152422706573404, -3.000000000000002665, -150.7113248654052313 ) ) ;
#26381 = MECHANICAL_DESIGN_GEOMETRIC_PRESENTATION_REPRESENTATION (  '', ( #22484 ), #8219 ) ;
#26382 = CARTESIAN_POINT ( 'NONE',  ( 120.9374999999996874, 2.500000000000114575, -1.035533905932629173 ) ) ;
#26383 = CARTESIAN_POINT ( 'NONE',  ( -0.07769256095284393648, -15.23231281889969679, 7.500000000000007105 ) ) ;
#26384 = CARTESIAN_POINT ( 'NONE',  ( 3.608439182435180470, -6.249999999999997335, -169.0580127018922383 ) ) ;
#26385 = CARTESIAN_POINT ( 'NONE',  ( 113.4761751345945555, 0.8284271247462053900, 2.000000000000212275 ) ) ;
#26386 = CARTESIAN_POINT ( 'NONE',  ( 23.81250000000003908, 0.8284271247463557142, -2.000000000000151879 ) ) ;
#26387 =( BOUNDED_CURVE ( )  B_SPLINE_CURVE ( 2, ( #9034, #23334, #18422, #2277, #8295, #18730, #27743, #27899, #20147 ),
 .UNSPECIFIED., .F., .T. ) 
 B_SPLINE_CURVE_WITH_KNOTS ( ( 3, 2, 2, 2, 3 ),
 ( 0.1472222222222221988, 0.1481481481481481399, 0.1499999999999999944, 0.1518518518518518490, 0.1527777777777777901 ),
 .UNSPECIFIED. ) 
 CURVE ( )  GEOMETRIC_REPRESENTATION_ITEM ( )  RATIONAL_B_SPLINE_CURVE ( ( 0.9330127018922196314, 0.9330127018922185211, 1.000000000000000000, 0.8660254037844388186, 1.000000000000000000, 0.8660254037844388186, 1.000000000000000000, 0.9330127018922184101, 0.9330127018922194093 ) ) 
 REPRESENTATION_ITEM ( '' )  );
#26388 = CARTESIAN_POINT ( 'NONE',  ( -4.763139720814407951, 2.749999999999946709, -116.7500000000000142 ) ) ;
#26389 = CARTESIAN_POINT ( 'NONE',  ( -3.175426480542816510, 5.499999999999865885, -115.3750000000000000 ) ) ;
#26390 = DIRECTION ( 'NONE',  ( 1.000000000000000000, 0.000000000000000000, 0.000000000000000000 ) ) ;
#26391 = CARTESIAN_POINT ( 'NONE',  ( 0.000000000000000000, -5.999999999999991118, -131.5386751345948255 ) ) ;
#26392 = VERTEX_POINT ( 'NONE', #4088 ) ;
#26393 = CARTESIAN_POINT ( 'NONE',  ( 8.673617379884035472E-16, -15.46112173798350753, 5.976438085239231590 ) ) ;
#26394 = CARTESIAN_POINT ( 'NONE',  ( 6.000000000000000888, -1.859271017917181981E-14, -109.5863248654052029 ) ) ;
#26395 = ORIENTED_EDGE ( 'NONE', *, *, #5061, .T. ) ;
#26396 =( NAMED_UNIT ( * ) SI_UNIT ( $, .STERADIAN. ) SOLID_ANGLE_UNIT ( ) );
#26397 = DIRECTION ( 'NONE',  ( -7.147005652999508048E-36, 5.642372883946980038E-36, 1.000000000000000000 ) ) ;
#26398 = EDGE_CURVE ( 'NONE', #11694, #8247, #3927, .T. ) ;
#26399 = CARTESIAN_POINT ( 'NONE',  ( 22.89882486540531303, 1.035533905932809473, 2.500000000000024425 ) ) ;
#26400 = VERTEX_POINT ( 'NONE', #18258 ) ;
#26401 = EDGE_CURVE ( 'NONE', #3499, #29376, #21741, .T. ) ;
#26402 = VERTEX_POINT ( 'NONE', #13662 ) ;
#26403 = ORIENTED_EDGE ( 'NONE', *, *, #5271, .T. ) ;
#26404 = CARTESIAN_POINT ( 'NONE',  ( 5.196152422706629359, 3.000000000000002665, -85.46132486540525974 ) ) ;
#26405 = CARTESIAN_POINT ( 'NONE',  ( 160.3125000000000284, 4.242640687119298093, -4.242640687119298093 ) ) ;
#26406 = ORIENTED_EDGE ( 'NONE', *, *, #12210, .T. ) ;
#26407 = AXIS2_PLACEMENT_3D ( 'NONE', #28569, #14209, #16948 ) ;
#26408 = CARTESIAN_POINT ( 'NONE',  ( 5.412658773652712085, -3.125000000000086153, -133.5669872981078470 ) ) ;
#26409 = CARTESIAN_POINT ( 'NONE',  ( 104.1247167782375556, -1.849990392679468076, 0.000000000000000000 ) ) ;
#26410 = CARTESIAN_POINT ( 'NONE',  ( 135.8257310488615417, -9.165151389911700974, -8.000000000000007105 ) ) ;
#26411 = CARTESIAN_POINT ( 'NONE',  ( 144.6636751345948255, 0.000000000000000000, 5.500000000000005329 ) ) ;
#26412 = ORIENTED_EDGE ( 'NONE', *, *, #2004, .T. ) ;
#26413 = CARTESIAN_POINT ( 'NONE',  ( 15.43750000000009770, -1.999999999999851674, 0.8284271247462354770 ) ) ;
#26414 = CARTESIAN_POINT ( 'NONE',  ( 0.1991271335306928347, -15.94713376385915637, -7.214644098438425246 ) ) ;
#26415 = LINE ( 'NONE', #21829, #18647 ) ;
#26416 = CARTESIAN_POINT ( 'NONE',  ( 137.3288997308104342, 4.999999999999989342, -2.071067811865468400 ) ) ;
#26417 = LINE ( 'NONE', #24122, #1548 ) ;
#26418 =( NAMED_UNIT ( * ) SI_UNIT ( $, .STERADIAN. ) SOLID_ANGLE_UNIT ( ) );
#26419 = SURFACE_STYLE_USAGE ( .BOTH. , #14926 ) ;
#26420 = CARTESIAN_POINT ( 'NONE',  ( 6.000000000000000888, 7.762456499804235646E-14, -138.0863248654052029 ) ) ;
#26421 = CARTESIAN_POINT ( 'NONE',  ( 105.1249999999999005, 1.767766952966265404, 1.767766952966431937 ) ) ;
#26422 =( BOUNDED_CURVE ( )  B_SPLINE_CURVE ( 2, ( #12452, #21942, #15035, #19778, #5480, #10427, #29126, #3325, #26090 ),
 .UNSPECIFIED., .F., .T. ) 
 B_SPLINE_CURVE_WITH_KNOTS ( ( 3, 2, 2, 2, 3 ),
 ( 0.2874999999999998113, 0.2937500000000000666, 0.3000000000000002665, 0.3062500000000005773, 0.3125000000000007772 ),
 .UNSPECIFIED. ) 
 CURVE ( )  GEOMETRIC_REPRESENTATION_ITEM ( )  RATIONAL_B_SPLINE_CURVE ( ( 1.000000000000001998, 0.9238795325112847401, 1.000000000000000000, 0.9238795325112867385, 1.000000000000000000, 0.9238795325112867385, 1.000000000000000000, 0.9238795325112773016, 1.000000000000009548 ) ) 
 REPRESENTATION_ITEM ( '' )  );
#26423 = CARTESIAN_POINT ( 'NONE',  ( 4.763139720814407951, -2.749999999999988454, -134.0000000000000000 ) ) ;
#26424 = DIRECTION ( 'NONE',  ( -7.147005652999508048E-36, 5.642372883946980038E-36, 1.000000000000000000 ) ) ;
#26425 = ORIENTED_EDGE ( 'NONE', *, *, #24669, .T. ) ;
#26426 = CARTESIAN_POINT ( 'NONE',  ( -2.775557561562891351E-14, -5.500000000000115463, -48.75000000000001421 ) ) ;
#26427 = CARTESIAN_POINT ( 'NONE',  ( 1.000000000000000888, -15.50000000000001421, -5.656854249492387687 ) ) ;
#26428 = EDGE_LOOP ( 'NONE', ( #6726, #7734, #24828, #18734 ) ) ;
#26429 = CARTESIAN_POINT ( 'NONE',  ( 118.6247167782376408, 1.849990392679468076, 0.000000000000000000 ) ) ;
#26430 = FILL_AREA_STYLE ('',( #17105 ) ) ;
#26431 = CARTESIAN_POINT ( 'NONE',  ( -7.216878364870328078, 0.000000000000000000, -92.19198729810779014 ) ) ;
#26432 = ADVANCED_FACE ( 'NONE', ( #23005 ), #1948, .T. ) ;
#26433 = CARTESIAN_POINT ( 'NONE',  ( 135.0000000000000284, 6.000000000000005329, 0.000000000000000000 ) ) ;
#26434 = EDGE_CURVE ( 'NONE', #1653, #476, #24679, .T. ) ;
#26435 = CARTESIAN_POINT ( 'NONE',  ( 20.71132486540530593, 2.500000000000057732, -1.665334536937734811E-13 ) ) ;
#26436 = CARTESIAN_POINT ( 'NONE',  ( 118.9374999999996589, 2.500000000000234479, -1.035533905932568999 ) ) ;
#26437 = ORIENTED_EDGE ( 'NONE', *, *, #16303, .F. ) ;
#26438 = DIRECTION ( 'NONE',  ( 0.000000000000000000, -1.000000000000000000, -1.010643099614862550E-15 ) ) ;
#26439 = CARTESIAN_POINT ( 'NONE',  ( -4.763139720814407951, 2.749999999999946709, -125.7500000000000284 ) ) ;
#26440 = CARTESIAN_POINT ( 'NONE',  ( 9.812500000000115463, 0.8284271247462955401, -2.000000000000091926 ) ) ;
#26441 = ORIENTED_EDGE ( 'NONE', *, *, #17425, .F. ) ;
#26442 = CARTESIAN_POINT ( 'NONE',  ( 3.464101615137757051, -5.999999999999979572, -82.83632486540524553 ) ) ;
#26443 = CARTESIAN_POINT ( 'NONE',  ( 0.000000000000000000, 5.499999999999991118, -61.50000000000000000 ) ) ;
#26444 = VECTOR ( 'NONE', #656, 1000.000000000000000 ) ;
#26445 = CARTESIAN_POINT ( 'NONE',  ( 0.000000000000000000, 0.000000000000000000, -43.99152654425658682 ) ) ;
#26446 = CARTESIAN_POINT ( 'NONE',  ( -6.000000000000007105, -1.607695154586655129, -62.84668783648705670 ) ) ;
#26447 = CARTESIAN_POINT ( 'NONE',  ( -5.412658773652739619, 3.124999999999975131, -82.68301270189226670 ) ) ;
#26448 = VECTOR ( 'NONE', #12941, 1000.000000000000000 ) ;
#26449 = CARTESIAN_POINT ( 'NONE',  ( 160.0000000000000284, -59.99999999999980105, 3.000000000000002665 ) ) ;
#26450 = CARTESIAN_POINT ( 'NONE',  ( 6.000000000000000888, -1.859271017917181981E-14, -168.0863248654052029 ) ) ;
#26451 = PRESENTATION_STYLE_ASSIGNMENT (( #14813 ) ) ;
#26452 = CARTESIAN_POINT ( 'NONE',  ( 3.464101615137852974, 5.999999999999884537, -61.33632486540521001 ) ) ;
#26453 = CARTESIAN_POINT ( 'NONE',  ( 114.5627832217621602, 0.7662911109078588412, 1.849990392679712103 ) ) ;
#26454 = CARTESIAN_POINT ( 'NONE',  ( -3.175426480542816066, 5.499999999999865885, -143.8750000000000000 ) ) ;
#26455 = CARTESIAN_POINT ( 'NONE',  ( 140.0304953857124701, -9.269783219788546802, 7.622864659627890838 ) ) ;
#26456 = CARTESIAN_POINT ( 'NONE',  ( -5.412658773652739619, 3.124999999999975131, -156.1830127018922667 ) ) ;
#26457 = FILL_AREA_STYLE_COLOUR ( '', #21899 ) ;
#26458 = CARTESIAN_POINT ( 'NONE',  ( 0.000000000000000000, 5.499999999999991118, -69.00000000000000000 ) ) ;
#26459 = CARTESIAN_POINT ( 'NONE',  ( 3.175426480543072749, -5.500000000000105693, -57.62500000000004974 ) ) ;
#26460 = CARTESIAN_POINT ( 'NONE',  ( 144.5773502691896510, 5.000000000000004441, 0.000000000000000000 ) ) ;
#26461 = CARTESIAN_POINT ( 'NONE',  ( 152.5312500000000568, -2.485281374238556218, -6.000000000000005329 ) ) ;
#26462 = DIRECTION ( 'NONE',  ( 1.000000000000000000, -5.551115123125774074E-17, 0.000000000000000000 ) ) ;
#26463 = CARTESIAN_POINT ( 'NONE',  ( -5.999999999999963585, 1.780251999655701777E-13, -104.9136751345948255 ) ) ;
#26464 = EDGE_CURVE ( 'NONE', #29267, #20178, #1326, .T. ) ;
#26465 = ORIENTED_EDGE ( 'NONE', *, *, #17146, .F. ) ;
#26466 = CARTESIAN_POINT ( 'NONE',  ( 145.3125000000000284, 4.242640687119298093, -4.242640687119298093 ) ) ;
#26467 = AXIS2_PLACEMENT_3D ( 'NONE', #1529, #11085, #25022 ) ;
#26468 = AXIS2_PLACEMENT_3D ( 'NONE', #26700, #10614, #11193 ) ;
#26469 = CARTESIAN_POINT ( 'NONE',  ( 135.0448603013149977, 1.007610841837577542, 5.499999999999951150 ) ) ;
#26470 = CARTESIAN_POINT ( 'NONE',  ( 0.000000000000000000, 5.499999999999991118, -178.5000000000000000 ) ) ;
#26471 = CARTESIAN_POINT ( 'NONE',  ( 20.37500000000017053, -1.414213562372979016, 1.414213562373034527 ) ) ;
#26472 = ORIENTED_EDGE ( 'NONE', *, *, #10649, .T. ) ;
#26473 = CARTESIAN_POINT ( 'NONE',  ( -4.763139720814407951, -2.750000000000016431, -79.00000000000001421 ) ) ;
#26474 = DIRECTION ( 'NONE',  ( -8.326672684688675286E-17, -2.081668171172168821E-17, 1.000000000000000000 ) ) ;
#26475 =( NAMED_UNIT ( * ) PLANE_ANGLE_UNIT ( ) SI_UNIT ( $, .RADIAN. ) );
#26476 = CARTESIAN_POINT ( 'NONE',  ( 0.000000000000000000, 0.000000000000000000, 0.000000000000000000 ) ) ;
#26477 = PRESENTATION_STYLE_ASSIGNMENT (( #28934 ) ) ;
#26478 = CARTESIAN_POINT ( 'NONE',  ( 140.5384615384615756, -11.07692307692309264, 4.615384615384626521 ) ) ;
#26479 = CARTESIAN_POINT ( 'NONE',  ( -3.175426480542816066, 5.499999999999865885, -160.3750000000000000 ) ) ;
#26480 = CARTESIAN_POINT ( 'NONE',  ( -5.999999999999919176, 1.607695154586804565, -161.4033121635129930 ) ) ;
#26481 = CARTESIAN_POINT ( 'NONE',  ( -3.175426480542816510, 5.499999999999865885, -148.3750000000000568 ) ) ;
#26482 = EDGE_CURVE ( 'NONE', #26042, #2096, #18255, .T. ) ;
#26483 = DIRECTION ( 'NONE',  ( -7.147005652999508048E-36, 5.642372883946980038E-36, 1.000000000000000000 ) ) ;
#26484 = CARTESIAN_POINT ( 'NONE',  ( 3.464101615137757051, -5.999999999999979572, -51.91367513459486105 ) ) ;
#26485 = ADVANCED_FACE ( 'NONE', ( #23165 ), #21303, .T. ) ;
#26486 = CARTESIAN_POINT ( 'NONE',  ( -3.175426480542816066, -5.500000000000057732, -93.87500000000002842 ) ) ;
#26487 = PLANE ( 'NONE',  #28959 ) ;
#26488 = CARTESIAN_POINT ( 'NONE',  ( -4.763139720814407951, -2.750000000000016431, -82.00000000000001421 ) ) ;
#26489 = CARTESIAN_POINT ( 'NONE',  ( 135.3675748654052313, -5.500000000000012434, 2.278174593052012309 ) ) ;
#26490 = CARTESIAN_POINT ( 'NONE',  ( 157.3273502691896510, -5.000000000000004441, 0.000000000000000000 ) ) ;
#26491 = CARTESIAN_POINT ( 'NONE',  ( -5.196152422706601826, 2.999999999999975131, -143.4613248654052029 ) ) ;
#26492 = CARTESIAN_POINT ( 'NONE',  ( 24.00000000000013145, 2.000000000000057288, -1.665334536937734811E-13 ) ) ;
#26493 = CARTESIAN_POINT ( 'NONE',  ( 108.9999999999998579, 2.500000000000030198, 1.110223024625156540E-13 ) ) ;
#26494 = FACE_OUTER_BOUND ( 'NONE', #25464, .T. ) ;
#26495 = CARTESIAN_POINT ( 'NONE',  ( -5.196152422706601826, 2.999999999999975131, -72.03867513459482552 ) ) ;
#26496 = ADVANCED_FACE ( 'NONE', ( #20852 ), #16126, .T. ) ;
#26497 = CARTESIAN_POINT ( 'NONE',  ( 161.0000000000000284, 3.467572205841706889, 4.269185284954735593 ) ) ;
#26498 =( BOUNDED_SURFACE ( )  B_SPLINE_SURFACE ( 3, 2, ( 
 ( #13522, #9336, #30368 ),
 ( #27739, #16292, #25764 ),
 ( #22862, #11677, #1961 ),
 ( #8883, #29903, #14143 ),
 ( #1800, #4406, #25442 ),
 ( #21170, #18726, #112 ),
 ( #11206, #23176, #25135 ),
 ( #18575, #23015, #15836 ),
 ( #20713, #28199, #16136 ),
 ( #4100, #20552, #18271 ),
 ( #27583, #6561, #4253 ),
 ( #15982, #13674, #9030 ),
 ( #18419, #20865, #11366 ),
 ( #13831, #30215, #9178 ) ),
 .UNSPECIFIED., .F., .F., .T. ) 
 B_SPLINE_SURFACE_WITH_KNOTS ( ( 4, 2, 2, 2, 2, 2, 4 ),
 ( 3, 3 ),
 ( 0.007035869656342713836, 0.007146012451658744456, 0.007256155246974775076, 0.007311226644632790386, 0.007366298042290805696, 0.007421369439948821006, 0.007476440837606836316 ),
 ( 0.000000000000000000, 1.000000000000000000 ),
 .UNSPECIFIED. ) 
 GEOMETRIC_REPRESENTATION_ITEM ( )  RATIONAL_B_SPLINE_SURFACE ( (
 ( 1.000000000000000000, 0.7743236465966892856, 1.000000000000000000),
 ( 1.000000000000000000, 0.7823573883663251793, 1.000000000000000000),
 ( 1.000000000000000000, 0.7919060189340916267, 1.000000000000000000),
 ( 1.000000000000000000, 0.8152203555693537940, 1.000000000000000000),
 ( 1.000000000000000000, 0.8293580484731973845, 1.000000000000000000),
 ( 1.000000000000000000, 0.8517285253148718649, 1.000000000000000000),
 ( 1.000000000000000000, 0.8593271320052130458, 1.000000000000000000),
 ( 1.000000000000000000, 0.8720599197349646614, 1.000000000000000000),
 ( 1.000000000000000000, 0.8771186710024685418, 1.000000000000000000),
 ( 1.000000000000000000, 0.8813077611509017029, 1.000000000000000000),
 ( 1.000000000000000000, 0.8802096620080653855, 1.000000000000000000),
 ( 1.000000000000000000, 0.8725983457344340666, 1.000000000000000000),
 ( 1.000000000000000000, 0.8663204784655903490, 1.000000000000000000),
 ( 1.000000000000000000, 0.8593225670956808893, 1.000000000000000000) ) ) 
 REPRESENTATION_ITEM ( '' )  SURFACE ( )  );
#26499 = EDGE_CURVE ( 'NONE', #10998, #13277, #16229, .T. ) ;
#26500 = ORIENTED_EDGE ( 'NONE', *, *, #3601, .T. ) ;
#26501 = CARTESIAN_POINT ( 'NONE',  ( 161.5312500000000568, -2.485281374238555774, -6.000000000000005329 ) ) ;
#26502 = CARTESIAN_POINT ( 'NONE',  ( 6.000000000000000888, 7.762456499804235646E-14, -143.1636751345948255 ) ) ;
#26503 = CARTESIAN_POINT ( 'NONE',  ( 6.000000000000000888, 1.743066579297358182E-13, -81.08632486540518869 ) ) ;
#26504 = CARTESIAN_POINT ( 'NONE',  ( 104.3747167782376124, -5.551115123125782702E-14, -1.849990392679523588 ) ) ;
#26505 = VECTOR ( 'NONE', #19525, 1000.000000000000000 ) ;
#26506 = VERTEX_POINT ( 'NONE', #16724 ) ;
#26507 =( BOUNDED_CURVE ( )  B_SPLINE_CURVE ( 2, ( #28541, #23962, #7799, #12319, #26542, #17066, #24698, #10594, #22985 ),
 .UNSPECIFIED., .F., .F. ) 
 B_SPLINE_CURVE_WITH_KNOTS ( ( 3, 2, 2, 2, 3 ),
 ( 0.7361111111111111605, 0.7370370370370370461, 0.7388888888888889284, 0.7407407407407406996, 0.7416666666666666963 ),
 .UNSPECIFIED. ) 
 CURVE ( )  GEOMETRIC_REPRESENTATION_ITEM ( )  RATIONAL_B_SPLINE_CURVE ( ( 0.9330127018922194093, 0.9330127018922234061, 1.000000000000000000, 0.8660254037844388186, 1.000000000000000000, 0.8660254037844388186, 1.000000000000000000, 0.9330127018922154125, 0.9330127018922194093 ) ) 
 REPRESENTATION_ITEM ( '' )  );
#26508 = AXIS2_PLACEMENT_3D ( 'NONE', #16132, #18267, #27578 ) ;
#26509 = ORIENTED_EDGE ( 'NONE', *, *, #13249, .F. ) ;
#26510 = ORIENTED_EDGE ( 'NONE', *, *, #5928, .F. ) ;
#26511 = CARTESIAN_POINT ( 'NONE',  ( -2.775557561562891351E-14, -5.500000000000115463, -105.7500000000000142 ) ) ;
#26512 = CARTESIAN_POINT ( 'NONE',  ( 18.75000000000012790, -1.873492889144900975, 1.873492889144845464 ) ) ;
#26513 = CARTESIAN_POINT ( 'NONE',  ( 5.412658773652739619, 3.124999999999988898, -126.6830127018922525 ) ) ;
#26514 = AXIS2_PLACEMENT_3D ( 'NONE', #7120, #20971, #27537 ) ;
#26515 = ORIENTED_EDGE ( 'NONE', *, *, #14815, .F. ) ;
#26516 = CARTESIAN_POINT ( 'NONE',  ( 113.9613248654051034, 2.775557561562891351E-14, 2.000000000000223821 ) ) ;
#26517 = CARTESIAN_POINT ( 'NONE',  ( -7.216878364870328078, 0.000000000000000000, -161.1919872981078754 ) ) ;
#26518 = CARTESIAN_POINT ( 'NONE',  ( -1.110223024625164676E-16, 2.000000000000012879, 2.021286199229734960E-15 ) ) ;
#26519 = LINE ( 'NONE', #29270, #23849 ) ;
#26520 = CARTESIAN_POINT ( 'NONE',  ( -3.608439182435052128, -6.250000000000110134, -62.80801270189225249 ) ) ;
#26521 = ORIENTED_EDGE ( 'NONE', *, *, #5351, .F. ) ;
#26522 = CARTESIAN_POINT ( 'NONE',  ( -3.464101615137725076, 5.999999999999979572, -117.1636751345948255 ) ) ;
#26523 = CARTESIAN_POINT ( 'NONE',  ( 5.196152422706629359, -2.999999999999988898, -132.2113248654052029 ) ) ;
#26524 = FACE_OUTER_BOUND ( 'NONE', #1056, .T. ) ;
#26525 = CARTESIAN_POINT ( 'NONE',  ( -3.175426480542816510, -5.500000000000057732, -174.8750000000000284 ) ) ;
#26526 = CARTESIAN_POINT ( 'NONE',  ( 105.3752832217622739, 1.849990392679523588, 0.000000000000000000 ) ) ;
#26527 = CARTESIAN_POINT ( 'NONE',  ( -0.01297627431098077530, -14.38419007667407890, 8.362424020360270660 ) ) ;
#26528 = CARTESIAN_POINT ( 'NONE',  ( -7.216878364870328078, 0.000000000000000000, -169.5580127018922383 ) ) ;
#26529 = FACE_OUTER_BOUND ( 'NONE', #9726, .T. ) ;
#26530 = EDGE_CURVE ( 'NONE', #19941, #15497, #27816, .T. ) ;
#26531 = CARTESIAN_POINT ( 'NONE',  ( 24.81250000000012079, 0.8284271247463557142, -2.000000000000091926 ) ) ;
#26532 = AXIS2_PLACEMENT_3D ( 'NONE', #8673, #8981, #6054 ) ;
#26533 = CARTESIAN_POINT ( 'NONE',  ( -6.350852961085760029, -1.281975124255709124E-13, -119.6250000000000426 ) ) ;
#26534 = CARTESIAN_POINT ( 'NONE',  ( -5.196152422706601826, 2.999999999999975131, -84.03867513459483973 ) ) ;
#26535 = CARTESIAN_POINT ( 'NONE',  ( -3.175426480542816510, -5.500000000000057732, -114.8749999999999858 ) ) ;
#26536 = CARTESIAN_POINT ( 'NONE',  ( 5.196152422706629359, -2.999999999999988898, -131.2886751345948539 ) ) ;
#26537 = EDGE_LOOP ( 'NONE', ( #22608, #10631, #11429, #29904 ) ) ;
#26538 = CARTESIAN_POINT ( 'NONE',  ( 18.75000000000015632, 1.873492889145067508, 1.873492889144734441 ) ) ;
#26539 = CARTESIAN_POINT ( 'NONE',  ( 5.196152422706629359, -2.999999999999988898, -90.21132486540523132 ) ) ;
#26540 = CARTESIAN_POINT ( 'NONE',  ( 5.196152422706629359, 3.000000000000002665, -109.4613248654052171 ) ) ;
#26541 = EDGE_CURVE ( 'NONE', #26551, #23459, #21393, .T. ) ;
#26542 = CARTESIAN_POINT ( 'NONE',  ( 0.000000000000000000, -5.999999999999991118, -145.9613248654052597 ) ) ;
#26543 = ORIENTED_EDGE ( 'NONE', *, *, #2146, .F. ) ;
#26544 = AXIS2_PLACEMENT_3D ( 'NONE', #11491, #2087, #18841 ) ;
#26545 = DIRECTION ( 'NONE',  ( 0.000000000000000000, 0.000000000000000000, -1.000000000000000000 ) ) ;
#26546 = CARTESIAN_POINT ( 'NONE',  ( 4.763139720814407951, 2.750000000000002665, -178.7500000000000284 ) ) ;
#26547 = CARTESIAN_POINT ( 'NONE',  ( -5.412658773652684552, -3.125000000000099920, -84.56698729810784698 ) ) ;
#26548 = CARTESIAN_POINT ( 'NONE',  ( 22.71132486540533435, 2.500000000000057732, -1.665334536937734811E-13 ) ) ;
#26549 = ORIENTED_EDGE ( 'NONE', *, *, #9084, .F. ) ;
#26550 = FACE_OUTER_BOUND ( 'NONE', #2562, .T. ) ;
#26551 = VERTEX_POINT ( 'NONE', #13820 ) ;
#26552 = CARTESIAN_POINT ( 'NONE',  ( -5.999999999999963585, 1.780251999655701777E-13, -84.83632486540523132 ) ) ;
#26553 = CARTESIAN_POINT ( 'NONE',  ( 159.8437500000000000, -6.000000000000005329, -2.485281374238555774 ) ) ;
#26554 = CIRCLE ( 'NONE', #11912, 1.000000000000000000 ) ;
#26555 = ORIENTED_EDGE ( 'NONE', *, *, #22651, .F. ) ;
#26556 = CARTESIAN_POINT ( 'NONE',  ( -5.999999999999963585, -1.487416814333745711E-14, -143.9136751345948255 ) ) ;
#26557 = CARTESIAN_POINT ( 'NONE',  ( -3.608439182435052128, -6.250000000000110134, -133.9419872981078186 ) ) ;
#26558 = CARTESIAN_POINT ( 'NONE',  ( 0.000000000000000000, 2.220446049250313081E-16, -4.000000000000010658 ) ) ;
#26559 = CARTESIAN_POINT ( 'NONE',  ( 0.000000000000000000, -10.00000000000000888, -5.000000000000004441 ) ) ;
#26560 = FACE_OUTER_BOUND ( 'NONE', #6468, .T. ) ;
#26561 = ORIENTED_EDGE ( 'NONE', *, *, #2428, .T. ) ;
#26562 = CARTESIAN_POINT ( 'NONE',  ( 16.18750000000014566, 0.8284271247462955401, 2.000000000000031530 ) ) ;
#26563 = CARTESIAN_POINT ( 'NONE',  ( -5.196152422706601826, 2.999999999999975131, -135.0386751345948824 ) ) ;
#26564 = CARTESIAN_POINT ( 'NONE',  ( 0.000000000000000000, -5.999999999999991118, -139.0386751345948255 ) ) ;
#26565 = CARTESIAN_POINT ( 'NONE',  ( 139.5788997308104342, -4.999999999999989342, 2.071067811865468400 ) ) ;
#26566 = DIRECTION ( 'NONE',  ( 0.000000000000000000, 0.000000000000000000, 1.000000000000000000 ) ) ;
#26567 = DIRECTION ( 'NONE',  ( -7.147005652999508048E-36, 5.642372883946980038E-36, 1.000000000000000000 ) ) ;
#26568 = DIRECTION ( 'NONE',  ( -7.147005652999508048E-36, 5.642372883946980038E-36, 1.000000000000000000 ) ) ;
#26569 = CARTESIAN_POINT ( 'NONE',  ( 108.0624999999998153, 2.500000000000115019, 1.035533905932929599 ) ) ;
#26570 = ADVANCED_FACE ( 'NONE', ( #16281 ), #24859, .F. ) ;
#26571 = CARTESIAN_POINT ( 'NONE',  ( 107.5238248654050466, 0.8284271247462654530, -1.999999999999851674 ) ) ;
#26572 = CARTESIAN_POINT ( 'NONE',  ( 4.763139720814407951, 2.750000000000002665, -141.2500000000000000 ) ) ;
#26573 = ORIENTED_EDGE ( 'NONE', *, *, #6480, .F. ) ;
#26574 = CARTESIAN_POINT ( 'NONE',  ( -6.000000000000000888, 1.067854986875958443E-15, 7.560779664488942560E-35 ) ) ;
#26575 = CARTESIAN_POINT ( 'NONE',  ( -3.175426480542816066, -5.500000000000057732, -47.37500000000000000 ) ) ;
#26576 = CARTESIAN_POINT ( 'NONE',  ( -3.464101615137757051, -5.999999999999979572, -160.1636751345947687 ) ) ;
#26577 = EDGE_CURVE ( 'NONE', #1984, #14122, #19583, .T. ) ;
#26578 = CARTESIAN_POINT ( 'NONE',  ( 0.000000000000000000, 9.000000000000007105, 3.000000000000002665 ) ) ;
#26579 = EDGE_LOOP ( 'NONE', ( #20085, #9469, #3453, #21210 ) ) ;
#26580 = CARTESIAN_POINT ( 'NONE',  ( 119.1247167782375698, -1.849990392679412565, 1.110223024625156540E-13 ) ) ;
#26581 = CARTESIAN_POINT ( 'NONE',  ( -5.412658773652739619, 3.124999999999975131, -98.31698729810783277 ) ) ;
#26582 = CARTESIAN_POINT ( 'NONE',  ( 5.196152422706629359, 3.000000000000002665, -173.0386751345947971 ) ) ;
#26583 = CARTESIAN_POINT ( 'NONE',  ( -38.99999999999998579, -59.99999999999980105, 3.000000000000002665 ) ) ;
#26584 = CARTESIAN_POINT ( 'NONE',  ( 113.9999999999998153, 2.500000000000085265, 0.000000000000000000 ) ) ;
#26585 = ORIENTED_EDGE ( 'NONE', *, *, #21814, .T. ) ;
#26586 = AXIS2_PLACEMENT_3D ( 'NONE', #18145, #27457, #29319 ) ;
#26587 = ORIENTED_EDGE ( 'NONE', *, *, #13519, .F. ) ;
#26588 = DIRECTION ( 'NONE',  ( -1.000000000000000000, -1.665334536937731113E-16, 1.526556658859586792E-16 ) ) ;
#26589 = CARTESIAN_POINT ( 'NONE',  ( -4.763139720814407951, -2.750000000000016431, -61.00000000000000000 ) ) ;
#26590 = CARTESIAN_POINT ( 'NONE',  ( 140.5386751345948255, -5.500000000000005329, 0.000000000000000000 ) ) ;
#26591 = CYLINDRICAL_SURFACE ( 'NONE', #2439, 6.000000000000000888 ) ;
#26592 = CARTESIAN_POINT ( 'NONE',  ( -5.999999999999963585, -1.487416814333745711E-14, -67.41367513459481131 ) ) ;
#26593 = CARTESIAN_POINT ( 'NONE',  ( -5.412658773652684552, -3.125000000000099920, -73.43301270189222407 ) ) ;
#26594 =( BOUNDED_CURVE ( )  B_SPLINE_CURVE ( 2, ( #24272, #26870, #1084, #22295, #27030, #5995, #8136, #15570, #24739 ),
 .UNSPECIFIED., .F., .T. ) 
 B_SPLINE_CURVE_WITH_KNOTS ( ( 3, 2, 2, 2, 3 ),
 ( 0.4843750000000000000, 0.4921875000000000000, 0.5000000000000000000, 0.5078125000000000000, 0.5156250000000000000 ),
 .UNSPECIFIED. ) 
 CURVE ( )  GEOMETRIC_REPRESENTATION_ITEM ( )  RATIONAL_B_SPLINE_CURVE ( ( 1.000000000000000000, 0.9238795325112867385, 1.000000000000000000, 0.9238795325112867385, 1.000000000000000000, 0.9238795325112867385, 1.000000000000000000, 0.9238795325112867385, 1.000000000000000000 ) ) 
 REPRESENTATION_ITEM ( '' )  );
#26595 = CARTESIAN_POINT ( 'NONE',  ( 0.000000000000000000, 0.000000000000000000, 0.000000000000000000 ) ) ;
#26596 = CARTESIAN_POINT ( 'NONE',  ( 158.7038997308104058, 2.071067811865468400, 4.999999999999989342 ) ) ;
#26597 = CARTESIAN_POINT ( 'NONE',  ( 152.8199251345948255, -2.278174593051950136, -5.500000000000074607 ) ) ;
#26598 = SURFACE_SIDE_STYLE ('',( #7865 ) ) ;
#26599 = EDGE_CURVE ( 'NONE', #1119, #17742, #24995, .T. ) ;
#26600 = ADVANCED_FACE ( 'NONE', ( #14560 ), #984, .F. ) ;
#26601 =( GEOMETRIC_REPRESENTATION_CONTEXT ( 3 ) GLOBAL_UNCERTAINTY_ASSIGNED_CONTEXT ( ( #19266 ) ) GLOBAL_UNIT_ASSIGNED_CONTEXT ( ( #19158, #28186, #21459 ) ) REPRESENTATION_CONTEXT ( 'NONE', 'WORKASPACE' ) );
#26602 = CARTESIAN_POINT ( 'NONE',  ( -3.175426480542816066, 5.499999999999865885, -142.3750000000000568 ) ) ;
#26603 = CARTESIAN_POINT ( 'NONE',  ( 5.999999999999949374, 1.607695154586804565, -69.01933756729745539 ) ) ;
#26604 = CARTESIAN_POINT ( 'NONE',  ( 2.775557561562891351E-14, 6.250000000000033751, -156.4330127018922383 ) ) ;
#26605 = LINE ( 'NONE', #14670, #2742 ) ;
#26606 = FILL_AREA_STYLE ('',( #26457 ) ) ;
#26607 = CARTESIAN_POINT ( 'NONE',  ( 3.175426480543072749, -5.500000000000105693, -72.62500000000005684 ) ) ;
#26608 = CARTESIAN_POINT ( 'NONE',  ( 4.763139720814407951, 2.750000000000002665, -54.25000000000002132 ) ) ;
#26609 = ORIENTED_EDGE ( 'NONE', *, *, #25239, .F. ) ;
#26610 = CARTESIAN_POINT ( 'NONE',  ( 137.4523502691896510, 0.000000000000000000, 5.000000000000004441 ) ) ;
#26611 = CARTESIAN_POINT ( 'NONE',  ( 153.0000000000000284, 6.000000000000005329, 0.000000000000000000 ) ) ;
#26612 = CARTESIAN_POINT ( 'NONE',  ( -5.999999999999971578, 1.607695154586715303, -97.48066243270258724 ) ) ;
#26613 = CARTESIAN_POINT ( 'NONE',  ( 6.000000000000000888, 1.743066579297358182E-13, -104.1636751345948397 ) ) ;
#26614 = VECTOR ( 'NONE', #20585, 1000.000000000000000 ) ;
#26615 = ORIENTED_EDGE ( 'NONE', *, *, #17989, .F. ) ;
#26616 = CARTESIAN_POINT ( 'NONE',  ( 144.4687500000000568, -2.485281374238585972, 6.000000000000005329 ) ) ;
#26617 = CARTESIAN_POINT ( 'NONE',  ( 161.4205085250501668, -5.148837675204802622, -2.939615011427564539 ) ) ;
#26618 = CARTESIAN_POINT ( 'NONE',  ( 104.9785324208944957, -0.3128015976218990746, 1.970815887930343235 ) ) ;
#26619 = CARTESIAN_POINT ( 'NONE',  ( 18.37500000000008527, -1.414213562373090038, 1.414213562372867994 ) ) ;
#26620 = CARTESIAN_POINT ( 'NONE',  ( 5.412658773652739619, 3.124999999999988898, -148.3169872981078186 ) ) ;
#26621 = CARTESIAN_POINT ( 'NONE',  ( 3.175426480543072749, 5.499999999999865885, -84.12499999999997158 ) ) ;
#26622 = CARTESIAN_POINT ( 'NONE',  ( 13.37500000000010836, 2.649519052838444910, -5.551115123125782702E-14 ) ) ;
#26623 = CARTESIAN_POINT ( 'NONE',  ( 7.216878364870455975, -6.409875621278545621E-14, -98.30801270189222407 ) ) ;
#26624 = ORIENTED_EDGE ( 'NONE', *, *, #26868, .F. ) ;
#26625 = CARTESIAN_POINT ( 'NONE',  ( 0.000000000000000000, 0.000000000000000000, 0.000000000000000000 ) ) ;
#26626 = CYLINDRICAL_SURFACE ( 'NONE', #3901, 2.000000000000012879 ) ;
#26627 = DIRECTION ( 'NONE',  ( 0.000000000000000000, 0.000000000000000000, 1.000000000000000000 ) ) ;
#26628 =( NAMED_UNIT ( * ) SI_UNIT ( $, .STERADIAN. ) SOLID_ANGLE_UNIT ( ) );
#26629 = EDGE_CURVE ( 'NONE', #5531, #9311, #12710, .T. ) ;
#26630 = CARTESIAN_POINT ( 'NONE',  ( 0.000000000000000000, 5.499999999999991118, -163.5000000000000284 ) ) ;
#26631 = CARTESIAN_POINT ( 'NONE',  ( -3.464101615137757051, -5.999999999999979572, -60.58632486540521001 ) ) ;
#26632 = CARTESIAN_POINT ( 'NONE',  ( -4.763139720814407951, 2.749999999999946709, -148.2500000000000000 ) ) ;
#26633 = CARTESIAN_POINT ( 'NONE',  ( 116.8511751345945129, -1.999999999999881650, -0.8284271247460553989 ) ) ;
#26634 =( BOUNDED_CURVE ( )  B_SPLINE_CURVE ( 2, ( #7348, #2443, #28071, #30082, #16755, #21043, #5021, #14451, #573 ),
 .UNSPECIFIED., .F., .F. ) 
 B_SPLINE_CURVE_WITH_KNOTS ( ( 3, 2, 2, 2, 3 ),
 ( 0.08749999999999961975, 0.09374999999999986122, 0.1000000000000000888, 0.1062500000000003164, 0.1125000000000005579 ),
 .UNSPECIFIED. ) 
 CURVE ( )  GEOMETRIC_REPRESENTATION_ITEM ( )  RATIONAL_B_SPLINE_CURVE ( ( 1.000000000000004663, 0.9238795325112821866, 1.000000000000000000, 0.9238795325112867385, 1.000000000000000000, 0.9238795325112867385, 1.000000000000000000, 0.9238795325112799661, 1.000000000000006661 ) ) 
 REPRESENTATION_ITEM ( '' )  );
#26635 = CARTESIAN_POINT ( 'NONE',  ( 3.175426480543072749, 5.499999999999865885, -96.12500000000004263 ) ) ;
#26636 = PRESENTATION_STYLE_ASSIGNMENT (( #10864 ) ) ;
#26637 = CARTESIAN_POINT ( 'NONE',  ( -3.175426480542816510, 5.499999999999865885, -82.37500000000002842 ) ) ;
#26638 = CARTESIAN_POINT ( 'NONE',  ( 153.3898502691896510, 3.535533905932725318, -3.535533905932725318 ) ) ;
#26639 = CARTESIAN_POINT ( 'NONE',  ( -5.196152422706573404, -3.000000000000002665, -72.71132486540521711 ) ) ;
#26640 = CARTESIAN_POINT ( 'NONE',  ( 161.0000000000000284, -5.424442335930618420, -0.9085292203135086897 ) ) ;
#26641 = CARTESIAN_POINT ( 'NONE',  ( 1.000000000000000888, -14.99923475244191451, 9.015151515151503148 ) ) ;
#26642 = CARTESIAN_POINT ( 'NONE',  ( -5.196152422706601826, 2.999999999999975131, -128.4613248654051745 ) ) ;
#26643 = CARTESIAN_POINT ( 'NONE',  ( 0.000000000000000000, 5.999999999999977796, -72.28867513459485394 ) ) ;
#26644 = CARTESIAN_POINT ( 'NONE',  ( 5.999999999999949374, 1.607695154586804565, -78.59668783648706381 ) ) ;
#26645 = VERTEX_POINT ( 'NONE', #19736 ) ;
#26646 = CARTESIAN_POINT ( 'NONE',  ( 159.4687500000000568, -2.485281374238585972, 6.000000000000005329 ) ) ;
#26647 = DIRECTION ( 'NONE',  ( 1.000000000000000000, -5.551115123125773458E-17, -1.260129944081490338E-35 ) ) ;
#26648 = CARTESIAN_POINT ( 'NONE',  ( 120.9377832217621034, -1.849990392679562001, -0.7662911109077087390 ) ) ;
#26649 = ORIENTED_EDGE ( 'NONE', *, *, #647, .F. ) ;
#26650 = CIRCLE ( 'NONE', #13474, 6.499999999999977796 ) ;
#26651 = ADVANCED_FACE ( 'NONE', ( #10383 ), #6833, .F. ) ;
#26652 = CARTESIAN_POINT ( 'NONE',  ( 3.175426480543072749, -5.500000000000105693, -105.6250000000000142 ) ) ;
#26653 = CARTESIAN_POINT ( 'NONE',  ( 18.25000000000009948, 1.873492889145123019, -1.873492889144956486 ) ) ;
#26654 = CARTESIAN_POINT ( 'NONE',  ( 5.412658773652712085, -3.125000000000086153, -125.4330127018922241 ) ) ;
#26655 = EDGE_LOOP ( 'NONE', ( #24894, #10299, #8938, #27642 ) ) ;
#26656 = CARTESIAN_POINT ( 'NONE',  ( -3.464101615137757051, -5.999999999999979572, -68.66367513459479710 ) ) ;
#26657 = CARTESIAN_POINT ( 'NONE',  ( 7.216878364870455975, -6.409875621278545621E-14, -161.9419872981077901 ) ) ;
#26658 = CARTESIAN_POINT ( 'NONE',  ( 104.6249999999999005, -1.767766952966376426, -1.767766952966320915 ) ) ;
#26659 = CARTESIAN_POINT ( 'NONE',  ( 147.2886751345948539, 5.500000000000005329, 0.000000000000000000 ) ) ;
#26660 = CARTESIAN_POINT ( 'NONE',  ( 3.608439182435180470, -6.249999999999997335, -59.55801270189223118 ) ) ;
#26661 = ORIENTED_EDGE ( 'NONE', *, *, #1921, .F. ) ;
#26662 = CARTESIAN_POINT ( 'NONE',  ( -0.06967686769852464435, -14.74880632522791579, -8.209202207805669005 ) ) ;
#26663 = CYLINDRICAL_SURFACE ( 'NONE', #24603, 2.499999999999999112 ) ;
#26664 = ADVANCED_FACE ( 'NONE', ( #3136 ), #21904, .F. ) ;
#26665 = CARTESIAN_POINT ( 'NONE',  ( -5.195867772253099481, 9.698547982442537574, -21.97454809331925318 ) ) ;
#26666 = CARTESIAN_POINT ( 'NONE',  ( 118.9613248654051318, 5.551115123125782702E-14, 2.000000000000001776 ) ) ;
#26667 = CARTESIAN_POINT ( 'NONE',  ( -3.175426480542816510, -5.500000000000057732, -170.3750000000000568 ) ) ;
#26668 = CARTESIAN_POINT ( 'NONE',  ( 118.9999999999998437, 2.500000000000057732, 2.220446049250313081E-13 ) ) ;
#26669 = CARTESIAN_POINT ( 'NONE',  ( 6.000000000000000888, -1.859271017917181981E-14, -100.5863248654052171 ) ) ;
#26670 = CARTESIAN_POINT ( 'NONE',  ( 3.608439182435180470, 6.249999999999982236, -165.5580127018922383 ) ) ;
#26671 = CARTESIAN_POINT ( 'NONE',  ( 154.9613248654052029, -5.500000000000005329, 0.000000000000000000 ) ) ;
#26672 = CARTESIAN_POINT ( 'NONE',  ( 23.56250000000009948, -1.999999999999851674, -0.8284271247462354770 ) ) ;
#26673 = CARTESIAN_POINT ( 'NONE',  ( -2.775557561562891351E-14, -5.500000000000115463, -113.2500000000000142 ) ) ;
#26674 = CARTESIAN_POINT ( 'NONE',  ( 135.0710398743875373, -7.730392528201072366, 8.358534351738736490 ) ) ;
#26675 =( BOUNDED_CURVE ( )  B_SPLINE_CURVE ( 2, ( #5489, #20098, #15678, #24391, #24535, #3482, #27141, #26822, #13366 ),
 .UNSPECIFIED., .F., .T. ) 
 B_SPLINE_CURVE_WITH_KNOTS ( ( 3, 2, 2, 2, 3 ),
 ( 0.2805555555555555580, 0.2814814814814814437, 0.2833333333333333259, 0.2851851851851852082, 0.2861111111111112049 ),
 .UNSPECIFIED. ) 
 CURVE ( )  GEOMETRIC_REPRESENTATION_ITEM ( )  RATIONAL_B_SPLINE_CURVE ( ( 0.9330127018922194093, 0.9330127018922194093, 1.000000000000000000, 0.8660254037844388186, 1.000000000000000000, 0.8660254037844388186, 1.000000000000000000, 0.9330127018922154125, 0.9330127018922194093 ) ) 
 REPRESENTATION_ITEM ( '' )  );
#26676 = CARTESIAN_POINT ( 'NONE',  ( 4.763139720814407951, 2.750000000000002665, -108.2500000000000142 ) ) ;
#26677 = CARTESIAN_POINT ( 'NONE',  ( 16.39882486540525264, -1.035533905932749299, -2.499999999999964473 ) ) ;
#26678 = VERTEX_POINT ( 'NONE', #20047 ) ;
#26679 = CARTESIAN_POINT ( 'NONE',  ( 16.31250000000002487, -1.097466725451379244, -2.649519052838419153 ) ) ;
#26680 = CARTESIAN_POINT ( 'NONE',  ( 120.1249999999998295, 1.767766952966348670, 1.767766952966431937 ) ) ;
#26681 = DIRECTION ( 'NONE',  ( -1.000000000000000000, 3.469446951953694061E-16, 0.000000000000000000 ) ) ;
#26682 = ORIENTED_EDGE ( 'NONE', *, *, #23823, .F. ) ;
#26683 = CARTESIAN_POINT ( 'NONE',  ( 5.196152422706629359, 3.000000000000002665, -65.96132486540523132 ) ) ;
#26684 = CARTESIAN_POINT ( 'NONE',  ( -3.608439182435115633, 6.249999999999965361, -81.94198729810779014 ) ) ;
#26685 = SURFACE_SIDE_STYLE ('',( #28846 ) ) ;
#26686 = VERTEX_POINT ( 'NONE', #25232 ) ;
#26687 = CARTESIAN_POINT ( 'NONE',  ( 0.000000000000000000, 0.000000000000000000, 0.000000000000000000 ) ) ;
#26688 = ORIENTED_EDGE ( 'NONE', *, *, #11549, .F. ) ;
#26689 = ORIENTED_EDGE ( 'NONE', *, *, #15571, .T. ) ;
#26690 = CARTESIAN_POINT ( 'NONE',  ( 132.7648502691896510, 3.535533905932725318, 3.535533905932752852 ) ) ;
#26691 = ADVANCED_FACE ( 'NONE', ( #24940 ), #29398, .F. ) ;
#26692 = ORIENTED_EDGE ( 'NONE', *, *, #14228, .F. ) ;
#26693 = CARTESIAN_POINT ( 'NONE',  ( -7.216878364870328078, 0.000000000000000000, -129.6919872981078186 ) ) ;
#26694 = CARTESIAN_POINT ( 'NONE',  ( -5.999999999999963585, 8.134310703387671600E-14, -135.8363248654052597 ) ) ;
#26695 = CARTESIAN_POINT ( 'NONE',  ( 6.000000000000000888, -6.507448562710137091E-15, -175.5863248654052029 ) ) ;
#26696 = ORIENTED_EDGE ( 'NONE', *, *, #14755, .T. ) ;
#26697 = CARTESIAN_POINT ( 'NONE',  ( 14.87500000000011013, 1.414213562373201061, -1.414213562373090038 ) ) ;
#26698 = EDGE_CURVE ( 'NONE', #28026, #16343, #1134, .T. ) ;
#26699 = LINE ( 'NONE', #7975, #23548 ) ;
#26700 = CARTESIAN_POINT ( 'NONE',  ( 0.000000000000000000, 0.000000000000000000, 0.000000000000000000 ) ) ;
#26701 = CARTESIAN_POINT ( 'NONE',  ( 134.6101497308104342, 3.535533905932725318, 3.535533905932725318 ) ) ;
#26702 = CARTESIAN_POINT ( 'NONE',  ( -6.000000000000007105, -1.607695154586655129, -47.26933756729744829 ) ) ;
#26703 = CARTESIAN_POINT ( 'NONE',  ( 2.775557561562891351E-14, -6.250000000000061284, -66.31698729810780435 ) ) ;
#26704 = CARTESIAN_POINT ( 'NONE',  ( 7.216878364870455975, -6.409875621278545621E-14, -56.94198729810781145 ) ) ;
#26705 = CARTESIAN_POINT ( 'NONE',  ( 5.196152422706629359, -2.999999999999988898, -128.2886751345948539 ) ) ;
#26706 = CARTESIAN_POINT ( 'NONE',  ( 108.1874999999998721, 1.035533905932719101, 2.500000000000205169 ) ) ;
#26707 = PLANE ( 'NONE',  #6882 ) ;
#26708 = CARTESIAN_POINT ( 'NONE',  ( -3.175426480542816510, -5.500000000000057732, -126.8749999999999858 ) ) ;
#26709 = CARTESIAN_POINT ( 'NONE',  ( 1.000000000000000888, -15.13479642978409245, -8.789606617933440447 ) ) ;
#26710 = CARTESIAN_POINT ( 'NONE',  ( 104.7401757384973848, 1.616881886637318688, -0.9308393922784925500 ) ) ;
#26711 = EDGE_LOOP ( 'NONE', ( #16595, #20161, #15133, #24307, #14880, #27493, #25613, #12771, #16418, #24204, #5569, #3914, #28033, #6623, #12483, #29260 ) ) ;
#26712 = LINE ( 'NONE', #26574, #2829 ) ;
#26713 = CIRCLE ( 'NONE', #28191, 17.50000000000000355 ) ;
#26714 = DIRECTION ( 'NONE',  ( 0.000000000000000000, 0.000000000000000000, -1.000000000000000000 ) ) ;
#26715 = CARTESIAN_POINT ( 'NONE',  ( 6.000000000000000888, -1.859271017917181981E-14, -159.6636751345948539 ) ) ;
#26716 = CARTESIAN_POINT ( 'NONE',  ( -5.999999999999963585, 1.780251999655701777E-13, -89.33632486540523132 ) ) ;
#26717 = CARTESIAN_POINT ( 'NONE',  ( 104.9868134515153031, -0.6968434951807797040, -1.879196483909238102 ) ) ;
#26718 = ORIENTED_EDGE ( 'NONE', *, *, #20813, .F. ) ;
#26719 = CARTESIAN_POINT ( 'NONE',  ( 118.6011751345946550, -0.8284271247461453269, 2.000000000000332179 ) ) ;
#26720 =( BOUNDED_CURVE ( )  B_SPLINE_CURVE ( 2, ( #22166, #16830, #14957, #5099, #5402, #14525, #23864, #24009, #2804 ),
 .UNSPECIFIED., .F., .F. ) 
 B_SPLINE_CURVE_WITH_KNOTS ( ( 3, 2, 2, 2, 3 ),
 ( 0.7638888888888888395, 0.7648148148148148362, 0.7666666666666666075, 0.7685185185185184897, 0.7694444444444443754 ),
 .UNSPECIFIED. ) 
 CURVE ( )  GEOMETRIC_REPRESENTATION_ITEM ( )  RATIONAL_B_SPLINE_CURVE ( ( 0.9330127018922194093, 0.9330127018922154125, 1.000000000000000000, 0.8660254037844388186, 1.000000000000000000, 0.8660254037844388186, 1.000000000000000000, 0.9330127018922234061, 0.9330127018922194093 ) ) 
 REPRESENTATION_ITEM ( '' )  );
#26721 = CARTESIAN_POINT ( 'NONE',  ( 3.608439182435180470, 6.249999999999982236, -92.69198729810779014 ) ) ;
#26722 = SURFACE_STYLE_USAGE ( .BOTH. , #12509 ) ;
#26723 = CARTESIAN_POINT ( 'NONE',  ( 155.3511751345948539, -3.889087296526011706, 3.889087296526011706 ) ) ;
#26724 = CARTESIAN_POINT ( 'NONE',  ( 113.0624999999997726, 2.500000000000084821, 1.035533905932989551 ) ) ;
#26725 = CARTESIAN_POINT ( 'NONE',  ( 140.0000000000000284, -11.48545691804907420, 4.867024281885878878 ) ) ;
#26726 = ORIENTED_EDGE ( 'NONE', *, *, #30256, .F. ) ;
#26727 = CARTESIAN_POINT ( 'NONE',  ( 141.0000000000000284, -12.00000000000001066, 4.000000000000003553 ) ) ;
#26728 = ADVANCED_FACE ( 'NONE', ( #10534 ), #29393, .T. ) ;
#26729 = ORIENTED_EDGE ( 'NONE', *, *, #13761, .T. ) ;
#26730 = CARTESIAN_POINT ( 'NONE',  ( 18.66367513459488237, -1.767766952966154381, 1.767766952966320915 ) ) ;
#26731 = CARTESIAN_POINT ( 'NONE',  ( -4.763139720814407951, 2.749999999999946709, -61.25000000000002842 ) ) ;
#26732 = CARTESIAN_POINT ( 'NONE',  ( 0.000000000000000000, 5.999999999999977796, -69.28867513459479710 ) ) ;
#26733 = CARTESIAN_POINT ( 'NONE',  ( 3.464101615137757051, -5.999999999999979572, -134.4136751345947971 ) ) ;
#26734 = EDGE_CURVE ( 'NONE', #1194, #305, #9434, .T. ) ;
#26735 = CARTESIAN_POINT ( 'NONE',  ( 2.775557561562891351E-14, -6.250000000000061284, -79.18301270189220986 ) ) ;
#26736 = CARTESIAN_POINT ( 'NONE',  ( 157.3913997308104058, -2.071067811865468400, 4.999999999999989342 ) ) ;
#26737 = CARTESIAN_POINT ( 'NONE',  ( 6.000000000000000888, -1.607695154586752384, -168.1533121635130215 ) ) ;
#26738 = DIRECTION ( 'NONE',  ( 1.000000000000000000, -0.000000000000000000, -0.000000000000000000 ) ) ;
#26739 = CARTESIAN_POINT ( 'NONE',  ( 0.000000000000000000, -5.999999999999991118, -94.03867513459485394 ) ) ;
#26740 = CARTESIAN_POINT ( 'NONE',  ( 4.763139720814407951, 2.750000000000002665, -132.2500000000000284 ) ) ;
#26741 = VECTOR ( 'NONE', #19929, 1000.000000000000000 ) ;
#26742 = CARTESIAN_POINT ( 'NONE',  ( 6.000000000000000888, 1.743066579297358182E-13, -74.16367513459482552 ) ) ;
#26743 = CARTESIAN_POINT ( 'NONE',  ( 10.01999883338032937, -0.3094390903222259404, -2.500000000000104361 ) ) ;
#26744 = FACE_OUTER_BOUND ( 'NONE', #18742, .T. ) ;
#26745 = CARTESIAN_POINT ( 'NONE',  ( 4.763139720814407951, -2.749999999999988454, -69.50000000000000000 ) ) ;
#26746 = CARTESIAN_POINT ( 'NONE',  ( -6.350852961085760029, -1.281975124255709124E-13, -55.12500000000003553 ) ) ;
#26747 = ORIENTED_EDGE ( 'NONE', *, *, #19463, .T. ) ;
#26748 = CARTESIAN_POINT ( 'NONE',  ( 154.5000000000000284, 6.000000000000005329, 0.000000000000000000 ) ) ;
#26749 = CARTESIAN_POINT ( 'NONE',  ( 142.2261751345948539, -3.889087296526011706, -3.889087296526011706 ) ) ;
#26750 = CARTESIAN_POINT ( 'NONE',  ( 14.12500000000013678, 1.414213562373201061, 1.414213562373034527 ) ) ;
#26751 = AXIS2_PLACEMENT_3D ( 'NONE', #12680, #28904, #3406 ) ;
#26752 = CARTESIAN_POINT ( 'NONE',  ( 114.8988248654050182, 0.8284271247462955401, 2.000000000000212275 ) ) ;
#26753 = CARTESIAN_POINT ( 'NONE',  ( 111.4997167782375413, 1.308140751793696044, -1.308140751793640533 ) ) ;
#26754 = EDGE_LOOP ( 'NONE', ( #11857, #5835, #4158, #7989 ) ) ;
#26755 = CARTESIAN_POINT ( 'NONE',  ( 144.5625000000000284, -4.242640687119298093, 4.242640687119298093 ) ) ;
#26756 = DIRECTION ( 'NONE',  ( 0.000000000000000000, -1.000000000000000000, -8.881784197001262184E-16 ) ) ;
#26757 = ADVANCED_FACE ( 'NONE', ( #17771 ), #22353, .T. ) ;
#26758 = EDGE_CURVE ( 'NONE', #11212, #18409, #13164, .T. ) ;
#26759 = CARTESIAN_POINT ( 'NONE',  ( 4.763139720814407951, 2.750000000000002665, -145.7500000000000568 ) ) ;
#26760 =( BOUNDED_CURVE ( )  B_SPLINE_CURVE ( 2, ( #24483, #1606, #6214, #11010, #20355, #17927, #10860, #15632, #29235 ),
 .UNSPECIFIED., .F., .T. ) 
 B_SPLINE_CURVE_WITH_KNOTS ( ( 3, 2, 2, 2, 3 ),
 ( 0.4218750000000000000, 0.4296875000000000000, 0.4375000000000000000, 0.4453125000000000000, 0.4531250000000000000 ),
 .UNSPECIFIED. ) 
 CURVE ( )  GEOMETRIC_REPRESENTATION_ITEM ( )  RATIONAL_B_SPLINE_CURVE ( ( 1.000000000000000000, 0.9238795325112867385, 1.000000000000000000, 0.9238795325112867385, 1.000000000000000000, 0.9238795325112867385, 1.000000000000000000, 0.9238795325112867385, 1.000000000000000000 ) ) 
 REPRESENTATION_ITEM ( '' )  );
#26761 = CARTESIAN_POINT ( 'NONE',  ( 4.763139720814407951, 2.750000000000002665, -180.2500000000000284 ) ) ;
#26762 = CARTESIAN_POINT ( 'NONE',  ( 16.68750000000013856, -0.8284271247461753029, -2.000000000000151879 ) ) ;
#26763 = VERTEX_POINT ( 'NONE', #18220 ) ;
#26764 = CARTESIAN_POINT ( 'NONE',  ( 5.412658773652739619, 3.124999999999988898, -145.3169872981078186 ) ) ;
#26765 = CARTESIAN_POINT ( 'NONE',  ( 4.763139720814407951, -2.749999999999988454, -78.50000000000001421 ) ) ;
#26766 = CARTESIAN_POINT ( 'NONE',  ( 13.87500000000008171, -2.649519052838111843, 0.000000000000000000 ) ) ;
#26767 = CARTESIAN_POINT ( 'NONE',  ( 3.608439182435180470, 6.249999999999982236, -95.05801270189226670 ) ) ;
#26768 = CARTESIAN_POINT ( 'NONE',  ( -3.175426480542816510, 5.499999999999865885, -152.8749999999999716 ) ) ;
#26769 = LINE ( 'NONE', #834, #15807 ) ;
#26770 = CARTESIAN_POINT ( 'NONE',  ( -5.196152422706573404, -3.000000000000002665, -96.71132486540523132 ) ) ;
#26771 = CARTESIAN_POINT ( 'NONE',  ( 5.196152422706629359, -2.999999999999988898, -150.7886751345948255 ) ) ;
#26772 = CARTESIAN_POINT ( 'NONE',  ( 5.196152422706629359, -2.999999999999988898, -90.78867513459488237 ) ) ;
#26773 = CARTESIAN_POINT ( 'NONE',  ( 134.9985123063161723, -7.386692690774673054, 8.423607852766412663 ) ) ;
#26774 = FILL_AREA_STYLE ('',( #12862 ) ) ;
#26775 = CARTESIAN_POINT ( 'NONE',  ( -4.763139720814407951, 2.749999999999946709, -157.2500000000000000 ) ) ;
#26776 = CARTESIAN_POINT ( 'NONE',  ( 19.03867513459492500, 1.110223024625156540E-13, -2.500000000000057732 ) ) ;
#26777 = CARTESIAN_POINT ( 'NONE',  ( -6.350852961085760029, -1.281975124255709124E-13, -148.1250000000000284 ) ) ;
#26778 = DIRECTION ( 'NONE',  ( 1.000000000000000000, 0.000000000000000000, 0.000000000000000000 ) ) ;
#26779 = CARTESIAN_POINT ( 'NONE',  ( 0.000000000000000000, 5.499999999999991118, -94.50000000000002842 ) ) ;
#26780 = FACE_OUTER_BOUND ( 'NONE', #1810, .T. ) ;
#26781 = CARTESIAN_POINT ( 'NONE',  ( 6.350852961086080661, -9.614813431917819062E-14, -84.37500000000005684 ) ) ;
#26782 = CARTESIAN_POINT ( 'NONE',  ( 152.1711002691896226, 4.999999999999989342, 2.071067811865468400 ) ) ;
#26783 = CARTESIAN_POINT ( 'NONE',  ( 152.1636751345948255, 0.000000000000000000, 5.500000000000005329 ) ) ;
#26784 = VECTOR ( 'NONE', #23712, 1000.000000000000000 ) ;
#26785 = AXIS2_PLACEMENT_3D ( 'NONE', #15909, #25206, #15595 ) ;
#26786 = CARTESIAN_POINT ( 'NONE',  ( 21.43750000000007105, -1.999999999999911626, 0.8284271247461753029 ) ) ;
#26787 = CARTESIAN_POINT ( 'NONE',  ( -5.999999999999963585, -1.487416814333745711E-14, -124.4136751345948255 ) ) ;
#26788 = CARTESIAN_POINT ( 'NONE',  ( -4.999999999999886313, -9.000000000000007105, 5.000000000000004441 ) ) ;
#26789 = CARTESIAN_POINT ( 'NONE',  ( 0.000000000000000000, 0.000000000000000000, 0.000000000000000000 ) ) ;
#26790 = VERTEX_POINT ( 'NONE', #6514 ) ;
#26791 =( LENGTH_UNIT ( ) NAMED_UNIT ( * ) SI_UNIT ( .MILLI., .METRE. ) );
#26792 = CARTESIAN_POINT ( 'NONE',  ( -5.999999999999962697, 3.323446944526963891E-14, -157.4136751345948539 ) ) ;
#26793 = CARTESIAN_POINT ( 'NONE',  ( 109.7886751345948255, -2.000000000000001776, 0.000000000000000000 ) ) ;
#26794 = CARTESIAN_POINT ( 'NONE',  ( 24.97285668889470855, 1.969969495779358759, -0.5495425123464061645 ) ) ;
#26795 = VERTEX_POINT ( 'NONE', #24640 ) ;
#26796 = EDGE_CURVE ( 'NONE', #23369, #10419, #13015, .T. ) ;
#26797 = EDGE_LOOP ( 'NONE', ( #7654, #27946, #22838, #5804 ) ) ;
#26798 = CARTESIAN_POINT ( 'NONE',  ( -3.175426480542816510, 5.499999999999865885, -109.3750000000000284 ) ) ;
#26799 =( GEOMETRIC_REPRESENTATION_CONTEXT ( 3 ) GLOBAL_UNCERTAINTY_ASSIGNED_CONTEXT ( ( #2975 ) ) GLOBAL_UNIT_ASSIGNED_CONTEXT ( ( #20026, #6036, #1269 ) ) REPRESENTATION_CONTEXT ( 'NONE', 'WORKASPACE' ) );
#26800 = CIRCLE ( 'NONE', #12174, 0.5000000000000000000 ) ;
#26801 = CARTESIAN_POINT ( 'NONE',  ( -7.216878364870328078, 0.000000000000000000, -112.5580127018922241 ) ) ;
#26802 = ORIENTED_EDGE ( 'NONE', *, *, #9187, .T. ) ;
#26803 = CARTESIAN_POINT ( 'NONE',  ( -7.216878364870328078, 0.000000000000000000, -156.6919872981078186 ) ) ;
#26804 = CYLINDRICAL_SURFACE ( 'NONE', #2942, 5.500000000000000000 ) ;
#26805 = CARTESIAN_POINT ( 'NONE',  ( 147.5699251345948255, 2.278174593052259667, 5.499999999999763745 ) ) ;
#26806 = CARTESIAN_POINT ( 'NONE',  ( -3.608439182435115633, 6.249999999999965361, -54.30801270189220276 ) ) ;
#26807 = ORIENTED_EDGE ( 'NONE', *, *, #12812, .T. ) ;
#26808 = CYLINDRICAL_SURFACE ( 'NONE', #1453, 6.000000000000000888 ) ;
#26809 = CARTESIAN_POINT ( 'NONE',  ( -5.999999999999963585, 8.134310703387671600E-14, -119.9136751345948397 ) ) ;
#26810 = CARTESIAN_POINT ( 'NONE',  ( 6.000000000000052403, -1.607695154586662678, -166.6533121635129646 ) ) ;
#26811 = EDGE_CURVE ( 'NONE', #84, #19051, #25857, .T. ) ;
#26812 = CARTESIAN_POINT ( 'NONE',  ( 0.000000000000000000, 0.000000000000000000, 0.000000000000000000 ) ) ;
#26813 = CIRCLE ( 'NONE', #348, 0.5000000000000004441 ) ;
#26814 = CARTESIAN_POINT ( 'NONE',  ( -3.175426480542816510, -5.500000000000057732, -168.8750000000000568 ) ) ;
#26815 = CARTESIAN_POINT ( 'NONE',  ( 118.3124999999997726, -1.035533905932598975, 2.500000000000205169 ) ) ;
#26816 = CARTESIAN_POINT ( 'NONE',  ( -7.216878364870328078, 0.000000000000000000, -172.5580127018922383 ) ) ;
#26817 = CARTESIAN_POINT ( 'NONE',  ( 140.5000000000000284, -9.599999999999997868, 7.200000000000011724 ) ) ;
#26818 = CARTESIAN_POINT ( 'NONE',  ( 23.93750000000006750, 2.000000000000151879, -0.8284271247462955401 ) ) ;
#26819 = CARTESIAN_POINT ( 'NONE',  ( -4.763139720814407951, -2.750000000000016431, -116.5000000000000426 ) ) ;
#26820 = CARTESIAN_POINT ( 'NONE',  ( 3.175426480543072749, 5.499999999999865885, -102.1250000000000142 ) ) ;
#26821 = PLANE ( 'NONE',  #10125 ) ;
#26822 = CARTESIAN_POINT ( 'NONE',  ( -6.000000000000007105, -1.607695154586655129, -84.76933756729746960 ) ) ;
#26823 = ORIENTED_EDGE ( 'NONE', *, *, #12886, .F. ) ;
#26824 = ADVANCED_FACE ( 'NONE', ( #1603 ), #16918, .T. ) ;
#26825 = CARTESIAN_POINT ( 'NONE',  ( 119.1874999999998153, 1.035533905932779275, 2.500000000000205169 ) ) ;
#26826 = DIRECTION ( 'NONE',  ( -7.147005652999508048E-36, 5.642372883946980038E-36, 1.000000000000000000 ) ) ;
#26827 = AXIS2_PLACEMENT_3D ( 'NONE', #25956, #23672, #7072 ) ;
#26828 = FACE_OUTER_BOUND ( 'NONE', #12919, .T. ) ;
#26829 = ORIENTED_EDGE ( 'NONE', *, *, #13949, .F. ) ;
#26830 = CARTESIAN_POINT ( 'NONE',  ( 6.350852961086080661, -9.614813431917819062E-14, -159.3750000000000284 ) ) ;
#26831 = CARTESIAN_POINT ( 'NONE',  ( 139.3988248654052313, 3.889087296526011706, 3.889087296526011706 ) ) ;
#26832 = CARTESIAN_POINT ( 'NONE',  ( 7.216878364870455975, -6.409875621278545621E-14, -82.44198729810780435 ) ) ;
#26833 = DIRECTION ( 'NONE',  ( 0.000000000000000000, 1.776356839400250465E-15, -1.000000000000000000 ) ) ;
#26834 = VERTEX_POINT ( 'NONE', #8229 ) ;
#26835 = CYLINDRICAL_SURFACE ( 'NONE', #5160, 6.000000000000000888 ) ;
#26836 = EDGE_CURVE ( 'NONE', #21222, #956, #22083, .T. ) ;
#26837 = AXIS2_PLACEMENT_3D ( 'NONE', #5482, #19498, #3180 ) ;
#26838 = ORIENTED_EDGE ( 'NONE', *, *, #22049, .F. ) ;
#26839 = ORIENTED_EDGE ( 'NONE', *, *, #6477, .F. ) ;
#26840 = CARTESIAN_POINT ( 'NONE',  ( 134.7336002691896795, -4.999999999999989342, 2.071067811865468400 ) ) ;
#26841 = CARTESIAN_POINT ( 'NONE',  ( -3.608439182435115633, 6.249999999999965361, -136.8080127018922667 ) ) ;
#26842 = ORIENTED_EDGE ( 'NONE', *, *, #23986, .T. ) ;
#26843 = CARTESIAN_POINT ( 'NONE',  ( 157.4925748654052313, 2.278174593051919494, 5.500000000000105693 ) ) ;
#26844 = CARTESIAN_POINT ( 'NONE',  ( 3.608439182435180470, -6.249999999999997335, -130.6919872981078470 ) ) ;
#26845 = FACE_OUTER_BOUND ( 'NONE', #29272, .T. ) ;
#26846 = CARTESIAN_POINT ( 'NONE',  ( -4.763139720814407951, 2.749999999999946709, -173.7500000000000284 ) ) ;
#26847 = CARTESIAN_POINT ( 'NONE',  ( -5.999999999999963585, 1.780251999655701777E-13, -49.41367513459484684 ) ) ;
#26848 = DIRECTION ( 'NONE',  ( -1.000000000000000000, -1.665334536937736783E-16, -2.220446049250315546E-16 ) ) ;
#26849 = EDGE_LOOP ( 'NONE', ( #7033, #23565, #12939, #12003, #21739, #9923, #14791, #26914, #6877, #3235, #19297, #9761 ) ) ;
#26850 = AXIS2_PLACEMENT_3D ( 'NONE', #18088, #29717, #17628 ) ;
#26851 = CARTESIAN_POINT ( 'NONE',  ( 15.56250000000003375, -1.999999999999851674, -0.8284271247462354770 ) ) ;
#26852 = FACE_OUTER_BOUND ( 'NONE', #23605, .T. ) ;
#26853 =( BOUNDED_CURVE ( )  B_SPLINE_CURVE ( 2, ( #17296, #6040, #15135, #24621, #12696, #3268, #24928, #3729, #5571 ),
 .UNSPECIFIED., .F., .T. ) 
 B_SPLINE_CURVE_WITH_KNOTS ( ( 3, 2, 2, 2, 3 ),
 ( 0.6125000000000010436, 0.6187500000000007994, 0.6250000000000006661, 0.6312500000000004219, 0.6375000000000001776 ),
 .UNSPECIFIED. ) 
 CURVE ( )  GEOMETRIC_REPRESENTATION_ITEM ( )  RATIONAL_B_SPLINE_CURVE ( ( 0.9999999999999877875, 0.9238795325112989509, 1.000000000000000000, 0.9238795325112867385, 1.000000000000000000, 0.9238795325112867385, 1.000000000000000000, 0.9238795325112840739, 1.000000000000002665 ) ) 
 REPRESENTATION_ITEM ( '' )  );
#26854 = AXIS2_PLACEMENT_3D ( 'NONE', #7091, #16508, #21391 ) ;
#26855 = CARTESIAN_POINT ( 'NONE',  ( -5.196152422706601826, 2.999999999999975131, -90.03867513459485394 ) ) ;
#26856 = CARTESIAN_POINT ( 'NONE',  ( 0.000000000000000000, -5.999999999999991118, -107.5386751345948113 ) ) ;
#26857 = CARTESIAN_POINT ( 'NONE',  ( -3.608439182435052128, -6.250000000000110134, -67.94198729810780435 ) ) ;
#26858 = CARTESIAN_POINT ( 'NONE',  ( 5.412658773652739619, 3.124999999999988898, -53.81698729810779724 ) ) ;
#26859 = FACE_OUTER_BOUND ( 'NONE', #28658, .T. ) ;
#26860 = SURFACE_SIDE_STYLE ('',( #17243 ) ) ;
#26861 = CARTESIAN_POINT ( 'NONE',  ( 119.9999999999997868, 1.752251084791750291, -1.505035388676465580 ) ) ;
#26862 = CARTESIAN_POINT ( 'NONE',  ( 107.5863248654051318, 1.414213562373145550, -1.414213562373145550 ) ) ;
#26863 = CARTESIAN_POINT ( 'NONE',  ( -3.175426480542816510, -5.500000000000057732, -128.3750000000000000 ) ) ;
#26864 = CARTESIAN_POINT ( 'NONE',  ( 6.000000000000000888, 1.607695154586715303, -167.0966878364870354 ) ) ;
#26865 = EDGE_CURVE ( 'NONE', #29031, #3651, #17118, .T. ) ;
#26866 = VERTEX_POINT ( 'NONE', #22384 ) ;
#26867 = CARTESIAN_POINT ( 'NONE',  ( 5.196152422706629359, -2.999999999999988898, -118.7113248654052597 ) ) ;
#26868 = EDGE_CURVE ( 'NONE', #11262, #3485, #7778, .T. ) ;
#26869 = CARTESIAN_POINT ( 'NONE',  ( 17.66367513459490723, -1.767766952966320915, 1.767766952966431937 ) ) ;
#26870 = CARTESIAN_POINT ( 'NONE',  ( 16.89882486540530593, 1.035533905932869425, 2.499999999999904521 ) ) ;
#26871 = CARTESIAN_POINT ( 'NONE',  ( -6.000000000000000888, 1.067854986875958443E-15, 7.560779664488942560E-35 ) ) ;
#26872 = CARTESIAN_POINT ( 'NONE',  ( 6.000000000000000000, 2.951592740943527306E-14, -161.1636751345949108 ) ) ;
#26873 = ORIENTED_EDGE ( 'NONE', *, *, #19855, .T. ) ;
#26874 = CARTESIAN_POINT ( 'NONE',  ( 112.0622167782374277, -1.849990392679472073, 0.7662911109078888172 ) ) ;
#26875 = FACE_OUTER_BOUND ( 'NONE', #1658, .T. ) ;
#26876 = CARTESIAN_POINT ( 'NONE',  ( 10.87499999999996803, 1.414213562373312083, -1.414213562373145550 ) ) ;
#26877 = CARTESIAN_POINT ( 'NONE',  ( 3.608439182435180470, 6.249999999999982236, -98.69198729810781856 ) ) ;
#26878 = CARTESIAN_POINT ( 'NONE',  ( -5.999999999999956479, -1.607695154586745057, -54.76933756729744829 ) ) ;
#26879 = ADVANCED_FACE ( 'NONE', ( #26373 ), #2926, .T. ) ;
#26880 = CARTESIAN_POINT ( 'NONE',  ( 158.1636751345948255, 0.000000000000000000, 5.500000000000005329 ) ) ;
#26881 = CARTESIAN_POINT ( 'NONE',  ( 114.5624999999997442, -2.499999999999934719, -1.035533905932448873 ) ) ;
#26882 = LINE ( 'NONE', #24143, #20872 ) ;
#26883 = ORIENTED_EDGE ( 'NONE', *, *, #20517, .T. ) ;
#26884 = CARTESIAN_POINT ( 'NONE',  ( 24.81250000000011724, -2.649519052838298805, 1.097466725451559322 ) ) ;
#26885 = CARTESIAN_POINT ( 'NONE',  ( 160.9318293186996414, -11.54853638030490259, 3.263004215147740084 ) ) ;
#26886 = CARTESIAN_POINT ( 'NONE',  ( 0.000000000000000000, 5.499999999999991118, -46.49999999999998579 ) ) ;
#26887 = CARTESIAN_POINT ( 'NONE',  ( -5.999999999999956479, -1.607695154586745057, -59.84668783648706381 ) ) ;
#26888 = CARTESIAN_POINT ( 'NONE',  ( 2.775557561562891351E-14, 6.250000000000033751, -73.93301270189223828 ) ) ;
#26889 = CARTESIAN_POINT ( 'NONE',  ( 6.000000000000000888, -1.859271017917181981E-14, -172.5863248654052029 ) ) ;
#26890 = CARTESIAN_POINT ( 'NONE',  ( 148.7663997308104058, -4.999999999999989342, -2.071067811865468400 ) ) ;
#26891 = FACE_OUTER_BOUND ( 'NONE', #15207, .T. ) ;
#26892 = CARTESIAN_POINT ( 'NONE',  ( -1.285375204280330350E-15, -10.49588505988223375, 1.184433945098074864E-34 ) ) ;
#26893 = CARTESIAN_POINT ( 'NONE',  ( 5.196152422706629359, -2.999999999999988898, -152.2886751345948255 ) ) ;
#26894 = FACE_OUTER_BOUND ( 'NONE', #26797, .T. ) ;
#26895 = CARTESIAN_POINT ( 'NONE',  ( -4.763139720814407951, -2.750000000000016431, -133.0000000000000000 ) ) ;
#26896 = MECHANICAL_DESIGN_GEOMETRIC_PRESENTATION_REPRESENTATION (  '', ( #2465 ), #4352 ) ;
#26897 = DIRECTION ( 'NONE',  ( 1.000000000000000000, 0.000000000000000000, 0.000000000000000000 ) ) ;
#26898 = CARTESIAN_POINT ( 'NONE',  ( 5.412658773652712085, -3.125000000000086153, -147.9330127018922383 ) ) ;
#26899 = CARTESIAN_POINT ( 'NONE',  ( 0.000000000000000000, 5.999999999999977796, -158.7113248654052313 ) ) ;
#26900 = EDGE_CURVE ( 'NONE', #24100, #21920, #5373, .T. ) ;
#26901 = CARTESIAN_POINT ( 'NONE',  ( 0.000000000000000000, 5.499999999999991118, -61.50000000000000000 ) ) ;
#26902 = CARTESIAN_POINT ( 'NONE',  ( 4.763139720814407951, 2.750000000000002665, -60.25000000000002842 ) ) ;
#26903 = CARTESIAN_POINT ( 'NONE',  ( 137.1636751345948255, 0.000000000000000000, 5.500000000000005329 ) ) ;
#26904 = ORIENTED_EDGE ( 'NONE', *, *, #1371, .F. ) ;
#26905 = CARTESIAN_POINT ( 'NONE',  ( 144.4687500000000568, -2.485281374238585972, 6.000000000000005329 ) ) ;
#26906 = CARTESIAN_POINT ( 'NONE',  ( 141.9449251345948255, -5.500000000000012434, 2.278174593052012309 ) ) ;
#26907 = CARTESIAN_POINT ( 'NONE',  ( 5.196152422706629359, -2.999999999999988898, -98.28867513459482552 ) ) ;
#26908 = CARTESIAN_POINT ( 'NONE',  ( 110.9997167782376266, -1.308140751793585022, 1.308140751793640533 ) ) ;
#26909 = EDGE_CURVE ( 'NONE', #3013, #23373, #8073, .T. ) ;
#26910 = ADVANCED_FACE ( 'NONE', ( #17492 ), #26804, .F. ) ;
#26911 = ORIENTED_EDGE ( 'NONE', *, *, #26330, .F. ) ;
#26912 = CARTESIAN_POINT ( 'NONE',  ( 143.8125000000000284, 4.242640687119298093, -4.242640687119298093 ) ) ;
#26913 = CARTESIAN_POINT ( 'NONE',  ( 161.1118616798009953, -0.3161702963393516752, 5.611861679801007696 ) ) ;
#26914 = ORIENTED_EDGE ( 'NONE', *, *, #27125, .T. ) ;
#26915 = VECTOR ( 'NONE', #2651, 1000.000000000000000 ) ;
#26916 = CARTESIAN_POINT ( 'NONE',  ( -3.175426480542816510, 5.499999999999865885, -142.3750000000000568 ) ) ;
#26917 = AXIS2_PLACEMENT_3D ( 'NONE', #24266, #917, #12796 ) ;
#26918 = CARTESIAN_POINT ( 'NONE',  ( -3.608439182435115633, 6.249999999999965361, -48.94198729810783988 ) ) ;
#26919 = CARTESIAN_POINT ( 'NONE',  ( 16.12500000000002842, 1.414213562373201061, 1.414213562373034527 ) ) ;
#26920 = ORIENTED_EDGE ( 'NONE', *, *, #26299, .T. ) ;
#26921 = CARTESIAN_POINT ( 'NONE',  ( 3.608439182435180470, -6.249999999999997335, -148.6919872981078186 ) ) ;
#26922 = CARTESIAN_POINT ( 'NONE',  ( 4.763139720814407951, 2.750000000000002665, -72.25000000000004263 ) ) ;
#26923 = CARTESIAN_POINT ( 'NONE',  ( 2.775557561562891351E-14, 6.250000000000033751, -96.43301270189225249 ) ) ;
#26924 = EDGE_LOOP ( 'NONE', ( #5878, #23936, #10174, #28805 ) ) ;
#26925 = DIRECTION ( 'NONE',  ( -1.000000000000000000, -1.665334536937731113E-16, 1.526556658859586792E-16 ) ) ;
#26926 = CARTESIAN_POINT ( 'NONE',  ( 6.000000000000000888, 1.743066579297358182E-13, -96.08632486540521711 ) ) ;
#26927 = CYLINDRICAL_SURFACE ( 'NONE', #20424, 6.000000000000000888 ) ;
#26928 = CARTESIAN_POINT ( 'NONE',  ( 5.196152422706629359, 3.000000000000002665, -98.96132486540520290 ) ) ;
#26929 = CARTESIAN_POINT ( 'NONE',  ( -4.999999999999879208, -70.00000000000001421, -5.000000000000004441 ) ) ;
#26930 =( NAMED_UNIT ( * ) PLANE_ANGLE_UNIT ( ) SI_UNIT ( $, .RADIAN. ) );
#26931 = CARTESIAN_POINT ( 'NONE',  ( -6.350852961085760029, -1.281975124255709124E-13, -157.1250000000000284 ) ) ;
#26932 = DIRECTION ( 'NONE',  ( 1.000000000000000000, 0.000000000000000000, 0.000000000000000000 ) ) ;
#26933 = CARTESIAN_POINT ( 'NONE',  ( 3.175426480543072749, -5.500000000000105693, -147.6250000000000284 ) ) ;
#26934 = CARTESIAN_POINT ( 'NONE',  ( 5.999999999999949374, 1.607695154586804565, -77.09668783648706381 ) ) ;
#26935 = CARTESIAN_POINT ( 'NONE',  ( -3.464101615137757051, -5.999999999999979572, -92.66367513459478289 ) ) ;
#26936 = UNCERTAINTY_MEASURE_WITH_UNIT (LENGTH_MEASURE( 1.000000000000000082E-05 ), #17500, 'distance_accuracy_value', 'NONE');
#26937 = EDGE_CURVE ( 'NONE', #11692, #20342, #13303, .T. ) ;
#26938 = AXIS2_PLACEMENT_3D ( 'NONE', #27729, #4992, #18561 ) ;
#26939 = CARTESIAN_POINT ( 'NONE',  ( -4.763139720814407951, 2.749999999999946709, -83.74999999999998579 ) ) ;
#26940 = CARTESIAN_POINT ( 'NONE',  ( -3.175426480542816510, -5.500000000000057732, -81.87500000000004263 ) ) ;
#26941 = TOROIDAL_SURFACE ( 'NONE', #20113, 16.50000000000000355, 1.000000000000000000 ) ;
#26942 = CARTESIAN_POINT ( 'NONE',  ( 135.8363248654052029, 0.000000000000000000, -5.500000000000005329 ) ) ;
#26943 = CARTESIAN_POINT ( 'NONE',  ( 153.2023502691896510, 0.000000000000000000, -5.000000000000004441 ) ) ;
#26944 = CARTESIAN_POINT ( 'NONE',  ( -5.999999999999963585, -1.487416814333745711E-14, -105.8363248654052313 ) ) ;
#26945 = FACE_OUTER_BOUND ( 'NONE', #16317, .T. ) ;
#26946 = STYLED_ITEM ( 'NONE', ( #22395 ), #13969 ) ;
#26947 = CARTESIAN_POINT ( 'NONE',  ( 144.7425748654051461, -2.278174593052290753, -5.499999999999732658 ) ) ;
#26948 = CARTESIAN_POINT ( 'NONE',  ( 160.4136751345948824, 0.000000000000000000, -5.500000000000005329 ) ) ;
#26949 = CARTESIAN_POINT ( 'NONE',  ( 120.6247167782375413, 1.849990392679579099, 0.000000000000000000 ) ) ;
#26950 = EDGE_CURVE ( 'NONE', #22266, #2390, #9624, .T. ) ;
#26951 = CARTESIAN_POINT ( 'NONE',  ( -5.196152422706601826, 2.999999999999975131, -75.03867513459483973 ) ) ;
#26952 =( BOUNDED_CURVE ( )  B_SPLINE_CURVE ( 2, ( #5156, #12281, #19609, #21769, #28799, #10251, #19470, #28950, #22065 ),
 .UNSPECIFIED., .F., .F. ) 
 B_SPLINE_CURVE_WITH_KNOTS ( ( 3, 2, 2, 2, 3 ),
 ( 0.2027777777777777235, 0.2037037037037037202, 0.2055555555555556024, 0.2074074074074073737, 0.2083333333333333703 ),
 .UNSPECIFIED. ) 
 CURVE ( )  GEOMETRIC_REPRESENTATION_ITEM ( )  RATIONAL_B_SPLINE_CURVE ( ( 0.9330127018922194093, 0.9330127018922154125, 1.000000000000000000, 0.8660254037844388186, 1.000000000000000000, 0.8660254037844388186, 1.000000000000000000, 0.9330127018922154125, 0.9330127018922194093 ) ) 
 REPRESENTATION_ITEM ( '' )  );
#26953 = ORIENTED_EDGE ( 'NONE', *, *, #20101, .F. ) ;
#26954 = CARTESIAN_POINT ( 'NONE',  ( -5.196152422706601826, 2.999999999999975131, -72.96132486540524553 ) ) ;
#26955 = CARTESIAN_POINT ( 'NONE',  ( -6.000000000000007105, -1.607695154586655129, -79.34668783648702117 ) ) ;
#26956 = CARTESIAN_POINT ( 'NONE',  ( -5.999999999999963585, -1.487416814333745711E-14, -101.3363248654052171 ) ) ;
#26957 = ORIENTED_EDGE ( 'NONE', *, *, #15058, .T. ) ;
#26958 = EDGE_LOOP ( 'NONE', ( #26371, #24429, #5423, #20420 ) ) ;
#26959 = CARTESIAN_POINT ( 'NONE',  ( 0.000000000000000000, 5.499999999999991118, -97.50000000000002842 ) ) ;
#26960 = COLOUR_RGB ( '', 0.72549020, 0.75294118, 0.79215686) ;
#26961 = CYLINDRICAL_SURFACE ( 'NONE', #7702, 6.000000000000000888 ) ;
#26962 = CARTESIAN_POINT ( 'NONE',  ( -7.216878364870328078, 0.000000000000000000, -114.0580127018922241 ) ) ;
#26963 = ORIENTED_EDGE ( 'NONE', *, *, #270, .F. ) ;
#26964 = CARTESIAN_POINT ( 'NONE',  ( 3.464101615137852974, 5.999999999999884537, -91.91367513459485394 ) ) ;
#26965 = CARTESIAN_POINT ( 'NONE',  ( 105.9999999999998863, 2.500000000000002220, 1.110223024625156540E-13 ) ) ;
#26966 = CARTESIAN_POINT ( 'NONE',  ( 2.775557561562891351E-14, -6.250000000000061284, -55.18301270189224539 ) ) ;
#26967 = VERTEX_POINT ( 'NONE', #27566 ) ;
#26968 = CARTESIAN_POINT ( 'NONE',  ( 115.7886751345947118, -1.999999999999974021, 0.000000000000000000 ) ) ;
#26969 = CARTESIAN_POINT ( 'NONE',  ( 146.6324251345948539, -5.500000000000012434, -2.278174593052012309 ) ) ;
#26970 = CARTESIAN_POINT ( 'NONE',  ( 0.000000000000000000, 3.114577045054877854E-15, -17.50000000000000000 ) ) ;
#26971 = CARTESIAN_POINT ( 'NONE',  ( 3.175426480543072749, 5.499999999999865885, -169.6250000000000000 ) ) ;
#26972 = CARTESIAN_POINT ( 'NONE',  ( 105.4377832217621176, 1.849990392679562001, 0.7662911109078888172 ) ) ;
#26973 = CARTESIAN_POINT ( 'NONE',  ( -3.464101615137725076, 5.999999999999979572, -107.5863248654051603 ) ) ;
#26974 = CARTESIAN_POINT ( 'NONE',  ( 3.608439182435180470, -6.249999999999997335, -172.0580127018922383 ) ) ;
#26975 = CARTESIAN_POINT ( 'NONE',  ( -9.757819552369539906E-16, -10.00000000000000888, 5.000000000000004441 ) ) ;
#26976 = EDGE_CURVE ( 'NONE', #7376, #18429, #25903, .T. ) ;
#26977 = CARTESIAN_POINT ( 'NONE',  ( 4.763139720814407951, -2.749999999999988454, -114.5000000000000426 ) ) ;
#26978 = CARTESIAN_POINT ( 'NONE',  ( -4.999999999999990230, -24.99999999999999289, -5.000000000000004441 ) ) ;
#26979 = ADVANCED_FACE ( 'NONE', ( #3922, #16121 ), #20378, .F. ) ;
#26980 = CARTESIAN_POINT ( 'NONE',  ( 6.350852961086080661, -9.614813431917819062E-14, -108.3750000000000426 ) ) ;
#26981 = CARTESIAN_POINT ( 'NONE',  ( -5.196152422706573404, -3.000000000000002665, -87.71132486540523132 ) ) ;
#26982 = CARTESIAN_POINT ( 'NONE',  ( 135.0000000000000284, -8.448271545446896624, 7.965230813406249055 ) ) ;
#26983 = ORIENTED_EDGE ( 'NONE', *, *, #21062, .F. ) ;
#26984 = CARTESIAN_POINT ( 'NONE',  ( 13.31250000000006750, -1.097466725451439196, -2.649519052838419153 ) ) ;
#26985 = CYLINDRICAL_SURFACE ( 'NONE', #22152, 1.000000000000000000 ) ;
#26986 = AXIS2_PLACEMENT_3D ( 'NONE', #12778, #7816, #27162 ) ;
#26987 = DIRECTION ( 'NONE',  ( -7.147005652999508048E-36, 5.642372883946980038E-36, 1.000000000000000000 ) ) ;
#26988 = CARTESIAN_POINT ( 'NONE',  ( 110.7502832217622881, -1.308140751793585022, 1.308140751793640533 ) ) ;
#26989 = CARTESIAN_POINT ( 'NONE',  ( 107.7113248654050892, 2.000000000000057288, 0.000000000000000000 ) ) ;
#26990 = ORIENTED_EDGE ( 'NONE', *, *, #25790, .F. ) ;
#26991 = CARTESIAN_POINT ( 'NONE',  ( -6.350852961085760029, -1.281975124255709124E-13, -158.6250000000000284 ) ) ;
#26992 = CARTESIAN_POINT ( 'NONE',  ( -0.5000000000000004441, -10.50000000000000888, -8.500000000000007105 ) ) ;
#26993 = CARTESIAN_POINT ( 'NONE',  ( 3.608439182435180470, 6.249999999999982236, -82.19198729810780435 ) ) ;
#26994 = DIRECTION ( 'NONE',  ( -1.000000000000000000, -1.665334536937736783E-16, -2.220446049250315546E-16 ) ) ;
#26995 = ORIENTED_EDGE ( 'NONE', *, *, #17627, .T. ) ;
#26996 = CARTESIAN_POINT ( 'NONE',  ( 115.9613248654051603, 1.665334536937734811E-13, 2.000000000000223821 ) ) ;
#26997 = AXIS2_PLACEMENT_3D ( 'NONE', #20350, #6210, #15148 ) ;
#26998 = VERTEX_POINT ( 'NONE', #29886 ) ;
#26999 = ORIENTED_EDGE ( 'NONE', *, *, #16966, .F. ) ;
#27000 = CARTESIAN_POINT ( 'NONE',  ( 156.0937500000000000, 6.000000000000005329, 2.485281374238585972 ) ) ;
#27001 =( BOUNDED_CURVE ( )  B_SPLINE_CURVE ( 2, ( #23574, #2510, #28302, #5101, #21418, #19119, #7282, #16686, #4953 ),
 .UNSPECIFIED., .F., .F. ) 
 B_SPLINE_CURVE_WITH_KNOTS ( ( 3, 2, 2, 2, 3 ),
 ( 0.9583333333333333703, 0.9592592592592592560, 0.9611111111111111382, 0.9629629629629630205, 0.9638888888888889062 ),
 .UNSPECIFIED. ) 
 CURVE ( )  GEOMETRIC_REPRESENTATION_ITEM ( )  RATIONAL_B_SPLINE_CURVE ( ( 0.9330127018922194093, 0.9330127018922234061, 1.000000000000000000, 0.8660254037844388186, 1.000000000000000000, 0.8660254037844388186, 1.000000000000000000, 0.9330127018922194093, 0.9330127018922194093 ) ) 
 REPRESENTATION_ITEM ( '' )  );
#27002 = CARTESIAN_POINT ( 'NONE',  ( 3.175426480543072749, 5.499999999999865885, -132.1250000000000284 ) ) ;
#27003 = CARTESIAN_POINT ( 'NONE',  ( -3.608439182435115633, 6.249999999999965361, -139.8080127018922667 ) ) ;
#27004 = ORIENTED_EDGE ( 'NONE', *, *, #4385, .F. ) ;
#27005 = DIRECTION ( 'NONE',  ( -7.147005652999508048E-36, 5.642372883946980038E-36, 1.000000000000000000 ) ) ;
#27006 = CARTESIAN_POINT ( 'NONE',  ( 7.216878364870455975, -6.409875621278545621E-14, -122.9419872981078043 ) ) ;
#27007 = CYLINDRICAL_SURFACE ( 'NONE', #9851, 1.000000000000000888 ) ;
#27008 = CARTESIAN_POINT ( 'NONE',  ( 0.000000000000000000, 5.499999999999991118, -169.4999999999999716 ) ) ;
#27009 = CARTESIAN_POINT ( 'NONE',  ( 135.5000000000000284, -9.047800747817580813, -8.000000000000007105 ) ) ;
#27010 = DIRECTION ( 'NONE',  ( 1.000000000000000000, 0.000000000000000000, 0.000000000000000000 ) ) ;
#27011 = AXIS2_PLACEMENT_3D ( 'NONE', #1826, #11230, #8907 ) ;
#27012 = ORIENTED_EDGE ( 'NONE', *, *, #19067, .F. ) ;
#27013 = CARTESIAN_POINT ( 'NONE',  ( 16.93750000000001421, 2.000000000000151879, -0.8284271247462354770 ) ) ;
#27014 = CARTESIAN_POINT ( 'NONE',  ( 0.1950273200666168272, -15.66255992321440438, -7.807776097887558997 ) ) ;
#27015 = CARTESIAN_POINT ( 'NONE',  ( -6.000000000000023093, 1.607695154586625819, -147.9033121635129930 ) ) ;
#27016 = CARTESIAN_POINT ( 'NONE',  ( 6.000000000000000888, 7.762456499804234384E-14, -117.0863248654052171 ) ) ;
#27017 = CARTESIAN_POINT ( 'NONE',  ( 6.000000000000000888, -1.859271017917181981E-14, -171.6636751345948539 ) ) ;
#27018 = CARTESIAN_POINT ( 'NONE',  ( 0.7660434483343199208, -15.49920295329753550, -8.125643190292789697 ) ) ;
#27019 = CARTESIAN_POINT ( 'NONE',  ( 116.8752832217622313, -1.849990392679579099, 0.000000000000000000 ) ) ;
#27020 = CARTESIAN_POINT ( 'NONE',  ( 5.412658773652712085, -3.125000000000086153, -64.56698729810783277 ) ) ;
#27021 = CARTESIAN_POINT ( 'NONE',  ( 7.216878364870455975, -6.409875621278545621E-14, -55.44198729810780435 ) ) ;
#27022 = CARTESIAN_POINT ( 'NONE',  ( 159.0000000000000284, -59.99999999999980105, 4.000000000000003553 ) ) ;
#27023 = DIRECTION ( 'NONE',  ( -7.147005652999508048E-36, 5.642372883946980038E-36, 1.000000000000000000 ) ) ;
#27024 = CARTESIAN_POINT ( 'NONE',  ( 147.6636751345948255, 0.000000000000000000, 5.500000000000005329 ) ) ;
#27025 = CARTESIAN_POINT ( 'NONE',  ( 0.000000000000000000, 5.999999999999977796, -127.7886751345948539 ) ) ;
#27026 = EDGE_CURVE ( 'NONE', #18475, #17985, #10888, .T. ) ;
#27027 = CARTESIAN_POINT ( 'NONE',  ( -6.350852961085760029, -1.281975124255709124E-13, -130.1250000000000284 ) ) ;
#27028 = ORIENTED_EDGE ( 'NONE', *, *, #6087, .F. ) ;
#27029 = FACE_OUTER_BOUND ( 'NONE', #9886, .T. ) ;
#27030 = CARTESIAN_POINT ( 'NONE',  ( 16.71132486540527395, 2.500000000000057732, -5.551115123125782702E-14 ) ) ;
#27031 = CARTESIAN_POINT ( 'NONE',  ( -5.999999999999962697, 3.323446944526963891E-14, -147.8363248654052313 ) ) ;
#27032 = ORIENTED_EDGE ( 'NONE', *, *, #18028, .T. ) ;
#27033 = CARTESIAN_POINT ( 'NONE',  ( 113.3747167782374987, -1.110223024625156540E-13, -1.849990392679523588 ) ) ;
#27034 =( NAMED_UNIT ( * ) PLANE_ANGLE_UNIT ( ) SI_UNIT ( $, .RADIAN. ) );
#27035 = CARTESIAN_POINT ( 'NONE',  ( 5.412658773652712085, -3.125000000000086153, -114.0669872981078186 ) ) ;
#27036 = CARTESIAN_POINT ( 'NONE',  ( 135.0000000000000284, 4.401348733996699458, -3.652467542001735179 ) ) ;
#27037 = CARTESIAN_POINT ( 'NONE',  ( -5.196152422706601826, 2.999999999999975131, -90.96132486540520290 ) ) ;
#27038 = CARTESIAN_POINT ( 'NONE',  ( 116.0624999999999005, 2.500000000000054623, 1.035533905932929599 ) ) ;
#27039 = AXIS2_PLACEMENT_3D ( 'NONE', #23959, #14607, #19073 ) ;
#27040 = CARTESIAN_POINT ( 'NONE',  ( 159.9746938747179854, -12.51900727150228931, 3.255903183154158498 ) ) ;
#27041 = CARTESIAN_POINT ( 'NONE',  ( 140.1562500000000853, -6.000000000000005329, 2.485281374238555774 ) ) ;
#27042 =( BOUNDED_CURVE ( )  B_SPLINE_CURVE ( 2, ( #1069, #3354, #12628, #10459, #19382, #19232, #17088, #26267, #5512 ),
 .UNSPECIFIED., .F., .T. ) 
 B_SPLINE_CURVE_WITH_KNOTS ( ( 3, 2, 2, 2, 3 ),
 ( 0.5624999999999991118, 0.5687499999999993117, 0.5749999999999995115, 0.5812499999999999334, 0.5875000000000001332 ),
 .UNSPECIFIED. ) 
 CURVE ( )  GEOMETRIC_REPRESENTATION_ITEM ( )  RATIONAL_B_SPLINE_CURVE ( ( 1.000000000000010880, 0.9238795325112759693, 1.000000000000000000, 0.9238795325112867385, 1.000000000000000000, 0.9238795325112867385, 1.000000000000000000, 0.9238795325112854062, 1.000000000000001332 ) ) 
 REPRESENTATION_ITEM ( '' )  );
#27043 = AXIS2_PLACEMENT_3D ( 'NONE', #7507, #16921, #28091 ) ;
#27045 = CARTESIAN_POINT ( 'NONE',  ( -5.196152422706601826, 2.999999999999975131, -81.03867513459483973 ) ) ;
#27044 = CIRCLE ( 'NONE', #10391, 0.5000000000000000000 ) ;
#27046 = EDGE_CURVE ( 'NONE', #25773, #20871, #18406, .T. ) ;
#27047 = CARTESIAN_POINT ( 'NONE',  ( -6.350852961085760029, -1.281975124255709124E-13, -47.62500000000000000 ) ) ;
#27048 = CARTESIAN_POINT ( 'NONE',  ( -3.464101615137757051, -5.999999999999979572, -62.66367513459483973 ) ) ;
#27049 = CARTESIAN_POINT ( 'NONE',  ( -5.999999999999919176, 1.607695154586804565, -61.48066243270261566 ) ) ;
#27050 = CARTESIAN_POINT ( 'NONE',  ( 7.216878364870455975, -6.409875621278545621E-14, -78.80801270189225249 ) ) ;
#27051 = CARTESIAN_POINT ( 'NONE',  ( 116.6488248654049471, 2.000000000000091926, -0.8284271247460553989 ) ) ;
#27052 = CARTESIAN_POINT ( 'NONE',  ( 149.0476497308104058, 0.000000000000000000, -5.000000000000004441 ) ) ;
#27053 = VECTOR ( 'NONE', #8687, 1000.000000000000000 ) ;
#27054 = SURFACE_SIDE_STYLE ('',( #13136 ) ) ;
#27055 = PRESENTATION_STYLE_ASSIGNMENT (( #13139 ) ) ;
#27056 = VECTOR ( 'NONE', #5572, 1000.000000000000000 ) ;
#27057 = ADVANCED_FACE ( 'NONE', ( #20243 ), #27723, .T. ) ;
#27058 = CARTESIAN_POINT ( 'NONE',  ( -4.763139720814407951, 2.749999999999946709, -131.7500000000000284 ) ) ;
#27059 = CARTESIAN_POINT ( 'NONE',  ( 105.7261751345946976, -1.999999999999881650, 0.8284271247462955401 ) ) ;
#27060 = CARTESIAN_POINT ( 'NONE',  ( 101.5358983848621932, 0.000000000000000000, 0.000000000000000000 ) ) ;
#27061 = CARTESIAN_POINT ( 'NONE',  ( -3.464101615137725076, 5.999999999999979572, -178.0863248654052313 ) ) ;
#27062 = ORIENTED_EDGE ( 'NONE', *, *, #10445, .F. ) ;
#27063 = CARTESIAN_POINT ( 'NONE',  ( -3.175426480542816066, -5.500000000000057732, -59.37500000000005684 ) ) ;
#27064 = DIRECTION ( 'NONE',  ( -1.000000000000000000, -1.665334536937736783E-16, -2.220446049250315546E-16 ) ) ;
#27065 = CARTESIAN_POINT ( 'NONE',  ( 3.175426480543072749, -5.500000000000105693, -60.62500000000000000 ) ) ;
#27066 = ORIENTED_EDGE ( 'NONE', *, *, #10130, .F. ) ;
#27067 = CARTESIAN_POINT ( 'NONE',  ( 107.8124999999997442, 1.035533905932809473, -2.499999999999784173 ) ) ;
#27068 = CARTESIAN_POINT ( 'NONE',  ( 145.5000000000000284, 6.000000000000005329, 0.000000000000000000 ) ) ;
#27069 = DIRECTION ( 'NONE',  ( 1.000000000000000000, -5.551115123125773458E-17, -1.260129944081490338E-35 ) ) ;
#27070 = CARTESIAN_POINT ( 'NONE',  ( 15.75000000000006928, 2.775557561562891351E-13, -2.000000000000057288 ) ) ;
#27071 = VECTOR ( 'NONE', #12390, 1000.000000000000114 ) ;
#27072 = CARTESIAN_POINT ( 'NONE',  ( -6.000000000000007105, -1.607695154586655129, -49.34668783648707091 ) ) ;
#27073 = ORIENTED_EDGE ( 'NONE', *, *, #1587, .T. ) ;
#27074 = CARTESIAN_POINT ( 'NONE',  ( 147.0000000000000284, 6.000000000000005329, 0.000000000000000000 ) ) ;
#27075 = CARTESIAN_POINT ( 'NONE',  ( 161.1719978263368205, -2.466862157723925364, 5.117282274813819143 ) ) ;
#27076 = VERTEX_POINT ( 'NONE', #13351 ) ;
#27077 = CARTESIAN_POINT ( 'NONE',  ( -4.763139720814407951, 2.749999999999946709, -146.7500000000000568 ) ) ;
#27078 = CARTESIAN_POINT ( 'NONE',  ( 5.412658773652712085, -3.125000000000086153, -48.06698729810781856 ) ) ;
#27079 = CARTESIAN_POINT ( 'NONE',  ( 16.75000000000015277, 1.665334536937734811E-13, -2.000000000000001776 ) ) ;
#27080 = VERTEX_POINT ( 'NONE', #11032 ) ;
#27081 = CARTESIAN_POINT ( 'NONE',  ( 3.608439182435180470, -6.249999999999997335, -145.6919872981078470 ) ) ;
#27082 = EDGE_CURVE ( 'NONE', #8702, #567, #29547, .T. ) ;
#27083 = CARTESIAN_POINT ( 'NONE',  ( -4.763139720814407951, -2.750000000000016431, -74.50000000000001421 ) ) ;
#27084 = CARTESIAN_POINT ( 'NONE',  ( 14.93750000000007461, -2.649519052838298805, -1.097466725451559322 ) ) ;
#27085 = CARTESIAN_POINT ( 'NONE',  ( 2.775557561562891351E-14, -6.250000000000061284, -95.68301270189222407 ) ) ;
#27086 = CARTESIAN_POINT ( 'NONE',  ( -2.693961096941767774, -10.67153403684355339, -19.62422301979501782 ) ) ;
#27087 = CARTESIAN_POINT ( 'NONE',  ( -9.999999999999793943, 9.000000000000007105, -4.000000000000003553 ) ) ;
#27088 = FACE_OUTER_BOUND ( 'NONE', #20120, .T. ) ;
#27089 = CARTESIAN_POINT ( 'NONE',  ( 0.000000000000000000, -5.999999999999991118, -86.53867513459483973 ) ) ;
#27090 = EDGE_CURVE ( 'NONE', #23148, #5313, #11634, .T. ) ;
#27091 = DIRECTION ( 'NONE',  ( -1.193484356672575258E-15, -0.3950055220923786026, 0.9186787455452135598 ) ) ;
#27092 = EDGE_CURVE ( 'NONE', #20296, #24857, #21126, .T. ) ;
#27093 = CARTESIAN_POINT ( 'NONE',  ( -3.175426480542816066, -5.500000000000057732, -158.3750000000000284 ) ) ;
#27094 = CARTESIAN_POINT ( 'NONE',  ( 137.0550748654052597, -5.500000000000012434, -2.278174593052012309 ) ) ;
#27095 = CARTESIAN_POINT ( 'NONE',  ( 6.350852961086080661, -9.614813431917819062E-14, -148.8750000000000284 ) ) ;
#27096 = CARTESIAN_POINT ( 'NONE',  ( -5.999999999999919176, 1.607695154586804565, -48.90331216351300725 ) ) ;
#27097 = CARTESIAN_POINT ( 'NONE',  ( -6.350852961085760029, -1.281975124255709124E-13, -89.62500000000001421 ) ) ;
#27098 = CYLINDRICAL_SURFACE ( 'NONE', #180, 15.00000000000000000 ) ;
#27099 = CARTESIAN_POINT ( 'NONE',  ( 24.45536158780166858, 1.279379774540844616, 2.256154131391882256 ) ) ;
#27100 = CARTESIAN_POINT ( 'NONE',  ( -3.175426480542816510, -5.500000000000057732, -83.37500000000004263 ) ) ;
#27101 = CIRCLE ( 'NONE', #2605, 15.00000000000000000 ) ;
#27102 = CARTESIAN_POINT ( 'NONE',  ( 5.196152422706629359, -2.999999999999988898, -120.2113248654052029 ) ) ;
#27103 = CARTESIAN_POINT ( 'NONE',  ( 0.000000000000000000, -14.14213562373095634, 8.500000000000007105 ) ) ;
#27104 = DIRECTION ( 'NONE',  ( 0.000000000000000000, 1.000000000000000000, 0.000000000000000000 ) ) ;
#27105 = DIRECTION ( 'NONE',  ( 1.000000000000000000, -5.551115123125773458E-17, -1.260129944081490338E-35 ) ) ;
#27106 = CARTESIAN_POINT ( 'NONE',  ( 0.000000000000000000, -5.999999999999991118, -165.4613248654052029 ) ) ;
#27107 = CARTESIAN_POINT ( 'NONE',  ( 120.1247167782375698, -1.849990392679523588, 0.000000000000000000 ) ) ;
#27108 = CARTESIAN_POINT ( 'NONE',  ( 3.464101615137852974, 5.999999999999884537, -174.4136751345948255 ) ) ;
#27109 = ORIENTED_EDGE ( 'NONE', *, *, #3574, .T. ) ;
#27110 = CARTESIAN_POINT ( 'NONE',  ( 9.433704689814137012, -8.984907651778784631E-16, 16.18577070100374371 ) ) ;
#27111 = CARTESIAN_POINT ( 'NONE',  ( 145.8824251345948539, 5.500000000000012434, 2.278174593052012309 ) ) ;
#27112 = CARTESIAN_POINT ( 'NONE',  ( 118.2502832217622739, 1.308140751793640533, -1.308140751793418488 ) ) ;
#27113 = ORIENTED_EDGE ( 'NONE', *, *, #424, .T. ) ;
#27114 = EDGE_CURVE ( 'NONE', #23700, #16823, #13972, .T. ) ;
#27115 = CARTESIAN_POINT ( 'NONE',  ( 6.350852961086080661, -9.614813431917819062E-14, -96.37499999999997158 ) ) ;
#27116 = CARTESIAN_POINT ( 'NONE',  ( 6.000000000000000888, 1.743066579297358182E-13, -71.16367513459481131 ) ) ;
#27117 = CARTESIAN_POINT ( 'NONE',  ( 2.775557561562891351E-14, 6.250000000000033751, -111.4330127018922099 ) ) ;
#27118 = CIRCLE ( 'NONE', #15409, 28.99999999999999645 ) ;
#27119 = ORIENTED_EDGE ( 'NONE', *, *, #21156, .F. ) ;
#27120 = DIRECTION ( 'NONE',  ( 1.000000000000000000, -5.551115123125773458E-17, -1.260129944081490338E-35 ) ) ;
#27121 = CARTESIAN_POINT ( 'NONE',  ( -5.999999999999919176, 1.607695154586804565, -62.98066243270261566 ) ) ;
#27122 = CARTESIAN_POINT ( 'NONE',  ( 5.412658773652739619, 3.124999999999988898, -51.68301270189223828 ) ) ;
#27123 = ORIENTED_EDGE ( 'NONE', *, *, #9151, .T. ) ;
#27124 = CARTESIAN_POINT ( 'NONE',  ( -4.999999999999886313, -14.50000000000001243, -7.500000000000007105 ) ) ;
#27125 = EDGE_CURVE ( 'NONE', #15294, #14644, #487, .T. ) ;
#27126 =( BOUNDED_CURVE ( )  B_SPLINE_CURVE ( 2, ( #13192, #1148, #10721, #997, #19608, #28949, #17472, #20061, #12877 ),
 .UNSPECIFIED., .F., .T. ) 
 B_SPLINE_CURVE_WITH_KNOTS ( ( 3, 2, 2, 2, 3 ),
 ( 0.8593750000000000000, 0.8671875000000000000, 0.8750000000000000000, 0.8828125000000000000, 0.8906250000000000000 ),
 .UNSPECIFIED. ) 
 CURVE ( )  GEOMETRIC_REPRESENTATION_ITEM ( )  RATIONAL_B_SPLINE_CURVE ( ( 1.000000000000000000, 0.9238795325112867385, 1.000000000000000000, 0.9238795325112867385, 1.000000000000000000, 0.9238795325112867385, 1.000000000000000000, 0.9238795325112867385, 1.000000000000000000 ) ) 
 REPRESENTATION_ITEM ( '' )  );
#27127 = CARTESIAN_POINT ( 'NONE',  ( 5.196152422706629359, -2.999999999999988898, -119.2886751345948397 ) ) ;
#27128 = AXIS2_PLACEMENT_3D ( 'NONE', #23126, #8362, #27091 ) ;
#27129 = CARTESIAN_POINT ( 'NONE',  ( 3.464101615137757051, -5.999999999999979572, -166.8363248654051745 ) ) ;
#27130 = CYLINDRICAL_SURFACE ( 'NONE', #7441, 14.99999999999998579 ) ;
#27131 = CARTESIAN_POINT ( 'NONE',  ( 4.763139720814407951, -2.749999999999988454, -173.0000000000000568 ) ) ;
#27132 = CARTESIAN_POINT ( 'NONE',  ( 116.2499999999998437, 5.551115123125782702E-14, 2.500000000000168754 ) ) ;
#27133 = CARTESIAN_POINT ( 'NONE',  ( 10.00000000000012257, -0.6095397823829284967, 2.424553825692621345 ) ) ;
#27134 = CARTESIAN_POINT ( 'NONE',  ( 3.608439182435180470, 6.249999999999982236, -159.5580127018922667 ) ) ;
#27135 = DIRECTION ( 'NONE',  ( -7.147005652999508048E-36, 5.642372883946980038E-36, 1.000000000000000000 ) ) ;
#27136 = CARTESIAN_POINT ( 'NONE',  ( 4.763139720814407951, -2.749999999999988454, -107.0000000000000426 ) ) ;
#27137 = DIRECTION ( 'NONE',  ( -0.000000000000000000, -0.000000000000000000, -1.000000000000000000 ) ) ;
#27138 = CARTESIAN_POINT ( 'NONE',  ( -4.763139720814407951, -2.750000000000016431, -104.5000000000000426 ) ) ;
#27139 =( BOUNDED_CURVE ( )  B_SPLINE_CURVE ( 2, ( #24592, #1097, #19998, #6010, #10813, #8311, #3695, #20163, #15429 ),
 .UNSPECIFIED., .F., .T. ) 
 B_SPLINE_CURVE_WITH_KNOTS ( ( 3, 2, 2, 2, 3 ),
 ( 0.8375000000000002442, 0.8437500000000004441, 0.8500000000000007550, 0.8562500000000009548, 0.8625000000000012657 ),
 .UNSPECIFIED. ) 
 CURVE ( )  GEOMETRIC_REPRESENTATION_ITEM ( )  RATIONAL_B_SPLINE_CURVE ( ( 0.9999999999999973355, 0.9238795325112894030, 1.000000000000000000, 0.9238795325112867385, 1.000000000000000000, 0.9238795325112867385, 1.000000000000000000, 0.9238795325112718615, 1.000000000000014877 ) ) 
 REPRESENTATION_ITEM ( '' )  );
#27140 = CARTESIAN_POINT ( 'NONE',  ( 11.53867513459497296, 5.551115123125782702E-14, 2.500000000000002220 ) ) ;
#27141 = CARTESIAN_POINT ( 'NONE',  ( -5.196152422706573404, -3.000000000000002665, -84.71132486540523132 ) ) ;
#27142 = ORIENTED_EDGE ( 'NONE', *, *, #3123, .F. ) ;
#27143 = CARTESIAN_POINT ( 'NONE',  ( 13.25000000000003908, -1.873492889144789952, -1.873492889145123019 ) ) ;
#27144 = DIRECTION ( 'NONE',  ( -7.147005652999508048E-36, 5.642372883946980038E-36, 1.000000000000000000 ) ) ;
#27145 = CARTESIAN_POINT ( 'NONE',  ( 109.1877832217621034, 0.7662911109079489913, -1.849990392679291551 ) ) ;
#27146 = CARTESIAN_POINT ( 'NONE',  ( 0.000000000000000000, -5.999999999999991118, -133.9613248654052313 ) ) ;
#27147 = ORIENTED_EDGE ( 'NONE', *, *, #9048, .T. ) ;
#27148 = CARTESIAN_POINT ( 'NONE',  ( -2.775557561562891351E-14, -5.500000000000115463, -158.2500000000000000 ) ) ;
#27149 = CARTESIAN_POINT ( 'NONE',  ( 5.412658773652739619, 3.124999999999988898, -80.81698729810781856 ) ) ;
#27150 = CARTESIAN_POINT ( 'NONE',  ( -1.110223024625164676E-16, 2.000000000000012879, 2.021286199229734960E-15 ) ) ;
#27151 = ORIENTED_EDGE ( 'NONE', *, *, #7338, .T. ) ;
#27152 = CARTESIAN_POINT ( 'NONE',  ( 116.1488248654049755, -1.999999999999941602, 0.8284271247463557142 ) ) ;
#27153 = ORIENTED_EDGE ( 'NONE', *, *, #6435, .F. ) ;
#27154 = EDGE_LOOP ( 'NONE', ( #16263, #21001, #27012, #24511 ) ) ;
#27155 = CARTESIAN_POINT ( 'NONE',  ( 158.2500000000000284, -6.000000000000005329, 0.000000000000000000 ) ) ;
#27156 = ADVANCED_FACE ( 'NONE', ( #11663 ), #21007, .F. ) ;
#27157 = CARTESIAN_POINT ( 'NONE',  ( -3.175426480542816510, -5.500000000000057732, -119.3750000000000284 ) ) ;
#27158 = EDGE_CURVE ( 'NONE', #27870, #29809, #25294, .T. ) ;
#27159 = CARTESIAN_POINT ( 'NONE',  ( -3.608439182435115633, 6.249999999999965361, -138.3080127018922951 ) ) ;
#27160 = CARTESIAN_POINT ( 'NONE',  ( 5.999999999999999112, 2.951592740943527306E-14, -161.1636751345949108 ) ) ;
#27161 = CARTESIAN_POINT ( 'NONE',  ( 2.775557561562891351E-14, -6.250000000000061284, -126.3169872981078043 ) ) ;
#27162 = DIRECTION ( 'NONE',  ( 1.665334536937739001E-16, -1.000000000000000000, -8.881784197001260212E-16 ) ) ;
#27163 = CARTESIAN_POINT ( 'NONE',  ( 0.000000000000000000, 5.499999999999991118, -174.0000000000000568 ) ) ;
#27164 = CARTESIAN_POINT ( 'NONE',  ( 159.7627798038683693, -11.43531980891128796, 3.685954457582622190 ) ) ;
#27165 = VERTEX_POINT ( 'NONE', #28107 ) ;
#27166 = CARTESIAN_POINT ( 'NONE',  ( 12.18750000000008349, 0.8284271247463557142, 1.999999999999851674 ) ) ;
#27167 = DIRECTION ( 'NONE',  ( 5.551115123125785167E-17, -1.000000000000000000, -8.881784197001256268E-16 ) ) ;
#27168 = CARTESIAN_POINT ( 'NONE',  ( -5.999999999999963585, -1.487416814333745711E-14, -117.8363248654052313 ) ) ;
#27169 = CARTESIAN_POINT ( 'NONE',  ( -5.999999999999963585, -1.487416814333745711E-14, -55.41367513459483973 ) ) ;
#27170 = DIRECTION ( 'NONE',  ( 0.000000000000000000, 0.000000000000000000, 1.000000000000000000 ) ) ;
#27171 = CARTESIAN_POINT ( 'NONE',  ( 111.6877832217621176, -0.7662911109077388261, 1.849990392679652151 ) ) ;
#27172 = CARTESIAN_POINT ( 'NONE',  ( -5.412658773652684552, -3.125000000000099920, -68.06698729810783277 ) ) ;
#27173 = CARTESIAN_POINT ( 'NONE',  ( 5.412658773652712085, -3.125000000000086153, -52.56698729810782567 ) ) ;
#27174 = LINE ( 'NONE', #6145, #19004 ) ;
#27175 = DIRECTION ( 'NONE',  ( -0.000000000000000000, -0.000000000000000000, 1.000000000000000000 ) ) ;
#27176 = CARTESIAN_POINT ( 'NONE',  ( 119.9999999999998295, 1.988103546243131570, -1.253414257844930102 ) ) ;
#27177 = CARTESIAN_POINT ( 'NONE',  ( 3.464101615137852974, 5.999999999999884537, -74.83632486540521711 ) ) ;
#27178 = AXIS2_PLACEMENT_3D ( 'NONE', #14793, #19402, #12059 ) ;
#27179 = CARTESIAN_POINT ( 'NONE',  ( -2.775557561562891351E-14, -5.500000000000115463, -132.7500000000000284 ) ) ;
#27180 = CARTESIAN_POINT ( 'NONE',  ( 3.464101615137852974, 5.999999999999884537, -50.83632486540523132 ) ) ;
#27181 = VERTEX_POINT ( 'NONE', #11892 ) ;
#27182 = CARTESIAN_POINT ( 'NONE',  ( 5.999999999999999112, 2.951592740943527306E-14, -158.1636751345948539 ) ) ;
#27183 = CARTESIAN_POINT ( 'NONE',  ( -3.464101615137725076, 5.999999999999979572, -119.5863248654052313 ) ) ;
#27184 = DIRECTION ( 'NONE',  ( -1.000000000000000000, -1.665334536937731113E-16, 1.526556658859586792E-16 ) ) ;
#27185 = CARTESIAN_POINT ( 'NONE',  ( 137.3586002691896226, 2.071067811865468400, 4.999999999999989342 ) ) ;
#27186 = ORIENTED_EDGE ( 'NONE', *, *, #28246, .T. ) ;
#27187 = CARTESIAN_POINT ( 'NONE',  ( 114.3122167782374419, -0.7662911109077388261, -1.849990392679231599 ) ) ;
#27188 = FACE_OUTER_BOUND ( 'NONE', #25069, .T. ) ;
#27189 = CARTESIAN_POINT ( 'NONE',  ( 15.21132486540524553, -2.499999999999780176, -1.110223024625156540E-13 ) ) ;
#27190 = CARTESIAN_POINT ( 'NONE',  ( -7.216878364870328078, 0.000000000000000000, -117.6919872981078470 ) ) ;
#27191 = CARTESIAN_POINT ( 'NONE',  ( -3.464101615137757051, -5.999999999999979572, -173.6636751345947687 ) ) ;
#27192 = CARTESIAN_POINT ( 'NONE',  ( 114.9999999999999716, 2.500000000000002220, 0.000000000000000000 ) ) ;
#27193 = ORIENTED_EDGE ( 'NONE', *, *, #1936, .F. ) ;
#27194 = LINE ( 'NONE', #8940, #266 ) ;
#27195 = CARTESIAN_POINT ( 'NONE',  ( 142.9687500000000000, -2.485281374238585972, 6.000000000000005329 ) ) ;
#27196 = CIRCLE ( 'NONE', #14096, 4.000000000000003553 ) ;
#27197 = ADVANCED_FACE ( 'NONE', ( #9702 ), #7386, .F. ) ;
#27198 = CARTESIAN_POINT ( 'NONE',  ( -4.763139720814407951, -2.750000000000016431, -53.49999999999999289 ) ) ;
#27199 = CARTESIAN_POINT ( 'NONE',  ( 159.4761751345948255, 3.889087296526011706, 3.889087296526011706 ) ) ;
#27200 = CARTESIAN_POINT ( 'NONE',  ( 5.196152422706629359, 3.000000000000002665, -120.5386751345948255 ) ) ;
#27201 = CARTESIAN_POINT ( 'NONE',  ( 6.000000000000000888, -1.859271017917181981E-14, -79.58632486540520290 ) ) ;
#27202 = CARTESIAN_POINT ( 'NONE',  ( 3.608439182435180470, -6.249999999999997335, -77.55801270189225249 ) ) ;
#27203 = DIRECTION ( 'NONE',  ( -1.000000000000000000, -0.000000000000000000, -0.000000000000000000 ) ) ;
#27204 = CARTESIAN_POINT ( 'NONE',  ( 147.7351497308104342, 3.535533905932725318, -3.535533905932725318 ) ) ;
#27205 = DIRECTION ( 'NONE',  ( 1.000000000000000000, -5.551115123125773458E-17, -1.260129944081490338E-35 ) ) ;
#27206 =( NAMED_UNIT ( * ) PLANE_ANGLE_UNIT ( ) SI_UNIT ( $, .RADIAN. ) );
#27207 = CIRCLE ( 'NONE', #24786, 1.000000000000000888 ) ;
#27208 = DIRECTION ( 'NONE',  ( -8.326672684688675286E-17, -2.081668171172168821E-17, 1.000000000000000000 ) ) ;
#27209 = DIRECTION ( 'NONE',  ( 1.000000000000000000, -5.551115123125773458E-17, -1.260129944081490338E-35 ) ) ;
#27210 = CARTESIAN_POINT ( 'NONE',  ( 135.0085428039600970, -7.340339031313663831, 8.407416807790594859 ) ) ;
#27211 = CARTESIAN_POINT ( 'NONE',  ( -6.350852961085760029, -1.281975124255709124E-13, -134.6250000000000284 ) ) ;
#27212 = DIRECTION ( 'NONE',  ( -7.147005652999508048E-36, 5.642372883946980038E-36, 1.000000000000000000 ) ) ;
#27213 = VERTEX_POINT ( 'NONE', #2619 ) ;
#27214 = CARTESIAN_POINT ( 'NONE',  ( 0.000000000000000000, 5.499999999999991118, -63.00000000000000000 ) ) ;
#27215 = DIRECTION ( 'NONE',  ( 1.000000000000000000, -5.551115123125773458E-17, -1.260129944081490338E-35 ) ) ;
#27216 = SURFACE_SIDE_STYLE ('',( #17899 ) ) ;
#27217 = ORIENTED_EDGE ( 'NONE', *, *, #25761, .T. ) ;
#27218 = CARTESIAN_POINT ( 'NONE',  ( 107.6249999999998721, -1.767766952966376426, -1.767766952966320915 ) ) ;
#27219 = CARTESIAN_POINT ( 'NONE',  ( 143.3437500000000853, -6.000000000000005329, -2.485281374238556218 ) ) ;
#27220 = DIRECTION ( 'NONE',  ( 1.000000000000000000, -5.551115123125773458E-17, -1.260129944081490338E-35 ) ) ;
#27221 = EDGE_CURVE ( 'NONE', #25740, #1154, #3060, .T. ) ;
#27222 = DIRECTION ( 'NONE',  ( -7.147005652999508048E-36, 5.642372883946980038E-36, 1.000000000000000000 ) ) ;
#27223 =( BOUNDED_CURVE ( )  B_SPLINE_CURVE ( 2, ( #11529, #27291, #1969, #25143, #15843, #6408, #23185, #20719, #24993 ),
 .UNSPECIFIED., .F., .T. ) 
 B_SPLINE_CURVE_WITH_KNOTS ( ( 3, 2, 2, 2, 3 ),
 ( 0.6176470588235294379, 0.6250000000000000000, 0.6323529411764705621, 0.6397058823529411242, 0.6470588235294117974 ),
 .UNSPECIFIED. ) 
 CURVE ( )  GEOMETRIC_REPRESENTATION_ITEM ( )  RATIONAL_B_SPLINE_CURVE ( ( 1.000000000000000000, 0.9238795325112867385, 1.000000000000000000, 0.9238795325112867385, 1.000000000000000000, 0.9238795325112867385, 1.000000000000000000, 0.9238795325112867385, 1.000000000000000000 ) ) 
 REPRESENTATION_ITEM ( '' )  );
#27224 = ORIENTED_EDGE ( 'NONE', *, *, #29154, .T. ) ;
#27225 = CARTESIAN_POINT ( 'NONE',  ( 135.9375000000000568, -4.242640687119298093, -4.242640687119298093 ) ) ;
#27226 = CARTESIAN_POINT ( 'NONE',  ( 161.4122677408628874, -5.290788382733226491, -2.657712799832109063 ) ) ;
#27227 = ORIENTED_EDGE ( 'NONE', *, *, #6164, .F. ) ;
#27228 = VECTOR ( 'NONE', #6650, 1000.000000000000000 ) ;
#27229 = CARTESIAN_POINT ( 'NONE',  ( -4.763139720814407951, 2.749999999999946709, -142.2500000000000000 ) ) ;
#27230 = EDGE_CURVE ( 'NONE', #13661, #29800, #5697, .T. ) ;
#27231 = CARTESIAN_POINT ( 'NONE',  ( 17.62500000000008527, -1.414213562372923505, -1.414213562373145550 ) ) ;
#27232 = ORIENTED_EDGE ( 'NONE', *, *, #27812, .F. ) ;
#27233 = CARTESIAN_POINT ( 'NONE',  ( -3.175426480542816510, -5.500000000000057732, -72.87500000000000000 ) ) ;
#27234 = CARTESIAN_POINT ( 'NONE',  ( 15.06250000000004441, -1.097466725451439196, -2.649519052838419153 ) ) ;
#27235 = CARTESIAN_POINT ( 'NONE',  ( -3.608439182435052128, -6.250000000000110134, -95.80801270189220986 ) ) ;
#27236 = AXIS2_PLACEMENT_3D ( 'NONE', #23167, #2111, #11515 ) ;
#27237 = CARTESIAN_POINT ( 'NONE',  ( -10.00000000000000178, 9.000000000000007105, -4.000000000000003553 ) ) ;
#27238 = DIRECTION ( 'NONE',  ( 0.000000000000000000, 0.000000000000000000, 1.000000000000000000 ) ) ;
#27239 = CARTESIAN_POINT ( 'NONE',  ( 148.0238248654052313, 3.889087296526011706, -3.889087296526011706 ) ) ;
#27240 = CARTESIAN_POINT ( 'NONE',  ( 5.196152422706629359, -2.999999999999988898, -86.28867513459481131 ) ) ;
#27241 = DIRECTION ( 'NONE',  ( 1.000000000000000000, 0.000000000000000000, 0.000000000000000000 ) ) ;
#27242 = CARTESIAN_POINT ( 'NONE',  ( -3.175426480542816066, -5.500000000000057732, -156.8750000000000284 ) ) ;
#27243 = CARTESIAN_POINT ( 'NONE',  ( -5.999999999999963585, -1.487416814333745711E-14, -117.8363248654052313 ) ) ;
#27244 = CARTESIAN_POINT ( 'NONE',  ( 156.5550748654052029, -5.500000000000012434, -2.278174593052012309 ) ) ;
#27245 = AXIS2_PLACEMENT_3D ( 'NONE', #7653, #14604, #16915 ) ;
#27246 = CARTESIAN_POINT ( 'NONE',  ( 0.000000000000000000, 5.499999999999991118, -85.50000000000001421 ) ) ;
#27247 = DIRECTION ( 'NONE',  ( -7.147005652999508048E-36, 5.642372883946980038E-36, 1.000000000000000000 ) ) ;
#27248 = CARTESIAN_POINT ( 'NONE',  ( -3.175426480542816510, -5.500000000000057732, -72.87500000000000000 ) ) ;
#27249 = CARTESIAN_POINT ( 'NONE',  ( 152.4523502691896510, 0.000000000000000000, 5.000000000000004441 ) ) ;
#27250 = CARTESIAN_POINT ( 'NONE',  ( 161.3393457717174044, -4.235451996440949607, -4.042466237327082546 ) ) ;
#27251 = DIRECTION ( 'NONE',  ( 0.000000000000000000, 1.000000000000000000, -0.000000000000000000 ) ) ;
#27252 = EDGE_CURVE ( 'NONE', #27478, #20611, #23534, .T. ) ;
#27253 = CARTESIAN_POINT ( 'NONE',  ( 6.000000000000000888, 5.577813053751546416E-15, -165.0863248654052029 ) ) ;
#27254 = CARTESIAN_POINT ( 'NONE',  ( 116.0000000000000142, 6.735557395310442023E-16, 5.500000000000000000 ) ) ;
#27255 = FACE_OUTER_BOUND ( 'NONE', #14216, .T. ) ;
#27256 = ORIENTED_EDGE ( 'NONE', *, *, #3456, .T. ) ;
#27257 = CARTESIAN_POINT ( 'NONE',  ( 157.3125000000000284, 4.242640687119298093, -4.242640687119298093 ) ) ;
#27258 = CARTESIAN_POINT ( 'NONE',  ( -3.464101615137757051, -5.999999999999979572, -172.1636751345947687 ) ) ;
#27259 = CARTESIAN_POINT ( 'NONE',  ( 116.5002832217622171, 1.308140751793696044, 1.308140751793640533 ) ) ;
#27260 = AXIS2_PLACEMENT_3D ( 'NONE', #8564, #12759, #3481 ) ;
#27261 = CARTESIAN_POINT ( 'NONE',  ( -5.630955349224697315, 2.071796769723730058, -179.9999999999999432 ) ) ;
#27262 = ADVANCED_FACE ( 'NONE', ( #19375 ), #28699, .F. ) ;
#27263 = ORIENTED_EDGE ( 'NONE', *, *, #5413, .F. ) ;
#27264 = CARTESIAN_POINT ( 'NONE',  ( 4.763139720814407951, 2.750000000000002665, -99.25000000000000000 ) ) ;
#27265 = CARTESIAN_POINT ( 'NONE',  ( -6.000000000000007105, -1.607695154586655129, -89.84668783648706381 ) ) ;
#27266 = CARTESIAN_POINT ( 'NONE',  ( -3.608439182435115633, 6.249999999999965361, -115.8080127018922383 ) ) ;
#27267 = ORIENTED_EDGE ( 'NONE', *, *, #1648, .T. ) ;
#27268 = DIRECTION ( 'NONE',  ( 0.000000000000000000, 0.000000000000000000, -1.000000000000000000 ) ) ;
#27269 = AXIS2_PLACEMENT_3D ( 'NONE', #27962, #25519, #16358 ) ;
#27270 = CARTESIAN_POINT ( 'NONE',  ( -5.999999999999963585, 1.780251999655701777E-13, -51.83632486540522422 ) ) ;
#27271 = CARTESIAN_POINT ( 'NONE',  ( 5.412658773652739619, 3.124999999999988898, -48.68301270189223828 ) ) ;
#27272 = EDGE_LOOP ( 'NONE', ( #29845, #7076, #259, #11986 ) ) ;
#27273 = SHAPE_REPRESENTATION_RELATIONSHIP ( 'NONE' , 'NONE' ,  #15661, #13685 ) ;
#27274 = CARTESIAN_POINT ( 'NONE',  ( -5.196152422706601826, 2.999999999999975131, -135.9613248654052313 ) ) ;
#27275 = CARTESIAN_POINT ( 'NONE',  ( 3.175426480543072749, 5.499999999999865885, -160.6250000000000284 ) ) ;
#27276 = MECHANICAL_DESIGN_GEOMETRIC_PRESENTATION_REPRESENTATION (  '', ( #27787 ), #28745 ) ;
#27277 = CARTESIAN_POINT ( 'NONE',  ( 118.0624999999998010, 2.500000000000055067, 1.035533905932929599 ) ) ;
#27278 = CARTESIAN_POINT ( 'NONE',  ( 160.0000000000000284, -12.64911064067353408, -3.000000000000002665 ) ) ;
#27279 = CARTESIAN_POINT ( 'NONE',  ( 4.763139720814407951, -2.749999999999988454, -109.9999999999999858 ) ) ;
#27280 = CARTESIAN_POINT ( 'NONE',  ( 13.10117513459486993, 1.035533905932869425, -2.499999999999904521 ) ) ;
#27281 = CARTESIAN_POINT ( 'NONE',  ( -3.175426480542816510, -5.500000000000057732, -104.3750000000000142 ) ) ;
#27282 = CARTESIAN_POINT ( 'NONE',  ( 5.999999999999999112, 2.951592740943527306E-14, -152.1636751345948255 ) ) ;
#27283 =( NAMED_UNIT ( * ) PLANE_ANGLE_UNIT ( ) SI_UNIT ( $, .RADIAN. ) );
#27284 = CARTESIAN_POINT ( 'NONE',  ( 3.464101615137852974, 5.999999999999884537, -145.3363248654052029 ) ) ;
#27285 = ORIENTED_EDGE ( 'NONE', *, *, #16540, .F. ) ;
#27286 = CARTESIAN_POINT ( 'NONE',  ( 15.68750000000006217, 2.649519052838358757, 1.097466725451379244 ) ) ;
#27287 = CARTESIAN_POINT ( 'NONE',  ( 116.5624999999998863, -2.499999999999844569, -1.035533905932629173 ) ) ;
#27288 = ADVANCED_FACE ( 'NONE', ( #16645 ), #18786, .F. ) ;
#27289 = CARTESIAN_POINT ( 'NONE',  ( 111.3752832217622739, 1.849990392679468076, 0.000000000000000000 ) ) ;
#27290 = CARTESIAN_POINT ( 'NONE',  ( 23.60117513459490013, -1.035533905932568999, 2.499999999999844569 ) ) ;
#27291 = CARTESIAN_POINT ( 'NONE',  ( 110.1488248654049897, -2.000000000000001776, 0.8284271247464157772 ) ) ;
#27292 = VECTOR ( 'NONE', #18787, 1000.000000000000000 ) ;
#27293 = CARTESIAN_POINT ( 'NONE',  ( 5.412658773652712085, -3.125000000000086153, -88.56698729810786119 ) ) ;
#27294 = CARTESIAN_POINT ( 'NONE',  ( 0.000000000000000000, -5.999999999999991118, -103.0386751345948539 ) ) ;
#27295 = ORIENTED_EDGE ( 'NONE', *, *, #9505, .F. ) ;
#27296 = CONICAL_SURFACE ( 'NONE', #14132, 2.499999999999999112, 0.7853981633974522758 ) ;
#27297 = ADVANCED_FACE ( 'NONE', ( #1365 ), #21630, .T. ) ;
#27298 = CARTESIAN_POINT ( 'NONE',  ( 6.000000000000000888, 1.743066579297358182E-13, -75.08632486540521711 ) ) ;
#27299 = EDGE_CURVE ( 'NONE', #14042, #22235, #14319, .T. ) ;
#27300 = CARTESIAN_POINT ( 'NONE',  ( -3.175426480542816510, -5.500000000000057732, -150.8750000000000000 ) ) ;
#27301 = VERTEX_POINT ( 'NONE', #26558 ) ;
#27302 = VERTEX_POINT ( 'NONE', #6133 ) ;
#27303 = CARTESIAN_POINT ( 'NONE',  ( 153.7500000000000284, -6.000000000000005329, 0.000000000000000000 ) ) ;
#27304 = CARTESIAN_POINT ( 'NONE',  ( 4.763139720814407951, 2.750000000000002665, -121.7500000000000284 ) ) ;
#27305 =( BOUNDED_CURVE ( )  B_SPLINE_CURVE ( 2, ( #26188, #7315, #12263, #14558, #16722, #21604, #14422, #9929, #23758 ),
 .UNSPECIFIED., .F., .F. ) 
 B_SPLINE_CURVE_WITH_KNOTS ( ( 3, 2, 2, 2, 3 ),
 ( 0.9083333333333333259, 0.9092592592592592116, 0.9111111111111110938, 0.9129629629629629761, 0.9138888888888888618 ),
 .UNSPECIFIED. ) 
 CURVE ( )  GEOMETRIC_REPRESENTATION_ITEM ( )  RATIONAL_B_SPLINE_CURVE ( ( 0.9330127018922194093, 0.9330127018922194093, 1.000000000000000000, 0.8660254037844388186, 1.000000000000000000, 0.8660254037844388186, 1.000000000000000000, 0.9330127018922234061, 0.9330127018922194093 ) ) 
 REPRESENTATION_ITEM ( '' )  );
#27306 = CARTESIAN_POINT ( 'NONE',  ( -7.216878364870328078, 0.000000000000000000, -141.0580127018922099 ) ) ;
#27307 = VERTEX_POINT ( 'NONE', #17531 ) ;
#27308 = CARTESIAN_POINT ( 'NONE',  ( 0.000000000000000000, 5.999999999999977796, -57.28867513459484684 ) ) ;
#27309 = CARTESIAN_POINT ( 'NONE',  ( -3.608439182435115633, 6.249999999999965361, -122.4419872981077901 ) ) ;
#27310 = CARTESIAN_POINT ( 'NONE',  ( 2.775557561562891351E-14, 6.250000000000033751, -175.0669872981078186 ) ) ;
#27311 = VECTOR ( 'NONE', #20370, 1000.000000000000000 ) ;
#27312 = CARTESIAN_POINT ( 'NONE',  ( -3.175426480542816510, -5.500000000000057732, -173.3750000000000284 ) ) ;
#27313 = CARTESIAN_POINT ( 'NONE',  ( 159.2646601775326474, -12.02761966486299627, 3.966636896921674982 ) ) ;
#27314 = APPLICATION_CONTEXT ( 'automotive_design' ) ;
#27315 = ORIENTED_EDGE ( 'NONE', *, *, #3715, .F. ) ;
#27316 = CARTESIAN_POINT ( 'NONE',  ( 12.68750000000013500, -0.8284271247459952248, -1.999999999999911626 ) ) ;
#27317 = DIRECTION ( 'NONE',  ( -1.000000000000000000, -1.665334536937736783E-16, -2.220446049250315546E-16 ) ) ;
#27318 =( BOUNDED_CURVE ( )  B_SPLINE_CURVE ( 2, ( #6996, #25417, #2250, #30036, #20526, #4684, #18398, #30192, #9156 ),
 .UNSPECIFIED., .F., .T. ) 
 B_SPLINE_CURVE_WITH_KNOTS ( ( 3, 2, 2, 2, 3 ),
 ( 0.7968750000000000000, 0.8046875000000000000, 0.8125000000000000000, 0.8203125000000000000, 0.8281250000000000000 ),
 .UNSPECIFIED. ) 
 CURVE ( )  GEOMETRIC_REPRESENTATION_ITEM ( )  RATIONAL_B_SPLINE_CURVE ( ( 1.000000000000000000, 0.9238795325112867385, 1.000000000000000000, 0.9238795325112867385, 1.000000000000000000, 0.9238795325112867385, 1.000000000000000000, 0.9238795325112867385, 1.000000000000000000 ) ) 
 REPRESENTATION_ITEM ( '' )  );
#27319 = CARTESIAN_POINT ( 'NONE',  ( -5.999999999999919176, 1.607695154586804565, -89.98066243270262987 ) ) ;
#27320 = AXIS2_PLACEMENT_3D ( 'NONE', #19304, #28492, #5137 ) ;
#27321 = CARTESIAN_POINT ( 'NONE',  ( 140.2425748654052029, -2.278174593052322283, -5.499999999999701572 ) ) ;
#27322 = DIRECTION ( 'NONE',  ( 1.000000000000000000, -3.469446951953694061E-16, 0.000000000000000000 ) ) ;
#27323 = CARTESIAN_POINT ( 'NONE',  ( 111.2502832217621886, 1.308140751793696044, -1.308140751793640533 ) ) ;
#27324 = CARTESIAN_POINT ( 'NONE',  ( 2.775557561562891351E-14, -6.250000000000061284, -70.81698729810781856 ) ) ;
#27325 = CARTESIAN_POINT ( 'NONE',  ( 2.775557561562891351E-14, 6.250000000000033751, -55.06698729810782567 ) ) ;
#27326 = CARTESIAN_POINT ( 'NONE',  ( 104.9999999999999432, -1.999999999999998668, -7.622424050173526697E-16 ) ) ;
#27327 = CARTESIAN_POINT ( 'NONE',  ( 6.350852961086080661, -9.614813431917819062E-14, -52.87500000000002132 ) ) ;
#27328 = DIRECTION ( 'NONE',  ( 0.000000000000000000, 1.000000000000000000, -0.000000000000000000 ) ) ;
#27329 = CARTESIAN_POINT ( 'NONE',  ( 6.000000000000000888, 7.762456499804234384E-14, -123.0863248654052313 ) ) ;
#27330 = CARTESIAN_POINT ( 'NONE',  ( -3.175426480542816510, -5.500000000000057732, -132.8750000000000284 ) ) ;
#27331 = DIRECTION ( 'NONE',  ( -1.000000000000000000, -1.665334536937731113E-16, 1.526556658859586792E-16 ) ) ;
#27332 = ORIENTED_EDGE ( 'NONE', *, *, #8544, .F. ) ;
#27333 = CARTESIAN_POINT ( 'NONE',  ( -5.196152422706601826, 2.999999999999975131, -157.5386751345948539 ) ) ;
#27334 = EDGE_CURVE ( 'NONE', #1801, #25259, #28435, .T. ) ;
#27335 = DIRECTION ( 'NONE',  ( -1.000000000000000000, -1.665334536937736783E-16, -2.220446049250315546E-16 ) ) ;
#27336 = ADVANCED_FACE ( 'NONE', ( #15064 ), #27007, .T. ) ;
#27337 = CARTESIAN_POINT ( 'NONE',  ( 138.2961002691896795, 2.071067811865468400, -4.999999999999989342 ) ) ;
#27338 = ORIENTED_EDGE ( 'NONE', *, *, #25573, .F. ) ;
#27339 = CARTESIAN_POINT ( 'NONE',  ( 114.1872167782375413, -1.849990392679411677, -0.7662911109076485650 ) ) ;
#27340 = LINE ( 'NONE', #25036, #15987 ) ;
#27341 = CARTESIAN_POINT ( 'NONE',  ( 6.000000000000001776, 5.345404176511898156E-15, -178.5863248654052313 ) ) ;
#27342 = CARTESIAN_POINT ( 'NONE',  ( 3.608439182435180470, 6.249999999999982236, -118.1919872981078328 ) ) ;
#27343 = CARTESIAN_POINT ( 'NONE',  ( -5.999999999999964473, 9.063946212346262433E-15, -173.9136751345948255 ) ) ;
#27344 = ADVANCED_FACE ( 'NONE', ( #26845 ), #6292, .T. ) ;
#27345 = CARTESIAN_POINT ( 'NONE',  ( 110.6488248654049755, 2.000000000000001776, -0.8284271247459350507 ) ) ;
#27346 = ORIENTED_EDGE ( 'NONE', *, *, #19615, .T. ) ;
#27347 = CARTESIAN_POINT ( 'NONE',  ( 160.0000000000000284, -12.64911064067353408, 3.000000000000002665 ) ) ;
#27348 = CARTESIAN_POINT ( 'NONE',  ( 139.5937500000000284, 6.000000000000005329, 2.485281374238585972 ) ) ;
#27349 = AXIS2_PLACEMENT_3D ( 'NONE', #28594, #9591, #26008 ) ;
#27350 = ORIENTED_EDGE ( 'NONE', *, *, #13203, .F. ) ;
#27351 = CARTESIAN_POINT ( 'NONE',  ( 3.175426480543072749, -5.500000000000105693, -48.62500000000000711 ) ) ;
#27352 = CARTESIAN_POINT ( 'NONE',  ( 24.25000000000018829, 1.110223024625156540E-13, 2.000000000000001776 ) ) ;
#27353 = CARTESIAN_POINT ( 'NONE',  ( -5.196152422706601826, 2.999999999999975131, -61.53867513459482552 ) ) ;
#27354 = CARTESIAN_POINT ( 'NONE',  ( -7.216878364870328078, 0.000000000000000000, -67.55801270189226670 ) ) ;
#27355 = CARTESIAN_POINT ( 'NONE',  ( -9.999999999999765521, -89.00000000000001421, -3.000000000000002665 ) ) ;
#27356 = CARTESIAN_POINT ( 'NONE',  ( 151.8601497308104058, -3.535533905932725318, -3.535533905932725318 ) ) ;
#27357 = CARTESIAN_POINT ( 'NONE',  ( -5.196152422706601826, 2.999999999999975131, -177.0386751345948255 ) ) ;
#27358 = CARTESIAN_POINT ( 'NONE',  ( 6.000000000000052403, -1.607695154586662678, -66.73066243270258724 ) ) ;
#27359 = CARTESIAN_POINT ( 'NONE',  ( 3.175426480543072749, 5.499999999999865885, -133.6250000000000284 ) ) ;
#27360 = CARTESIAN_POINT ( 'NONE',  ( 3.608439182435180470, 6.249999999999982236, -147.5580127018922667 ) ) ;
#27361 = DIRECTION ( 'NONE',  ( -7.147005652999508048E-36, 5.642372883946980038E-36, 1.000000000000000000 ) ) ;
#27362 = ORIENTED_EDGE ( 'NONE', *, *, #25536, .F. ) ;
#27363 = EDGE_CURVE ( 'NONE', #29584, #4494, #13812, .T. ) ;
#27364 = CARTESIAN_POINT ( 'NONE',  ( 4.763139720814407951, 2.750000000000002665, -66.25000000000002842 ) ) ;
#27365 = CYLINDRICAL_SURFACE ( 'NONE', #22752, 2.000000000000012879 ) ;
#27366 = DIRECTION ( 'NONE',  ( -7.147005652999508048E-36, 5.642372883946980038E-36, 1.000000000000000000 ) ) ;
#27367 = EDGE_CURVE ( 'NONE', #15456, #3196, #15266, .T. ) ;
#27368 = CARTESIAN_POINT ( 'NONE',  ( 0.000000000000000000, -5.999999999999991118, -163.0386751345947971 ) ) ;
#27369 = ORIENTED_EDGE ( 'NONE', *, *, #27367, .T. ) ;
#27370 = CARTESIAN_POINT ( 'NONE',  ( 110.4374999999997442, -2.500000000000024425, 1.035533905932809473 ) ) ;
#27371 = CARTESIAN_POINT ( 'NONE',  ( 144.6562500000000284, -6.000000000000005329, 2.485281374238556218 ) ) ;
#27372 = CARTESIAN_POINT ( 'NONE',  ( 0.000000000000000000, 0.000000000000000000, 0.000000000000000000 ) ) ;
#27373 = DIRECTION ( 'NONE',  ( -0.9230769230769184652, 0.000000000000000000, 0.3846153846153959610 ) ) ;
#27374 = VERTEX_POINT ( 'NONE', #10965 ) ;
#27375 = CARTESIAN_POINT ( 'NONE',  ( 140.0625000000000284, -4.242640687119298093, 4.242640687119298093 ) ) ;
#27376 = CARTESIAN_POINT ( 'NONE',  ( 21.66367513459499605, -1.767766952966265404, 1.767766952966376426 ) ) ;
#27377 = VERTEX_POINT ( 'NONE', #6927 ) ;
#27378 = CARTESIAN_POINT ( 'NONE',  ( -2.775557561562891351E-14, -5.500000000000115463, -146.2500000000000000 ) ) ;
#27379 = B_SPLINE_CURVE_WITH_KNOTS ( 'NONE', 3,
 ( #22664, #11155, #27541, #18225 ),
 .UNSPECIFIED., .F., .F.,
 ( 4, 4 ),
 ( 0.000000000000000000, 0.0004167600821326112193 ),
 .UNSPECIFIED. ) ;
#27380 = CARTESIAN_POINT ( 'NONE',  ( 12.31250000000005151, -0.8284271247461753029, 2.000000000000091926 ) ) ;
#27381 = ORIENTED_EDGE ( 'NONE', *, *, #9843, .T. ) ;
#27382 = CARTESIAN_POINT ( 'NONE',  ( -3.175426480542816510, 5.499999999999865885, -70.37500000000004263 ) ) ;
#27383 = CARTESIAN_POINT ( 'NONE',  ( 10.00000000000015099, 1.428799426191789346, -1.736548481638942487 ) ) ;
#27384 = ORIENTED_EDGE ( 'NONE', *, *, #14089, .T. ) ;
#27385 = LINE ( 'NONE', #15468, #17737 ) ;
#27386 = FACE_OUTER_BOUND ( 'NONE', #15607, .T. ) ;
#27387 = FACE_OUTER_BOUND ( 'NONE', #22906, .T. ) ;
#27388 = CARTESIAN_POINT ( 'NONE',  ( 135.2584316331435446, -8.263189528310192600, -8.258603766105704125 ) ) ;
#27389 = CARTESIAN_POINT ( 'NONE',  ( 0.000000000000000000, 5.499999999999991118, -156.0000000000000284 ) ) ;
#27390 = FACE_OUTER_BOUND ( 'NONE', #4140, .T. ) ;
#27391 = CARTESIAN_POINT ( 'NONE',  ( 0.000000000000000000, 5.999999999999977796, -49.21132486540524553 ) ) ;
#27392 = CARTESIAN_POINT ( 'NONE',  ( 3.175426480543072749, 5.499999999999865885, -87.12500000000000000 ) ) ;
#27393 = CARTESIAN_POINT ( 'NONE',  ( -4.999999999999879208, -14.50000000000001243, -7.500000000000007105 ) ) ;
#27394 = CARTESIAN_POINT ( 'NONE',  ( -4.763139720814407951, 2.749999999999946709, -70.25000000000002842 ) ) ;
#27395 =( BOUNDED_CURVE ( )  B_SPLINE_CURVE ( 2, ( #2462, #28391, #19904, #8376, #11018, #24810, #29574, #8530, #12875 ),
 .UNSPECIFIED., .F., .T. ) 
 B_SPLINE_CURVE_WITH_KNOTS ( ( 3, 2, 2, 2, 3 ),
 ( 0.09038686088851133338, 0.09374999999999979183, 0.09999999999999939493, 0.1062499999999989980, 0.1124999999999987121 ),
 .UNSPECIFIED. ) 
 CURVE ( )  GEOMETRIC_REPRESENTATION_ITEM ( )  RATIONAL_B_SPLINE_CURVE ( ( 0.9621607869126793666, 0.9590394045766249542, 1.000000000000000000, 0.9238795325112867385, 1.000000000000000000, 0.9238795325112867385, 1.000000000000000000, 0.9238795325113029477, 0.9999999999999837907 ) ) 
 REPRESENTATION_ITEM ( '' )  );
#27396 = EDGE_CURVE ( 'NONE', #28026, #9311, #20619, .T. ) ;
#27397 = CARTESIAN_POINT ( 'NONE',  ( -3.464101615137757051, -5.999999999999979572, -120.5863248654052313 ) ) ;
#27398 = CARTESIAN_POINT ( 'NONE',  ( 149.2648502691896510, 3.535533905932725318, 3.535533905932752852 ) ) ;
#27399 = CARTESIAN_POINT ( 'NONE',  ( 3.464101615137852974, 5.999999999999884537, -106.3363248654052313 ) ) ;
#27400 = CARTESIAN_POINT ( 'NONE',  ( -3.464101615137757051, -5.999999999999979572, -175.1636751345947403 ) ) ;
#27401 = CARTESIAN_POINT ( 'NONE',  ( 114.2113248654050750, -1.999999999999890754, 0.000000000000000000 ) ) ;
#27402 = CARTESIAN_POINT ( 'NONE',  ( 19.18750000000004263, 0.8284271247462955401, 2.000000000000031530 ) ) ;
#27403 = CARTESIAN_POINT ( 'NONE',  ( -5.196152422706601826, 2.999999999999975131, -94.53867513459479710 ) ) ;
#27404 = FACE_OUTER_BOUND ( 'NONE', #1979, .T. ) ;
#27405 = FACE_OUTER_BOUND ( 'NONE', #8909, .T. ) ;
#27406 = ORIENTED_EDGE ( 'NONE', *, *, #19031, .T. ) ;
#27407 = AXIS2_PLACEMENT_3D ( 'NONE', #6296, #2000, #23059 ) ;
#27408 = CARTESIAN_POINT ( 'NONE',  ( 157.5937500000000284, 6.000000000000005329, 2.485281374238585972 ) ) ;
#27409 = CARTESIAN_POINT ( 'NONE',  ( 116.7502832217622171, -1.308140751793529510, 1.308140751793640533 ) ) ;
#27410 = CARTESIAN_POINT ( 'NONE',  ( 6.000000000000000888, 1.743066579297358182E-13, -55.58632486540519579 ) ) ;
#27411 = ORIENTED_EDGE ( 'NONE', *, *, #14553, .T. ) ;
#27412 = ORIENTED_EDGE ( 'NONE', *, *, #11869, .F. ) ;
#27413 = CARTESIAN_POINT ( 'NONE',  ( -4.763139720814407951, 2.749999999999946709, -94.25000000000000000 ) ) ;
#27414 = CARTESIAN_POINT ( 'NONE',  ( 0.000000000000000000, 0.000000000000000000, 0.000000000000000000 ) ) ;
#27415 = CARTESIAN_POINT ( 'NONE',  ( -3.608439182435115633, 6.249999999999965361, -111.3080127018922241 ) ) ;
#27416 = VERTEX_POINT ( 'NONE', #16197 ) ;
#27417 = CARTESIAN_POINT ( 'NONE',  ( -3.464101615137757051, -5.999999999999979572, -124.1636751345947829 ) ) ;
#27418 = CARTESIAN_POINT ( 'NONE',  ( 140.4778447815541256, -9.422006252106452706, -7.432744258808803295 ) ) ;
#27419 = CARTESIAN_POINT ( 'NONE',  ( 0.8353624398881696056, -15.41361754457665612, 8.287081578747827137 ) ) ;
#27420 = EDGE_CURVE ( 'NONE', #14683, #15286, #21033, .T. ) ;
#27421 = CARTESIAN_POINT ( 'NONE',  ( 7.216878364870455975, -6.409875621278545621E-14, -53.30801270189225960 ) ) ;
#27422 = ORIENTED_EDGE ( 'NONE', *, *, #1371, .T. ) ;
#27423 = CARTESIAN_POINT ( 'NONE',  ( 5.999999999999988454, 1.607695154586737729, -153.5966878364870638 ) ) ;
#27424 = SURFACE_STYLE_USAGE ( .BOTH. , #22700 ) ;
#27425 = AXIS2_PLACEMENT_3D ( 'NONE', #6282, #1204, #11078 ) ;
#27426 = DIRECTION ( 'NONE',  ( 1.000000000000000000, 0.000000000000000000, 0.000000000000000000 ) ) ;
#27427 = CARTESIAN_POINT ( 'NONE',  ( -3.175426480542816510, -5.500000000000057732, -164.3750000000000568 ) ) ;
#27428 = CARTESIAN_POINT ( 'NONE',  ( 115.9999999999998153, 2.500000000000002220, 2.220446049250313081E-13 ) ) ;
#27429 =( NAMED_UNIT ( * ) PLANE_ANGLE_UNIT ( ) SI_UNIT ( $, .RADIAN. ) );
#27430 = CARTESIAN_POINT ( 'NONE',  ( 159.9449251345948539, -5.500000000000012434, 2.278174593052012309 ) ) ;
#27431 = CARTESIAN_POINT ( 'NONE',  ( 5.196152422706629359, -2.999999999999988898, -165.7886751345948255 ) ) ;
#27432 = CARTESIAN_POINT ( 'NONE',  ( -6.350852961085760029, -1.281975124255709124E-13, -100.1250000000000568 ) ) ;
#27433 = CARTESIAN_POINT ( 'NONE',  ( 5.196152422706629359, -2.999999999999988898, -81.78867513459486815 ) ) ;
#27434 = ORIENTED_EDGE ( 'NONE', *, *, #11584, .T. ) ;
#27435 = CARTESIAN_POINT ( 'NONE',  ( 10.81250000000001243, 1.097466725451619718, 2.649519052838419153 ) ) ;
#27436 = CARTESIAN_POINT ( 'NONE',  ( 108.7502832217622881, -1.308140751793640533, 1.308140751793862577 ) ) ;
#27437 = EDGE_LOOP ( 'NONE', ( #3572, #16566, #28510, #21991, #919, #1694, #26729, #18854, #21588, #24558, #3386, #19394, #28873, #29458, #25289, #23331, #8227, #28074, #9110, #1776, #9662, #8786, #9157, #22184, #11267, #23022, #14267, #6264, #13005, #19472, #2726, #19449, #19801, #6151, #26066, #16748 ) ) ;
#27438 = CARTESIAN_POINT ( 'NONE',  ( 159.0000000000000284, -59.99999999999980105, -3.000000000000002665 ) ) ;
#27439 = CARTESIAN_POINT ( 'NONE',  ( -3.608439182435052128, -6.250000000000110134, -90.44198729810783277 ) ) ;
#27440 = AXIS2_PLACEMENT_3D ( 'NONE', #3852, #25351, #6476 ) ;
#27441 = CARTESIAN_POINT ( 'NONE',  ( 6.000000000000052403, -1.607695154586662678, -96.73066243270258724 ) ) ;
#27442 = ORIENTED_EDGE ( 'NONE', *, *, #9360, .T. ) ;
#27443 = CARTESIAN_POINT ( 'NONE',  ( 6.000000000000000888, 1.743066579297358182E-13, -65.16367513459479710 ) ) ;
#27444 = ORIENTED_EDGE ( 'NONE', *, *, #5486, .F. ) ;
#27445 = ORIENTED_EDGE ( 'NONE', *, *, #14978, .F. ) ;
#27446 = CARTESIAN_POINT ( 'NONE',  ( 159.1875000000000284, 4.242640687119269671, 4.242640687119298093 ) ) ;
#27447 = CARTESIAN_POINT ( 'NONE',  ( -3.175426480542816510, 5.499999999999865885, -118.3750000000000142 ) ) ;
#27448 = CARTESIAN_POINT ( 'NONE',  ( 2.775557561562891351E-14, -6.250000000000061284, -140.6830127018922099 ) ) ;
#27449 = ORIENTED_EDGE ( 'NONE', *, *, #11188, .F. ) ;
#27450 = CARTESIAN_POINT ( 'NONE',  ( 150.6636751345948255, 0.000000000000000000, 5.500000000000005329 ) ) ;
#27451 = CARTESIAN_POINT ( 'NONE',  ( 5.412658773652712085, -3.125000000000086153, -126.0669872981078328 ) ) ;
#27452 = CARTESIAN_POINT ( 'NONE',  ( -5.412658773652684552, -3.125000000000099920, -177.5669872981078186 ) ) ;
#27453 = FACE_OUTER_BOUND ( 'NONE', #11649, .T. ) ;
#27454 = EDGE_CURVE ( 'NONE', #8065, #7192, #24144, .T. ) ;
#27455 = ORIENTED_EDGE ( 'NONE', *, *, #24477, .F. ) ;
#27456 = CARTESIAN_POINT ( 'NONE',  ( 5.999999999999949374, 1.607695154586804565, -148.5193375672974696 ) ) ;
#27457 = DIRECTION ( 'NONE',  ( -1.665334536937730866E-16, 1.000000000000000000, 1.432813616264572524E-16 ) ) ;
#27458 = CARTESIAN_POINT ( 'NONE',  ( -1.110223024625164676E-16, 2.000000000000012879, 2.021286199229734960E-15 ) ) ;
#27459 = DIRECTION ( 'NONE',  ( 0.000000000000000000, 1.000000000000000000, 0.000000000000000000 ) ) ;
#27460 = CARTESIAN_POINT ( 'NONE',  ( 112.6252832217622597, 1.665334536937734811E-13, 1.849990392679745632 ) ) ;
#27461 = CARTESIAN_POINT ( 'NONE',  ( -3.608439182435115633, 6.249999999999965361, -72.94198729810781856 ) ) ;
#27462 = CARTESIAN_POINT ( 'NONE',  ( 2.775557561562891351E-14, 6.250000000000033751, -59.56698729810783277 ) ) ;
#27463 = DIRECTION ( 'NONE',  ( 1.000000000000000000, 0.000000000000000000, 0.000000000000000000 ) ) ;
#27464 = CARTESIAN_POINT ( 'NONE',  ( 0.000000000000000000, 5.499999999999991118, -48.00000000000004263 ) ) ;
#27465 = CARTESIAN_POINT ( 'NONE',  ( -1.000000000000002220, -9.000000000000007105, -4.000000000000005329 ) ) ;
#27466 = CARTESIAN_POINT ( 'NONE',  ( 0.000000000000000000, -5.999999999999991118, -47.53867513459481131 ) ) ;
#27467 = STYLED_ITEM ( 'NONE', ( #18710 ), #27156 ) ;
#27468 = EDGE_CURVE ( 'NONE', #2682, #10812, #25486, .T. ) ;
#27469 = CARTESIAN_POINT ( 'NONE',  ( -4.763139720814407951, -2.750000000000016431, -119.5000000000000568 ) ) ;
#27470 = EDGE_CURVE ( 'NONE', #28093, #4225, #8359, .T. ) ;
#27471 = CARTESIAN_POINT ( 'NONE',  ( 6.000000000000000888, 7.762456499804234384E-14, -138.6636751345948255 ) ) ;
#27472 = CARTESIAN_POINT ( 'NONE',  ( 104.7401757384972427, 0.2428654671893633876, -1.837968757803231101 ) ) ;
#27473 = ORIENTED_EDGE ( 'NONE', *, *, #8584, .F. ) ;
#27474 = CARTESIAN_POINT ( 'NONE',  ( -5.999999999999962697, 3.323446944526963891E-14, -157.4136751345948539 ) ) ;
#27475 = CYLINDRICAL_SURFACE ( 'NONE', #10166, 1.000000000000000000 ) ;
#27476 = CARTESIAN_POINT ( 'NONE',  ( -5.999999999999963585, -1.487416814333745711E-14, -96.83632486540520290 ) ) ;
#27477 = CARTESIAN_POINT ( 'NONE',  ( 140.8273502691896510, -5.000000000000004441, 0.000000000000000000 ) ) ;
#27478 = VERTEX_POINT ( 'NONE', #18788 ) ;
#27479 = CARTESIAN_POINT ( 'NONE',  ( 110.3122167782374419, -0.7662911109077388261, -1.849990392679411677 ) ) ;
#27480 = CARTESIAN_POINT ( 'NONE',  ( 124.9999999999999432, -65.00000000000000000, -7.500000000000007105 ) ) ;
#27481 = CARTESIAN_POINT ( 'NONE',  ( 113.3122167782374277, -0.7662911109077388261, -1.849990392679231599 ) ) ;
#27482 = CARTESIAN_POINT ( 'NONE',  ( -3.608439182435052128, -6.250000000000110134, -115.9419872981078328 ) ) ;
#27483 = CARTESIAN_POINT ( 'NONE',  ( 140.0769230769231228, -11.53846153846155254, -4.615384615384630074 ) ) ;
#27484 =( BOUNDED_CURVE ( )  B_SPLINE_CURVE ( 2, ( #30308, #8822, #27376, #27679, #20336, #9116, #13764, #27523, #29687 ),
 .UNSPECIFIED., .F., .T. ) 
 B_SPLINE_CURVE_WITH_KNOTS ( ( 3, 2, 2, 2, 3 ),
 ( 0.7343750000000000000, 0.7421875000000000000, 0.7500000000000000000, 0.7578125000000000000, 0.7656250000000000000 ),
 .UNSPECIFIED. ) 
 CURVE ( )  GEOMETRIC_REPRESENTATION_ITEM ( )  RATIONAL_B_SPLINE_CURVE ( ( 1.000000000000000000, 0.9238795325112867385, 1.000000000000000000, 0.9238795325112867385, 1.000000000000000000, 0.9238795325112867385, 1.000000000000000000, 0.9238795325112867385, 1.000000000000000000 ) ) 
 REPRESENTATION_ITEM ( '' )  );
#27485 = CARTESIAN_POINT ( 'NONE',  ( 110.5863248654050750, 1.414213562373145550, -1.414213562373145550 ) ) ;
#27486 = ORIENTED_EDGE ( 'NONE', *, *, #21116, .F. ) ;
#27487 = CARTESIAN_POINT ( 'NONE',  ( 21.77382486540523843, 2.500000000000084821, 1.035533905932689347 ) ) ;
#27488 = CARTESIAN_POINT ( 'NONE',  ( 140.4375000000000284, -4.242640687119298093, -4.242640687119298093 ) ) ;
#27489 = AXIS2_PLACEMENT_3D ( 'NONE', #2178, #11581, #16497 ) ;
#27490 =( BOUNDED_CURVE ( )  B_SPLINE_CURVE ( 2, ( #16188, #8936, #21219, #13889, #161, #30264, #12027, #18777, #28097 ),
 .UNSPECIFIED., .F., .T. ) 
 B_SPLINE_CURVE_WITH_KNOTS ( ( 3, 2, 2, 2, 3 ),
 ( 0.1406250000000000000, 0.1484375000000000000, 0.1562500000000000000, 0.1640625000000000000, 0.1718750000000000000 ),
 .UNSPECIFIED. ) 
 CURVE ( )  GEOMETRIC_REPRESENTATION_ITEM ( )  RATIONAL_B_SPLINE_CURVE ( ( 1.000000000000000000, 0.9238795325112867385, 1.000000000000000000, 0.9238795325112867385, 1.000000000000000000, 0.9238795325112867385, 1.000000000000000000, 0.9238795325112867385, 1.000000000000000000 ) ) 
 REPRESENTATION_ITEM ( '' )  );
#27491 = CIRCLE ( 'NONE', #11374, 0.5000000000000004441 ) ;
#27492 = VERTEX_POINT ( 'NONE', #7083 ) ;
#27493 = ORIENTED_EDGE ( 'NONE', *, *, #12965, .T. ) ;
#27494 = MECHANICAL_DESIGN_GEOMETRIC_PRESENTATION_REPRESENTATION (  '', ( #7894 ), #5918 ) ;
#27495 = CARTESIAN_POINT ( 'NONE',  ( -27.00000000000002487, 0.000000000000000000, 0.000000000000000000 ) ) ;
#27496 = CARTESIAN_POINT ( 'NONE',  ( 14.85117513459496408, -2.499999999999904521, -1.035533905932809473 ) ) ;
#27497 = EDGE_CURVE ( 'NONE', #1194, #19618, #16744, .T. ) ;
#27498 = CARTESIAN_POINT ( 'NONE',  ( 21.81250000000009592, 0.8284271247462955401, -2.000000000000151879 ) ) ;
#27499 = DIRECTION ( 'NONE',  ( 0.000000000000000000, 0.000000000000000000, 1.000000000000000000 ) ) ;
#27500 = CARTESIAN_POINT ( 'NONE',  ( 6.000000000000000888, -1.607695154586752384, -79.65331216351296462 ) ) ;
#27501 = CARTESIAN_POINT ( 'NONE',  ( -5.412658773652684552, -3.125000000000099920, -68.93301270189222407 ) ) ;
#27502 = AXIS2_PLACEMENT_3D ( 'NONE', #13884, #9381, #4149 ) ;
#27503 = CARTESIAN_POINT ( 'NONE',  ( 148.6726497308104058, -5.000000000000004441, 0.000000000000000000 ) ) ;
#27504 = DIRECTION ( 'NONE',  ( 0.000000000000000000, 0.000000000000000000, -1.000000000000000000 ) ) ;
#27505 = CARTESIAN_POINT ( 'NONE',  ( 0.7669223171414760731, -14.69693845669906018, 7.500000000000007105 ) ) ;
#27506 = CARTESIAN_POINT ( 'NONE',  ( -5.999999999999968026, -1.607695154586722186, -155.8466878364870070 ) ) ;
#27507 = ADVANCED_FACE ( 'NONE', ( #2335 ), #3427, .T. ) ;
#27508 = CARTESIAN_POINT ( 'NONE',  ( 3.175426480543072749, -5.500000000000105693, -122.1250000000000426 ) ) ;
#27509 = LINE ( 'NONE', #1878, #24030 ) ;
#27510 = DIRECTION ( 'NONE',  ( 5.551115123125785167E-17, -1.000000000000000000, -8.881784197001256268E-16 ) ) ;
#27511 = ORIENTED_EDGE ( 'NONE', *, *, #9293, .T. ) ;
#27512 = VECTOR ( 'NONE', #8511, 1000.000000000000000 ) ;
#27513 = CARTESIAN_POINT ( 'NONE',  ( 3.175426480543072749, -5.500000000000105693, -65.12500000000001421 ) ) ;
#27514 = CARTESIAN_POINT ( 'NONE',  ( -5.999999999999956479, -1.607695154586745057, -154.3466878364870638 ) ) ;
#27515 = CARTESIAN_POINT ( 'NONE',  ( 6.000000000000052403, -1.607695154586662678, -76.65331216351299304 ) ) ;
#27516 = CARTESIAN_POINT ( 'NONE',  ( -3.464101615137757051, -5.999999999999979572, -163.1636751345947687 ) ) ;
#27517 = ORIENTED_EDGE ( 'NONE', *, *, #25214, .F. ) ;
#27518 = VECTOR ( 'NONE', #28899, 1000.000000000000000 ) ;
#27519 = CARTESIAN_POINT ( 'NONE',  ( 105.1874999999998437, 1.035533905932749299, 2.500000000000265121 ) ) ;
#27520 = CARTESIAN_POINT ( 'NONE',  ( 147.0937500000000284, 6.000000000000005329, 2.485281374238585972 ) ) ;
#27521 = CARTESIAN_POINT ( 'NONE',  ( 12.75000000000017764, 1.665334536937734811E-13, -2.000000000000001776 ) ) ;
#27522 = CARTESIAN_POINT ( 'NONE',  ( 138.0937500000000284, 6.000000000000005329, 2.485281374238585972 ) ) ;
#27523 = CARTESIAN_POINT ( 'NONE',  ( 21.97617513459486460, -1.035533905932749299, -2.499999999999964473 ) ) ;
#27524 = ORIENTED_EDGE ( 'NONE', *, *, #24562, .F. ) ;
#27525 = TOROIDAL_SURFACE ( 'NONE', #11412, 28.99999999999999645, 1.000000000000000000 ) ;
#27526 = CARTESIAN_POINT ( 'NONE',  ( -2.775557561562891351E-14, -5.500000000000115463, -140.2500000000000000 ) ) ;
#27527 = CARTESIAN_POINT ( 'NONE',  ( 13.93750000000017941, 2.000000000000151879, -0.8284271247462354770 ) ) ;
#27528 = VERTEX_POINT ( 'NONE', #1865 ) ;
#27529 = CARTESIAN_POINT ( 'NONE',  ( 3.175426480543072749, 5.499999999999865885, -73.62500000000005684 ) ) ;
#27530 = PRESENTATION_LAYER_ASSIGNMENT (  '', '', ( #24109 ) ) ;
#27531 = EDGE_CURVE ( 'NONE', #2984, #20340, #19240, .T. ) ;
#27532 = DIRECTION ( 'NONE',  ( -7.147005652999508048E-36, 5.642372883946980038E-36, 1.000000000000000000 ) ) ;
#27533 = EDGE_CURVE ( 'NONE', #2252, #1389, #617, .T. ) ;
#27534 = CARTESIAN_POINT ( 'NONE',  ( -1.965048709171653751, -10.82948053518398979, -19.31713205297533520 ) ) ;
#27535 = CARTESIAN_POINT ( 'NONE',  ( 6.000000000000000888, 1.743066579297358182E-13, -83.16367513459481131 ) ) ;
#27536 = CARTESIAN_POINT ( 'NONE',  ( 112.7886751345947403, -1.999999999999946265, 0.000000000000000000 ) ) ;
#27537 = DIRECTION ( 'NONE',  ( 0.000000000000000000, 0.000000000000000000, -1.000000000000000000 ) ) ;
#27538 = CARTESIAN_POINT ( 'NONE',  ( 110.6011751345947260, -0.8284271247461453269, 2.000000000000271783 ) ) ;
#27539 = DIRECTION ( 'NONE',  ( 1.000000000000000000, 0.000000000000000000, 0.000000000000000000 ) ) ;
#27540 = CARTESIAN_POINT ( 'NONE',  ( -6.350852961085760029, -1.281975124255709124E-13, -149.6250000000000284 ) ) ;
#27541 = CARTESIAN_POINT ( 'NONE',  ( -0.01290326774830613359, -14.38393108808779175, -8.362582996346231923 ) ) ;
#27542 = VECTOR ( 'NONE', #9522, 1000.000000000000000 ) ;
#27543 = CARTESIAN_POINT ( 'NONE',  ( -2.775557561562891351E-14, -5.500000000000115463, -86.25000000000004263 ) ) ;
#27544 = CYLINDRICAL_SURFACE ( 'NONE', #18925, 6.000000000000000888 ) ;
#27545 = CARTESIAN_POINT ( 'NONE',  ( 4.763139720814407951, -2.749999999999988454, -75.50000000000001421 ) ) ;
#27546 = CARTESIAN_POINT ( 'NONE',  ( -19.99999999999998224, -54.99999999999990763, 5.000000000000004441 ) ) ;
#27547 = LINE ( 'NONE', #6524, #20602 ) ;
#27548 = CARTESIAN_POINT ( 'NONE',  ( 135.5000000000000000, -9.047800747817552391, 8.000000000000007105 ) ) ;
#27549 = CARTESIAN_POINT ( 'NONE',  ( 135.4709958594519037, -8.959870900750173561, -7.999999999999970690 ) ) ;
#27550 = CARTESIAN_POINT ( 'NONE',  ( 114.3988248654049755, -0.8284271247461453269, -1.999999999999791278 ) ) ;
#27551 = CARTESIAN_POINT ( 'NONE',  ( 19.06250000000013500, 2.000000000000091926, 0.8284271247461753029 ) ) ;
#27552 = CARTESIAN_POINT ( 'NONE',  ( 150.8363248654052029, 0.000000000000000000, -5.500000000000005329 ) ) ;
#27553 = CARTESIAN_POINT ( 'NONE',  ( 5.999999999999949374, 1.607695154586804565, -139.5193375672973843 ) ) ;
#27554 = ORIENTED_EDGE ( 'NONE', *, *, #11968, .T. ) ;
#27555 = CARTESIAN_POINT ( 'NONE',  ( 154.0312500000000568, -2.485281374238555774, -6.000000000000005329 ) ) ;
#27556 = AXIS2_PLACEMENT_3D ( 'NONE', #12525, #29049, #17422 ) ;
#27557 = CYLINDRICAL_SURFACE ( 'NONE', #1342, 6.000000000000000888 ) ;
#27558 = ORIENTED_EDGE ( 'NONE', *, *, #9647, .F. ) ;
#27559 = ORIENTED_EDGE ( 'NONE', *, *, #28511, .T. ) ;
#27560 = ORIENTED_EDGE ( 'NONE', *, *, #11975, .T. ) ;
#27561 = CARTESIAN_POINT ( 'NONE',  ( -6.350852961085760029, -1.281975124255709124E-13, -97.12500000000004263 ) ) ;
#27562 = CARTESIAN_POINT ( 'NONE',  ( 0.000000000000000000, 5.999999999999977796, -96.28867513459482552 ) ) ;
#27563 = ADVANCED_FACE ( 'NONE', ( #12626 ), #5062, .T. ) ;
#27564 = CARTESIAN_POINT ( 'NONE',  ( 2.775557561562891351E-14, 6.250000000000033751, -109.9330127018922667 ) ) ;
#27565 = ORIENTED_EDGE ( 'NONE', *, *, #19693, .T. ) ;
#27566 = CARTESIAN_POINT ( 'NONE',  ( 119.2886751345947260, 1.999999999999946265, 1.110223024625156540E-13 ) ) ;
#27567 = FACE_OUTER_BOUND ( 'NONE', #18257, .T. ) ;
#27568 = CARTESIAN_POINT ( 'NONE',  ( -4.763139720814407951, 2.749999999999946709, -164.7500000000000000 ) ) ;
#27569 = CARTESIAN_POINT ( 'NONE',  ( -5.999999999999963585, -1.487416814333745711E-14, -106.4136751345948113 ) ) ;
#27570 = ORIENTED_EDGE ( 'NONE', *, *, #1506, .T. ) ;
#27571 = CARTESIAN_POINT ( 'NONE',  ( 3.464101615137852974, 5.999999999999884537, -160.3363248654052313 ) ) ;
#27572 =( BOUNDED_CURVE ( )  B_SPLINE_CURVE ( 2, ( #20270, #24856, #20565, #16148, #8893, #4419, #1812, #9042, #27443 ),
 .UNSPECIFIED., .F., .T. ) 
 B_SPLINE_CURVE_WITH_KNOTS ( ( 3, 2, 2, 2, 3 ),
 ( 0.8583333333333332815, 0.8592592592592592782, 0.8611111111111111605, 0.8629629629629629317, 0.8638888888888889284 ),
 .UNSPECIFIED. ) 
 CURVE ( )  GEOMETRIC_REPRESENTATION_ITEM ( )  RATIONAL_B_SPLINE_CURVE ( ( 0.9330127018922194093, 0.9330127018922154125, 1.000000000000000000, 0.8660254037844388186, 1.000000000000000000, 0.8660254037844388186, 1.000000000000000000, 0.9330127018922154125, 0.9330127018922194093 ) ) 
 REPRESENTATION_ITEM ( '' )  );
#27573 = CARTESIAN_POINT ( 'NONE',  ( 140.5000000000000284, -9.422078944634874276, 7.437228073820182139 ) ) ;
#27574 = CARTESIAN_POINT ( 'NONE',  ( 4.763139720814407951, 2.750000000000002665, -162.2500000000000000 ) ) ;
#27575 = CARTESIAN_POINT ( 'NONE',  ( 116.3124999999997158, -1.035533905932598975, 2.500000000000144773 ) ) ;
#27576 = CARTESIAN_POINT ( 'NONE',  ( 4.763139720814407951, 2.750000000000002665, -111.2500000000000142 ) ) ;
#27577 = CARTESIAN_POINT ( 'NONE',  ( 23.77382486540529882, 2.500000000000144773, 1.035533905932689347 ) ) ;
#27578 = DIRECTION ( 'NONE',  ( 1.000000000000000000, -5.551115123125774074E-17, 0.000000000000000000 ) ) ;
#27579 = CARTESIAN_POINT ( 'NONE',  ( 0.000000000000000000, 5.499999999999991118, -100.5000000000000284 ) ) ;
#27580 = COLOUR_RGB ( '', 0.72549020, 0.75294118, 0.79215686) ;
#27581 = CARTESIAN_POINT ( 'NONE',  ( 158.8273502691896510, -5.000000000000004441, 0.000000000000000000 ) ) ;
#27582 = CARTESIAN_POINT ( 'NONE',  ( -6.000000000000000888, 1.067854986875958443E-15, 7.560779664488942560E-35 ) ) ;
#27583 = CARTESIAN_POINT ( 'NONE',  ( -0.08237205255902971257, -15.17882982317237150, 7.764958073340198830 ) ) ;
#27584 = VERTEX_POINT ( 'NONE', #25971 ) ;
#27585 = CARTESIAN_POINT ( 'NONE',  ( 12.62500000000010836, 2.649519052838555933, -5.551115123125782702E-14 ) ) ;
#27586 = CARTESIAN_POINT ( 'NONE',  ( 115.1874999999998437, 1.035533905932719101, 2.500000000000265121 ) ) ;
#27587 = CARTESIAN_POINT ( 'NONE',  ( 6.000000000000000888, -1.859271017917181981E-14, -130.5863248654052313 ) ) ;
#27588 = CARTESIAN_POINT ( 'NONE',  ( 112.1877832217621886, 0.7662911109079189043, -1.849990392679291551 ) ) ;
#27589 = CARTESIAN_POINT ( 'NONE',  ( 161.0173279456235207, 2.969419107450559814, 4.660845171074455173 ) ) ;
#27590 = ORIENTED_EDGE ( 'NONE', *, *, #17989, .T. ) ;
#27591 = CARTESIAN_POINT ( 'NONE',  ( 6.000000000000000888, -3.330669073875464691E-16, -7.560779664488942560E-35 ) ) ;
#27592 = CARTESIAN_POINT ( 'NONE',  ( 108.1247167782375556, -1.849990392679468076, 2.220446049250313081E-13 ) ) ;
#27593 = EDGE_CURVE ( 'NONE', #21900, #30382, #16273, .T. ) ;
#27594 = CARTESIAN_POINT ( 'NONE',  ( -5.412658773652739619, 3.124999999999975131, -86.31698729810783277 ) ) ;
#27595 = ORIENTED_EDGE ( 'NONE', *, *, #10802, .F. ) ;
#27596 = CARTESIAN_POINT ( 'NONE',  ( -1.581364418632495106, 10.89278420593271157, -30.80148057605384793 ) ) ;
#27597 = ORIENTED_EDGE ( 'NONE', *, *, #25688, .T. ) ;
#27598 = CARTESIAN_POINT ( 'NONE',  ( 152.4375000000000284, -4.242640687119298093, -4.242640687119298093 ) ) ;
#27599 = ORIENTED_EDGE ( 'NONE', *, *, #2389, .F. ) ;
#27600 = CARTESIAN_POINT ( 'NONE',  ( 6.350852961086080661, -9.614813431917819062E-14, -121.8750000000000426 ) ) ;
#27601 = CARTESIAN_POINT ( 'NONE',  ( 22.87500000000008882, -2.649519052838111843, 0.000000000000000000 ) ) ;
#27602 = AXIS2_PLACEMENT_3D ( 'NONE', #28936, #8677, #2074 ) ;
#27603 = EDGE_CURVE ( 'NONE', #20871, #12019, #15766, .T. ) ;
#27604 = CARTESIAN_POINT ( 'NONE',  ( 3.608439182435180470, -6.249999999999997335, -131.5580127018922383 ) ) ;
#27605 = ORIENTED_EDGE ( 'NONE', *, *, #15085, .T. ) ;
#27606 = DIRECTION ( 'NONE',  ( 1.000000000000000000, 0.000000000000000000, 0.000000000000000000 ) ) ;
#27607 = CARTESIAN_POINT ( 'NONE',  ( -3.608439182435052128, -6.250000000000110134, -123.4419872981078043 ) ) ;
#27608 = CARTESIAN_POINT ( 'NONE',  ( 3.608439182435180470, -6.249999999999997335, -178.6919872981078470 ) ) ;
#27609 = CARTESIAN_POINT ( 'NONE',  ( 159.0000000000000284, -12.00000000000001066, 4.000000000000004441 ) ) ;
#27610 = DIRECTION ( 'NONE',  ( 2.220446049250313574E-16, 8.881784197001254296E-16, -1.000000000000000000 ) ) ;
#27611 = ORIENTED_EDGE ( 'NONE', *, *, #13141, .T. ) ;
#27612 = CARTESIAN_POINT ( 'NONE',  ( 11.31250000000006395, -0.8284271247460552878, 2.000000000000031530 ) ) ;
#27613 = DIRECTION ( 'NONE',  ( -1.000000000000000000, -1.665334536937736783E-16, -2.220446049250315546E-16 ) ) ;
#27614 = CARTESIAN_POINT ( 'NONE',  ( -20.99999999999998224, -54.99999999999990763, -4.000000000000003553 ) ) ;
#27615 = FACE_OUTER_BOUND ( 'NONE', #26074, .T. ) ;
#27616 =( BOUNDED_CURVE ( )  B_SPLINE_CURVE ( 2, ( #26889, #13133, #15269, #17726, #3394, #12821, #20169, #22163, #24598 ),
 .UNSPECIFIED., .F., .T. ) 
 B_SPLINE_CURVE_WITH_KNOTS ( ( 3, 2, 2, 2, 3 ),
 ( 0.9361111111111111160, 0.9370370370370370017, 0.9388888888888888840, 0.9407407407407407662, 0.9416666666666666519 ),
 .UNSPECIFIED. ) 
 CURVE ( )  GEOMETRIC_REPRESENTATION_ITEM ( )  RATIONAL_B_SPLINE_CURVE ( ( 0.9330127018922194093, 0.9330127018922194093, 1.000000000000000000, 0.8660254037844388186, 1.000000000000000000, 0.8660254037844388186, 1.000000000000000000, 0.9330127018922234061, 0.9330127018922194093 ) ) 
 REPRESENTATION_ITEM ( '' )  );
#27617 = CARTESIAN_POINT ( 'NONE',  ( 5.196152422706629359, -2.999999999999988898, -150.2113248654052313 ) ) ;
#27618 = CARTESIAN_POINT ( 'NONE',  ( 110.8752832217622029, -1.849990392679495832, 0.000000000000000000 ) ) ;
#27619 = CARTESIAN_POINT ( 'NONE',  ( 5.412658773652712085, -3.125000000000086153, -72.06698729810784698 ) ) ;
#27620 = CARTESIAN_POINT ( 'NONE',  ( 7.216878364870455975, -6.409875621278545621E-14, -58.44198729810781856 ) ) ;
#27621 = CARTESIAN_POINT ( 'NONE',  ( 0.000000000000000000, -5.999999999999991118, -170.5386751345947971 ) ) ;
#27622 = CARTESIAN_POINT ( 'NONE',  ( 4.763139720814407951, -2.749999999999988454, -48.49999999999998579 ) ) ;
#27623 = CARTESIAN_POINT ( 'NONE',  ( 140.5000000000000284, -9.599999999999997868, -7.200000000000011724 ) ) ;
#27624 = CARTESIAN_POINT ( 'NONE',  ( 4.763139720814407951, -2.749999999999988454, -122.0000000000000000 ) ) ;
#27625 = CARTESIAN_POINT ( 'NONE',  ( 116.0000000000000142, 0.000000000000000000, 0.000000000000000000 ) ) ;
#27626 = AXIS2_PLACEMENT_3D ( 'NONE', #17654, #4095, #11044 ) ;
#27627 = EDGE_LOOP ( 'NONE', ( #13802, #13045, #9043, #13912 ) ) ;
#27628 = CARTESIAN_POINT ( 'NONE',  ( 19.87500000000008527, 1.665334536937734811E-13, 2.649519052838278377 ) ) ;
#27629 =( BOUNDED_CURVE ( )  B_SPLINE_CURVE ( 2, ( #4119, #13240, #22880, #22583, #27308, #19052, #25465, #18591, #23648 ),
 .UNSPECIFIED., .F., .F. ) 
 B_SPLINE_CURVE_WITH_KNOTS ( ( 3, 2, 2, 2, 3 ),
 ( 0.9194444444444445086, 0.9203703703703703942, 0.9222222222222222765, 0.9240740740740740478, 0.9249999999999999334 ),
 .UNSPECIFIED. ) 
 CURVE ( )  GEOMETRIC_REPRESENTATION_ITEM ( )  RATIONAL_B_SPLINE_CURVE ( ( 0.9330127018922194093, 0.9330127018922234061, 1.000000000000000000, 0.8660254037844388186, 1.000000000000000000, 0.8660254037844388186, 1.000000000000000000, 0.9330127018922234061, 0.9330127018922194093 ) ) 
 REPRESENTATION_ITEM ( '' )  );
#27630 = CARTESIAN_POINT ( 'NONE',  ( 143.6324251345948824, -5.500000000000012434, -2.278174593052012309 ) ) ;
#27631 = DIRECTION ( 'NONE',  ( 1.000000000000000000, 0.000000000000000000, 0.000000000000000000 ) ) ;
#27632 = CARTESIAN_POINT ( 'NONE',  ( 139.5148502691896510, -3.535533905932725318, -3.535533905932725318 ) ) ;
#27633 = ORIENTED_EDGE ( 'NONE', *, *, #26134, .F. ) ;
#27634 = CARTESIAN_POINT ( 'NONE',  ( 111.5622167782373566, 1.849990392679591977, -0.7662911109075283278 ) ) ;
#27635 = CARTESIAN_POINT ( 'NONE',  ( 6.000000000000000000, 2.951592740943527306E-14, -164.1636751345948824 ) ) ;
#27636 = CARTESIAN_POINT ( 'NONE',  ( 111.3747167782376692, -5.551115123125782702E-14, -1.849990392679523588 ) ) ;
#27637 = EDGE_CURVE ( 'NONE', #11496, #21299, #6662, .T. ) ;
#27638 = CARTESIAN_POINT ( 'NONE',  ( 2.775557561562891351E-14, 6.250000000000033751, -116.5669872981078328 ) ) ;
#27639 = CARTESIAN_POINT ( 'NONE',  ( -5.999999999999963585, 1.780251999655701777E-13, -107.9136751345948397 ) ) ;
#27640 = CARTESIAN_POINT ( 'NONE',  ( 130.0000000000000284, -60.00000000000001421, -3.000000000000002665 ) ) ;
#27641 = EDGE_LOOP ( 'NONE', ( #19626, #14691, #22837, #14083 ) ) ;
#27642 = ORIENTED_EDGE ( 'NONE', *, *, #7275, .T. ) ;
#27643 = CARTESIAN_POINT ( 'NONE',  ( 21.89882486540523843, 1.035533905932869425, 2.499999999999844569 ) ) ;
#27644 = CARTESIAN_POINT ( 'NONE',  ( 144.0937500000000000, 6.000000000000005329, 2.485281374238585972 ) ) ;
#27645 = ADVANCED_FACE ( 'NONE', ( #26560 ), #3062, .T. ) ;
#27646 = CARTESIAN_POINT ( 'NONE',  ( -5.412658773652739619, 3.124999999999975131, -50.31698729810785409 ) ) ;
#27647 = VERTEX_POINT ( 'NONE', #28859 ) ;
#27648 = CARTESIAN_POINT ( 'NONE',  ( -5.412658773652684552, -3.125000000000099920, -144.5669872981077901 ) ) ;
#27649 = ORIENTED_EDGE ( 'NONE', *, *, #19363, .F. ) ;
#27650 = AXIS2_PLACEMENT_3D ( 'NONE', #15585, #21077, #16646 ) ;
#27651 = LINE ( 'NONE', #23237, #2298 ) ;
#27652 = CARTESIAN_POINT ( 'NONE',  ( 21.31250000000010658, -0.8284271247460552878, 1.999999999999971800 ) ) ;
#27653 = DIRECTION ( 'NONE',  ( 0.000000000000000000, 1.000000000000000000, 0.000000000000000000 ) ) ;
#27654 = CARTESIAN_POINT ( 'NONE',  ( 104.9999999999999716, -0.4876318259226519736, 1.939643060552054266 ) ) ;
#27655 = CARTESIAN_POINT ( 'NONE',  ( 5.412658773652739619, 3.124999999999988898, -63.68301270189225249 ) ) ;
#27656 = CARTESIAN_POINT ( 'NONE',  ( 141.8288997308104058, 4.999999999999989342, -2.071067811865468400 ) ) ;
#27657 = CARTESIAN_POINT ( 'NONE',  ( 111.9136751345946692, -1.414213562373145550, -1.414213562373034527 ) ) ;
#27658 = LINE ( 'NONE', #14204, #7912 ) ;
#27659 = CARTESIAN_POINT ( 'NONE',  ( -5.999999999999963585, -1.487416814333745711E-14, -170.3363248654052313 ) ) ;
#27660 = CARTESIAN_POINT ( 'NONE',  ( 135.0000000000000284, 0.000000000000000000, 0.000000000000000000 ) ) ;
#27661 = CARTESIAN_POINT ( 'NONE',  ( 108.9374999999997300, 2.500000000000115019, -1.035533905932508825 ) ) ;
#27662 = CARTESIAN_POINT ( 'NONE',  ( -3.175426480542816066, -5.500000000000057732, -123.8749999999999858 ) ) ;
#27663 = DIRECTION ( 'NONE',  ( 1.000000000000000000, -5.551115123125773458E-17, -1.260129944081490338E-35 ) ) ;
#27664 = CARTESIAN_POINT ( 'NONE',  ( -3.608439182435115633, 6.249999999999965361, -144.3080127018922383 ) ) ;
#27665 = CARTESIAN_POINT ( 'NONE',  ( 24.99999999999999289, 1.110223024625156540E-13, -2.220446049250313081E-13 ) ) ;
#27666 =( LENGTH_UNIT ( ) NAMED_UNIT ( * ) SI_UNIT ( .MILLI., .METRE. ) );
#27667 = ORIENTED_EDGE ( 'NONE', *, *, #20291, .F. ) ;
#27668 = CARTESIAN_POINT ( 'NONE',  ( -3.175426480542816066, -5.500000000000057732, -54.87500000000003553 ) ) ;
#27669 = CYLINDRICAL_SURFACE ( 'NONE', #6063, 4.000000000000004441 ) ;
#27670 = CARTESIAN_POINT ( 'NONE',  ( -3.464101615137725076, 5.999999999999979572, -172.0863248654052029 ) ) ;
#27671 =( BOUNDED_CURVE ( )  B_SPLINE_CURVE ( 2, ( #21348, #9673, #19063, #26092, #5032, #433, #9822, #19198, #28527 ),
 .UNSPECIFIED., .F., .T. ) 
 B_SPLINE_CURVE_WITH_KNOTS ( ( 3, 2, 2, 2, 3 ),
 ( 0.2194444444444444420, 0.2203703703703703276, 0.2222222222222222099, 0.2240740740740740922, 0.2249999999999999778 ),
 .UNSPECIFIED. ) 
 CURVE ( )  GEOMETRIC_REPRESENTATION_ITEM ( )  RATIONAL_B_SPLINE_CURVE ( ( 0.9330127018922194093, 0.9330127018922194093, 1.000000000000000000, 0.8660254037844388186, 1.000000000000000000, 0.8660254037844388186, 1.000000000000000000, 0.9330127018922234061, 0.9330127018922194093 ) ) 
 REPRESENTATION_ITEM ( '' )  );
#27672 = CARTESIAN_POINT ( 'NONE',  ( -5.999999999999962697, 3.323446944526963891E-14, -163.4136751345948539 ) ) ;
#27673 = ORIENTED_EDGE ( 'NONE', *, *, #195, .F. ) ;
#27674 = CARTESIAN_POINT ( 'NONE',  ( 119.8747167782375982, 0.000000000000000000, 1.849990392679523588 ) ) ;
#27675 = CARTESIAN_POINT ( 'NONE',  ( 137.8125000000000284, 4.242640687119298093, -4.242640687119298093 ) ) ;
#27676 = EDGE_CURVE ( 'NONE', #22801, #10034, #19087, .T. ) ;
#27677 = CARTESIAN_POINT ( 'NONE',  ( -6.000000000000000888, 1.067854986875958443E-15, 7.560779664488942560E-35 ) ) ;
#27678 = CARTESIAN_POINT ( 'NONE',  ( 140.3437500000000284, -6.000000000000005329, -2.485281374238555774 ) ) ;
#27679 = CARTESIAN_POINT ( 'NONE',  ( 21.72617513459489658, -2.499999999999904521, 1.035533905932689347 ) ) ;
#27680 = EDGE_CURVE ( 'NONE', #16791, #27492, #28610, .T. ) ;
#27681 = CARTESIAN_POINT ( 'NONE',  ( 3.175426480543072749, -5.500000000000105693, -140.1250000000000000 ) ) ;
#27682 = CARTESIAN_POINT ( 'NONE',  ( 15.06250000000016342, 2.000000000000151879, 0.8284271247461153509 ) ) ;
#27683 = ORIENTED_EDGE ( 'NONE', *, *, #6677, .T. ) ;
#27684 = CARTESIAN_POINT ( 'NONE',  ( 3.175426480543072749, 5.499999999999865885, -66.12500000000002842 ) ) ;
#27685 = CARTESIAN_POINT ( 'NONE',  ( 18.46132486540535922, 1.665334536937734811E-13, -2.500000000000113243 ) ) ;
#27686 = CARTESIAN_POINT ( 'NONE',  ( -5.999999999999963585, -1.487416814333745711E-14, -139.4136751345948255 ) ) ;
#27687 = CARTESIAN_POINT ( 'NONE',  ( 0.000000000000000000, 0.000000000000000000, 0.000000000000000000 ) ) ;
#27688 = DIRECTION ( 'NONE',  ( -1.000000000000000000, -1.665334536937736783E-16, -2.220446049250315546E-16 ) ) ;
#27689 = DIRECTION ( 'NONE',  ( 1.000000000000000000, 0.000000000000000000, 0.000000000000000000 ) ) ;
#27690 = CARTESIAN_POINT ( 'NONE',  ( 118.1877832217622029, 0.7662911109078588412, -1.849990392679351725 ) ) ;
#27691 = CARTESIAN_POINT ( 'NONE',  ( 3.175426480543072749, 5.499999999999865885, -151.6250000000000284 ) ) ;
#27692 = FACE_OUTER_BOUND ( 'NONE', #7222, .T. ) ;
#27693 = CARTESIAN_POINT ( 'NONE',  ( -2.775557561562891351E-14, -5.500000000000115463, -141.7500000000000568 ) ) ;
#27694 = CARTESIAN_POINT ( 'NONE',  ( -5.412658773652739619, 3.124999999999975131, -163.6830127018922383 ) ) ;
#27695 = FACE_OUTER_BOUND ( 'NONE', #8349, .T. ) ;
#27696 = CARTESIAN_POINT ( 'NONE',  ( 6.350852961086080661, -9.614813431917819062E-14, -79.87500000000001421 ) ) ;
#27697 = CARTESIAN_POINT ( 'NONE',  ( 0.000000000000000000, 0.000000000000000000, 0.000000000000000000 ) ) ;
#27698 = CARTESIAN_POINT ( 'NONE',  ( -3.175426480542816510, 5.499999999999865885, -76.37500000000001421 ) ) ;
#27699 = CARTESIAN_POINT ( 'NONE',  ( 0.000000000000000000, -5.999999999999991118, -74.53867513459483973 ) ) ;
#27700 = VECTOR ( 'NONE', #27247, 1000.000000000000000 ) ;
#27701 = CARTESIAN_POINT ( 'NONE',  ( 160.9613248654052029, -5.500000000000005329, 0.000000000000000000 ) ) ;
#27702 = CARTESIAN_POINT ( 'NONE',  ( 135.0000000000000284, 1.949781249179022291, 5.142796231657420947 ) ) ;
#27703 = CARTESIAN_POINT ( 'NONE',  ( -3.464101615137757051, -5.999999999999979572, -71.66367513459481131 ) ) ;
#27704 = CARTESIAN_POINT ( 'NONE',  ( 18.56250000000005329, -1.999999999999971800, -0.8284271247462354770 ) ) ;
#27705 = AXIS2_PLACEMENT_3D ( 'NONE', #21626, #26355, #5306 ) ;
#27706 = CARTESIAN_POINT ( 'NONE',  ( -5.999999999999963585, 8.134310703387671600E-14, -145.4136751345948539 ) ) ;
#27707 = EDGE_CURVE ( 'NONE', #25500, #21299, #17997, .T. ) ;
#27708 = CARTESIAN_POINT ( 'NONE',  ( 116.1247167782375556, -1.849990392679468076, 1.110223024625156540E-13 ) ) ;
#27709 = CARTESIAN_POINT ( 'NONE',  ( -5.999999999999963585, 1.780251999655701777E-13, -83.91367513459482552 ) ) ;
#27710 = ADVANCED_FACE ( 'NONE', ( #5660 ), #24539, .T. ) ;
#27711 = ORIENTED_EDGE ( 'NONE', *, *, #18921, .F. ) ;
#27712 = CARTESIAN_POINT ( 'NONE',  ( 157.2187500000000284, 2.485281374238555774, -6.000000000000005329 ) ) ;
#27713 = DIRECTION ( 'NONE',  ( 0.000000000000000000, -1.000000000000000000, 0.000000000000000000 ) ) ;
#27714 = DIRECTION ( 'NONE',  ( 1.000000000000000000, -5.551115123125773458E-17, -1.260129944081490338E-35 ) ) ;
#27715 = ORIENTED_EDGE ( 'NONE', *, *, #873, .F. ) ;
#27716 = TOROIDAL_SURFACE ( 'NONE', #20888, 12.50000000000000000, 5.000000000000000000 ) ;
#27717 = ORIENTED_EDGE ( 'NONE', *, *, #12334, .F. ) ;
#27718 = VECTOR ( 'NONE', #15379, 1000.000000000000000 ) ;
#27719 = ORIENTED_EDGE ( 'NONE', *, *, #9291, .F. ) ;
#27720 = CARTESIAN_POINT ( 'NONE',  ( -4.763139720814407951, 2.749999999999946709, -92.75000000000000000 ) ) ;
#27721 = CARTESIAN_POINT ( 'NONE',  ( -5.412658773652684552, -3.125000000000099920, -103.4330127018922525 ) ) ;
#27722 = ORIENTED_EDGE ( 'NONE', *, *, #24886, .T. ) ;
#27723 = CYLINDRICAL_SURFACE ( 'NONE', #7853, 6.000000000000000888 ) ;
#27724 = CYLINDRICAL_SURFACE ( 'NONE', #3226, 2.000000000000012879 ) ;
#27725 = AXIS2_PLACEMENT_3D ( 'NONE', #4066, #77, #9462 ) ;
#27726 = CARTESIAN_POINT ( 'NONE',  ( -3.175426480542816510, 5.499999999999865885, -164.8750000000000568 ) ) ;
#27727 = CARTESIAN_POINT ( 'NONE',  ( 3.679869817085056116, -10.37177793260014091, -29.75506555745400306 ) ) ;
#27728 = ORIENTED_EDGE ( 'NONE', *, *, #9598, .T. ) ;
#27729 = CARTESIAN_POINT ( 'NONE',  ( 136.0000000000000284, 1.347111479062088799E-15, 11.00000000000000355 ) ) ;
#27730 =( LENGTH_UNIT ( ) NAMED_UNIT ( * ) SI_UNIT ( .MILLI., .METRE. ) );
#27731 = CARTESIAN_POINT ( 'NONE',  ( -4.763139720814407951, 2.749999999999946709, -169.2500000000000000 ) ) ;
#27732 = CARTESIAN_POINT ( 'NONE',  ( 6.000000000000000000, 2.951592740943527306E-14, -158.1636751345948539 ) ) ;
#27733 = CARTESIAN_POINT ( 'NONE',  ( -2.775557561562891351E-14, -5.500000000000115463, -161.2500000000000000 ) ) ;
#27734 = CARTESIAN_POINT ( 'NONE',  ( 116.3749999999998579, -1.767766952966209892, 1.767766952966542959 ) ) ;
#27735 = CARTESIAN_POINT ( 'NONE',  ( -6.350852961085760029, -1.281975124255709124E-13, -104.6250000000000142 ) ) ;
#27736 = FACE_OUTER_BOUND ( 'NONE', #10317, .T. ) ;
#27737 = CARTESIAN_POINT ( 'NONE',  ( -5.999999999999963585, -1.487416814333745711E-14, -166.4136751345948539 ) ) ;
#27738 = CARTESIAN_POINT ( 'NONE',  ( -2.775557561562891351E-14, -5.500000000000115463, -93.75000000000000000 ) ) ;
#27739 = CARTESIAN_POINT ( 'NONE',  ( -0.05026229418827968254, -14.53482904599736791, 8.281231568825615952 ) ) ;
#27740 = EDGE_LOOP ( 'NONE', ( #21037, #9507, #27595, #12468 ) ) ;
#27741 = AXIS2_PLACEMENT_3D ( 'NONE', #16900, #13053, #12592 ) ;
#27742 = CARTESIAN_POINT ( 'NONE',  ( 118.1874999999997158, 1.035533905932719101, 2.500000000000205169 ) ) ;
#27743 = CARTESIAN_POINT ( 'NONE',  ( 5.196152422706629359, -2.999999999999988898, -161.2886751345948255 ) ) ;
#27744 = CARTESIAN_POINT ( 'NONE',  ( 107.3752832217621886, 1.849990392679523588, 0.000000000000000000 ) ) ;
#27745 = CARTESIAN_POINT ( 'NONE',  ( 139.5000000000000284, -8.500000000000007105, -7.500000000000007105 ) ) ;
#27746 = EDGE_CURVE ( 'NONE', #25123, #13073, #2363, .T. ) ;
#27747 = ORIENTED_EDGE ( 'NONE', *, *, #603, .F. ) ;
#27748 = CYLINDRICAL_SURFACE ( 'NONE', #13843, 5.500000000000000000 ) ;
#27749 = VECTOR ( 'NONE', #29530, 1000.000000000000000 ) ;
#27750 = CARTESIAN_POINT ( 'NONE',  ( -7.216878364870328078, 0.000000000000000000, -90.69198729810784698 ) ) ;
#27751 = EDGE_LOOP ( 'NONE', ( #19574, #13097, #29689, #13367, #13765, #9189, #28025, #9521, #13998, #17115, #3805, #4975, #13459, #6428 ) ) ;
#27752 = DIRECTION ( 'NONE',  ( -1.000000000000000000, -0.000000000000000000, -0.000000000000000000 ) ) ;
#27753 = ORIENTED_EDGE ( 'NONE', *, *, #2463, .F. ) ;
#27754 = CARTESIAN_POINT ( 'NONE',  ( 150.4687500000000284, -2.485281374238585972, 6.000000000000005329 ) ) ;
#27755 = CARTESIAN_POINT ( 'NONE',  ( 6.350852961086080661, -9.614813431917819062E-14, -123.3749999999999858 ) ) ;
#27756 = CARTESIAN_POINT ( 'NONE',  ( 21.75000000000010303, -1.873492889144789952, 1.873492889144845464 ) ) ;
#27757 =( BOUNDED_CURVE ( )  B_SPLINE_CURVE ( 2, ( #5898, #3753, #6067, #29565, #15478, #25098, #17465, #3594, #4054, #13328, #15156 ),
 .UNSPECIFIED., .F., .T. ) 
 B_SPLINE_CURVE_WITH_KNOTS ( ( 3, 2, 2, 2, 2, 3 ),
 ( 0.9344201253893971160, 0.9411764705882352811, 0.9485294117647058432, 0.9558823529411765163, 0.9632352941176470784, 0.9705882352941176405 ),
 .UNSPECIFIED. ) 
 CURVE ( )  GEOMETRIC_REPRESENTATION_ITEM ( )  RATIONAL_B_SPLINE_CURVE ( ( 0.9886498549717824824, 0.9300557229131066750, 1.000000000000000000, 0.9238795325112867385, 1.000000000000000000, 0.9238795325112867385, 1.000000000000000000, 0.9238795325112867385, 1.000000000000000000, 0.9238795325112867385, 1.000000000000000000 ) ) 
 REPRESENTATION_ITEM ( '' )  );
#27758 = CARTESIAN_POINT ( 'NONE',  ( -5.412658773652684552, -3.125000000000099920, -127.4330127018922241 ) ) ;
#27759 = CARTESIAN_POINT ( 'NONE',  ( 10.62500000000013500, -1.414213562372979016, -1.414213562373090038 ) ) ;
#27760 = ORIENTED_EDGE ( 'NONE', *, *, #16516, .T. ) ;
#27761 = DIRECTION ( 'NONE',  ( 1.000000000000000000, -5.551115123125773458E-17, -1.260129944081490338E-35 ) ) ;
#27762 = CARTESIAN_POINT ( 'NONE',  ( 7.216878364870455975, -6.409875621278545621E-14, -166.4419872981078186 ) ) ;
#27763 = CARTESIAN_POINT ( 'NONE',  ( 5.412658773652712085, -3.125000000000086153, -178.5669872981078186 ) ) ;
#27764 = FILL_AREA_STYLE ('',( #15860 ) ) ;
#27765 = FILL_AREA_STYLE ('',( #12113 ) ) ;
#27766 = VERTEX_POINT ( 'NONE', #1066 ) ;
#27767 = CARTESIAN_POINT ( 'NONE',  ( 13.37500000000019185, -1.414213562372979016, 1.414213562372979016 ) ) ;
#27768 = CARTESIAN_POINT ( 'NONE',  ( 0.7617735382584472914, -15.57904714829914461, -7.971427046324570220 ) ) ;
#27769 = CARTESIAN_POINT ( 'NONE',  ( -5.196152422706601826, 2.999999999999975131, -54.03867513459481842 ) ) ;
#27770 = CARTESIAN_POINT ( 'NONE',  ( 2.308094007029174666, 5.188356418777920531, -180.0000000000000000 ) ) ;
#27771 = CARTESIAN_POINT ( 'NONE',  ( 5.196152422706629359, 3.000000000000002665, -137.0386751345948255 ) ) ;
#27772 = CARTESIAN_POINT ( 'NONE',  ( -10.00000000000001421, 1.779758311459933302E-15, -43.99152654425658682 ) ) ;
#27773 = CARTESIAN_POINT ( 'NONE',  ( 3.608439182435180470, -6.249999999999997335, -73.69198729810783277 ) ) ;
#27774 = CARTESIAN_POINT ( 'NONE',  ( 7.216878364870455975, -6.409875621278545621E-14, -62.94198729810783277 ) ) ;
#27775 = ADVANCED_FACE ( 'NONE', ( #17379 ), #23607, .T. ) ;
#27776 = CARTESIAN_POINT ( 'NONE',  ( -4.763139720814407951, -2.750000000000016431, -47.49999999999998579 ) ) ;
#27777 = CARTESIAN_POINT ( 'NONE',  ( -0.05236263670368471873, -9.947637363296282231, -4.619711369386857669 ) ) ;
#27778 = CARTESIAN_POINT ( 'NONE',  ( 6.000000000000052403, -1.607695154586662678, -153.1533121635129646 ) ) ;
#27779 = CARTESIAN_POINT ( 'NONE',  ( 3.464101615137852974, 5.999999999999884537, -159.4136751345947687 ) ) ;
#27780 = CARTESIAN_POINT ( 'NONE',  ( -4.763139720814407951, -2.750000000000016431, -124.0000000000000000 ) ) ;
#27781 = CARTESIAN_POINT ( 'NONE',  ( 6.000000000000000888, -1.859271017917181981E-14, -166.5863248654052029 ) ) ;
#27782 = ORIENTED_EDGE ( 'NONE', *, *, #27114, .F. ) ;
#27783 = CARTESIAN_POINT ( 'NONE',  ( 21.43750000000001066, 1.097466725451619718, -2.649519052838358757 ) ) ;
#27784 = CARTESIAN_POINT ( 'NONE',  ( -5.196152422706601826, 2.999999999999975131, -105.0386751345948539 ) ) ;
#27785 = EDGE_CURVE ( 'NONE', #24822, #22378, #1156, .T. ) ;
#27786 = VERTEX_POINT ( 'NONE', #17686 ) ;
#27787 = STYLED_ITEM ( 'NONE', ( #4321 ), #6778 ) ;
#27788 = CARTESIAN_POINT ( 'NONE',  ( 110.1247167782376124, -1.849990392679412565, 2.220446049250313081E-13 ) ) ;
#27789 = LINE ( 'NONE', #28250, #7401 ) ;
#27790 = CARTESIAN_POINT ( 'NONE',  ( 112.5622167782374703, 1.849990392679562001, -0.7662911109077087390 ) ) ;
#27791 = CARTESIAN_POINT ( 'NONE',  ( 7.216878364870455975, -6.409875621278545621E-14, -107.9419872981078043 ) ) ;
#27792 = CARTESIAN_POINT ( 'NONE',  ( 19.91367513459488237, -1.767766952966154381, -1.767766952966542959 ) ) ;
#27793 = CARTESIAN_POINT ( 'NONE',  ( 110.2738248654048903, -1.999999999999911626, -0.8284271247459952248 ) ) ;
#27794 = VECTOR ( 'NONE', #3571, 1000.000000000000000 ) ;
#27795 = ORIENTED_EDGE ( 'NONE', *, *, #4385, .T. ) ;
#27796 = EDGE_LOOP ( 'NONE', ( #27842, #1929, #5490, #16514 ) ) ;
#27797 = DIRECTION ( 'NONE',  ( 0.000000000000000000, 0.000000000000000000, -1.000000000000000000 ) ) ;
#27798 = CARTESIAN_POINT ( 'NONE',  ( 135.8437500000000284, -6.000000000000005329, -2.485281374238555774 ) ) ;
#27799 = CARTESIAN_POINT ( 'NONE',  ( 5.412658773652739619, 3.124999999999988898, -140.8169872981078186 ) ) ;
#27800 = CIRCLE ( 'NONE', #25851, 5.500000000000000000 ) ;
#27801 = CARTESIAN_POINT ( 'NONE',  ( 14.72617513459484506, -2.499999999999904521, 1.035533905932749299 ) ) ;
#27802 = VECTOR ( 'NONE', #14256, 1000.000000000000000 ) ;
#27803 = CARTESIAN_POINT ( 'NONE',  ( 22.62500000000017408, -1.414213562372867994, -1.414213562373034527 ) ) ;
#27804 = CARTESIAN_POINT ( 'NONE',  ( 0.000000000000000000, 2.081899558550501068E-15, 16.50000000000000355 ) ) ;
#27805 = AXIS2_PLACEMENT_3D ( 'NONE', #3526, #29026, #26714 ) ;
#27806 = CARTESIAN_POINT ( 'NONE',  ( 2.775557561562891351E-14, -6.250000000000061284, -70.18301270189225249 ) ) ;
#27807 = CARTESIAN_POINT ( 'NONE',  ( 145.5788997308104342, -4.999999999999989342, 2.071067811865468400 ) ) ;
#27808 = CARTESIAN_POINT ( 'NONE',  ( 112.2261751345945555, 2.000000000000122125, -0.8284271247460553989 ) ) ;
#27809 = CARTESIAN_POINT ( 'NONE',  ( 3.464101615137757051, -5.999999999999979572, -69.91367513459481131 ) ) ;
#27810 = EDGE_CURVE ( 'NONE', #22119, #26506, #29153, .T. ) ;
#27811 = CARTESIAN_POINT ( 'NONE',  ( 5.999999999999993783, 1.607695154586726627, -165.5966878364870354 ) ) ;
#27812 = EDGE_CURVE ( 'NONE', #7342, #15812, #7455, .T. ) ;
#27813 = CARTESIAN_POINT ( 'NONE',  ( 24.66481880024108619, -2.300353558045364455, 0.4292561541254182877 ) ) ;
#27814 = CARTESIAN_POINT ( 'NONE',  ( 16.85117513459481842, -2.499999999999904521, -1.035533905932749299 ) ) ;
#27815 = CARTESIAN_POINT ( 'NONE',  ( 108.5624999999997442, -2.499999999999934719, -1.035533905932568999 ) ) ;
#27816 =( BOUNDED_CURVE ( )  B_SPLINE_CURVE ( 2, ( #16573, #7008, #2263, #21011, #25429, #26048, #28340, #11668, #30357 ),
 .UNSPECIFIED., .F., .F. ) 
 B_SPLINE_CURVE_WITH_KNOTS ( ( 3, 2, 2, 2, 3 ),
 ( 0.6527777777777777901, 0.6537037037037036757, 0.6555555555555555580, 0.6574074074074074403, 0.6583333333333333259 ),
 .UNSPECIFIED. ) 
 CURVE ( )  GEOMETRIC_REPRESENTATION_ITEM ( )  RATIONAL_B_SPLINE_CURVE ( ( 0.9330127018922194093, 0.9330127018922194093, 1.000000000000000000, 0.8660254037844388186, 1.000000000000000000, 0.8660254037844388186, 1.000000000000000000, 0.9330127018922194093, 0.9330127018922194093 ) ) 
 REPRESENTATION_ITEM ( '' )  );
#27817 = CARTESIAN_POINT ( 'NONE',  ( 0.000000000000000000, 5.499999999999991118, -123.0000000000000000 ) ) ;
#27819 = SURFACE_STYLE_USAGE ( .BOTH. , #17463 ) ;
#27818 = AXIS2_PLACEMENT_3D ( 'NONE', #15925, #11462, #6338 ) ;
#27820 = CARTESIAN_POINT ( 'NONE',  ( 7.216878364870455975, -6.409875621278545621E-14, -146.3080127018922667 ) ) ;
#27821 = DIRECTION ( 'NONE',  ( 1.000000000000000000, 0.000000000000000000, 0.000000000000000000 ) ) ;
#27822 = ORIENTED_EDGE ( 'NONE', *, *, #26900, .T. ) ;
#27823 = CARTESIAN_POINT ( 'NONE',  ( 4.763139720814407951, -2.749999999999988454, -53.00000000000004974 ) ) ;
#27824 = EDGE_CURVE ( 'NONE', #3063, #6123, #5461, .T. ) ;
#27825 = CARTESIAN_POINT ( 'NONE',  ( -5.999999999999919176, 1.607695154586804565, -171.9033121635130215 ) ) ;
#27826 = EDGE_CURVE ( 'NONE', #14122, #17549, #1678, .T. ) ;
#27827 = CARTESIAN_POINT ( 'NONE',  ( 0.000000000000000000, -5.999999999999991118, -163.9613248654052597 ) ) ;
#27828 = ORIENTED_EDGE ( 'NONE', *, *, #24562, .T. ) ;
#27829 = CARTESIAN_POINT ( 'NONE',  ( 105.8124999999999574, 1.035533905932839449, -2.499999999999724221 ) ) ;
#27830 = CARTESIAN_POINT ( 'NONE',  ( 138.0937500000000568, 6.000000000000005329, 2.485281374238585972 ) ) ;
#27831 = LINE ( 'NONE', #4339, #2793 ) ;
#27832 = STYLED_ITEM ( 'NONE', ( #7997 ), #5167 ) ;
#27833 = CARTESIAN_POINT ( 'NONE',  ( 136.5000000000000284, 6.000000000000005329, 0.000000000000000000 ) ) ;
#27834 = CARTESIAN_POINT ( 'NONE',  ( 14.08632486540523132, -1.767766952966320915, 1.767766952966431937 ) ) ;
#27835 = ORIENTED_EDGE ( 'NONE', *, *, #14910, .T. ) ;
#27836 = CARTESIAN_POINT ( 'NONE',  ( -3.175426480542816510, -5.500000000000057732, -135.8750000000000284 ) ) ;
#27837 = AXIS2_PLACEMENT_3D ( 'NONE', #2282, #17178, #5606 ) ;
#27838 = CARTESIAN_POINT ( 'NONE',  ( 13.25000000000017764, 5.551115123125782702E-14, 1.999999999999890754 ) ) ;
#27839 = ORIENTED_EDGE ( 'NONE', *, *, #13022, .T. ) ;
#27840 = CARTESIAN_POINT ( 'NONE',  ( -2.775557561562891351E-14, -5.500000000000115463, -68.25000000000002842 ) ) ;
#27841 = CARTESIAN_POINT ( 'NONE',  ( 18.28867513459494987, 2.500000000000113243, -5.551115123125782702E-14 ) ) ;
#27842 = ORIENTED_EDGE ( 'NONE', *, *, #5312, .F. ) ;
#27843 = CARTESIAN_POINT ( 'NONE',  ( 119.9999999999999574, -0.4876318259219858398, 1.939643060552387110 ) ) ;
#27844 = EDGE_CURVE ( 'NONE', #4876, #4112, #4282, .T. ) ;
#27845 = DIRECTION ( 'NONE',  ( 1.000000000000000000, -0.000000000000000000, -0.000000000000000000 ) ) ;
#27846 = CARTESIAN_POINT ( 'NONE',  ( 140.2643372958527266, -11.26433729585143340, -4.292342582647269644 ) ) ;
#27847 = CARTESIAN_POINT ( 'NONE',  ( 118.3752832217622029, 1.849990392679523588, 0.000000000000000000 ) ) ;
#27848 =( BOUNDED_CURVE ( )  B_SPLINE_CURVE ( 2, ( #1244, #25199, #20166, #17885, #1407, #8315, #4162, #1716, #29515 ),
 .UNSPECIFIED., .F., .T. ) 
 B_SPLINE_CURVE_WITH_KNOTS ( ( 3, 2, 2, 2, 3 ),
 ( 0.1124999999999987121, 0.1187499999999989536, 0.1249999999999991951, 0.1312499999999994227, 0.1374999999999996780 ),
 .UNSPECIFIED. ) 
 CURVE ( )  GEOMETRIC_REPRESENTATION_ITEM ( )  RATIONAL_B_SPLINE_CURVE ( ( 1.000000000000016209, 0.9238795325112705292, 1.000000000000000000, 0.9238795325112867385, 1.000000000000000000, 0.9238795325112867385, 1.000000000000000000, 0.9238795325112900692, 0.9999999999999966693 ) ) 
 REPRESENTATION_ITEM ( '' )  );
#27849 = CARTESIAN_POINT ( 'NONE',  ( -3.175426480542816066, 5.499999999999865885, -146.8750000000000284 ) ) ;
#27850 = DIRECTION ( 'NONE',  ( 1.000000000000000000, -5.551115123125774074E-17, 0.000000000000000000 ) ) ;
#27851 = CARTESIAN_POINT ( 'NONE',  ( 3.175426480543072749, 5.499999999999865885, -139.6250000000000000 ) ) ;
#27852 = CARTESIAN_POINT ( 'NONE',  ( 2.775557561562891351E-14, 6.250000000000033751, -162.4330127018922667 ) ) ;
#27853 = CARTESIAN_POINT ( 'NONE',  ( 0.000000000000000000, 0.000000000000000000, 0.000000000000000000 ) ) ;
#27854 = CARTESIAN_POINT ( 'NONE',  ( 4.763139720814407951, 2.750000000000002665, -81.25000000000004263 ) ) ;
#27855 = ADVANCED_FACE ( 'NONE', ( #27453 ), #8755, .F. ) ;
#27856 = CARTESIAN_POINT ( 'NONE',  ( 4.763139720814407951, 2.750000000000002665, -72.25000000000004263 ) ) ;
#27857 =( BOUNDED_CURVE ( )  B_SPLINE_CURVE ( 2, ( #4760, #16036, #23224, #25333, #4308, #23069, #21065, #6765, #16186 ),
 .UNSPECIFIED., .F., .T. ) 
 B_SPLINE_CURVE_WITH_KNOTS ( ( 3, 2, 2, 2, 3 ),
 ( 0.3374999999999998557, 0.3437500000000000555, 0.3500000000000003109, 0.3562500000000005662, 0.3625000000000007661 ),
 .UNSPECIFIED. ) 
 CURVE ( )  GEOMETRIC_REPRESENTATION_ITEM ( )  RATIONAL_B_SPLINE_CURVE ( ( 1.000000000000001998, 0.9238795325112847401, 1.000000000000000000, 0.9238795325112867385, 1.000000000000000000, 0.9238795325112867385, 1.000000000000000000, 0.9238795325112773016, 1.000000000000009548 ) ) 
 REPRESENTATION_ITEM ( '' )  );
#27858 = ADVANCED_FACE ( 'NONE', ( #16160 ), #23755, .T. ) ;
#27859 = CARTESIAN_POINT ( 'NONE',  ( -6.000000000000007105, -1.607695154586655129, -120.7693375672974412 ) ) ;
#27860 = CARTESIAN_POINT ( 'NONE',  ( 150.3898502691896510, 3.535533905932725318, -3.535533905932725318 ) ) ;
#27861 = DIRECTION ( 'NONE',  ( 0.000000000000000000, 0.000000000000000000, -1.000000000000000000 ) ) ;
#27862 = LINE ( 'NONE', #20987, #2243 ) ;
#27863 = PRESENTATION_LAYER_ASSIGNMENT (  '', '', ( #10736 ) ) ;
#27864 = CARTESIAN_POINT ( 'NONE',  ( 156.0000000000000284, 6.000000000000005329, 0.000000000000000000 ) ) ;
#27865 = CARTESIAN_POINT ( 'NONE',  ( 20.37500000000017053, -1.414213562372979016, 1.414213562373034527 ) ) ;
#27866 = FACE_OUTER_BOUND ( 'NONE', #26028, .T. ) ;
#27867 = CARTESIAN_POINT ( 'NONE',  ( 119.9999999999998721, -0.4876318259425804769, -1.939643060543838615 ) ) ;
#27868 = CARTESIAN_POINT ( 'NONE',  ( 118.1247167782376408, -1.849990392679523588, 0.000000000000000000 ) ) ;
#27869 = CARTESIAN_POINT ( 'NONE',  ( -0.5000000000000004441, -9.500000000000008882, 5.000000000000004441 ) ) ;
#27870 = VERTEX_POINT ( 'NONE', #20735 ) ;
#27871 = CARTESIAN_POINT ( 'NONE',  ( 158.3437500000000568, -6.000000000000005329, -2.485281374238555774 ) ) ;
#27872 = CARTESIAN_POINT ( 'NONE',  ( 3.464101615137757051, -5.999999999999979572, -108.9136751345947971 ) ) ;
#27873 = CARTESIAN_POINT ( 'NONE',  ( 113.5627832217622029, 0.7662911109078888172, 1.849990392679652151 ) ) ;
#27874 = CARTESIAN_POINT ( 'NONE',  ( 3.175426480543072749, -5.500000000000105693, -153.6250000000000568 ) ) ;
#27875 = DIRECTION ( 'NONE',  ( -1.000000000000000000, -0.000000000000000000, -0.000000000000000000 ) ) ;
#27876 = ORIENTED_EDGE ( 'NONE', *, *, #473, .T. ) ;
#27877 = ORIENTED_EDGE ( 'NONE', *, *, #19553, .T. ) ;
#27878 = ORIENTED_EDGE ( 'NONE', *, *, #6608, .F. ) ;
#27879 = CARTESIAN_POINT ( 'NONE',  ( 3.175426480543072749, -5.500000000000105693, -86.12500000000000000 ) ) ;
#27880 = CARTESIAN_POINT ( 'NONE',  ( -5.412658773652739619, 3.124999999999975131, -106.6830127018922383 ) ) ;
#27881 = CARTESIAN_POINT ( 'NONE',  ( 4.767949350811410802, 9.915884935901873476, -28.66271918150854958 ) ) ;
#27882 = CARTESIAN_POINT ( 'NONE',  ( 113.2886751345947118, 1.999999999999946265, 1.110223024625156540E-13 ) ) ;
#27883 = EDGE_CURVE ( 'NONE', #476, #25526, #27979, .T. ) ;
#27884 = CARTESIAN_POINT ( 'NONE',  ( 3.608439182435180470, -6.249999999999997335, -47.55801270189223828 ) ) ;
#27885 = ORIENTED_EDGE ( 'NONE', *, *, #19430, .F. ) ;
#27886 = DIRECTION ( 'NONE',  ( 0.000000000000000000, -1.000000000000000000, 0.000000000000000000 ) ) ;
#27887 = CARTESIAN_POINT ( 'NONE',  ( -3.175426480542816066, -5.500000000000057732, -168.8750000000000568 ) ) ;
#27888 = CARTESIAN_POINT ( 'NONE',  ( -6.000000000000000888, 1.067854986875958443E-15, 7.560779664488942560E-35 ) ) ;
#27889 = CARTESIAN_POINT ( 'NONE',  ( 4.763139720814407951, 2.750000000000002665, -165.2500000000000000 ) ) ;
#27890 = CARTESIAN_POINT ( 'NONE',  ( 110.9999999999999147, 2.500000000000057732, 0.000000000000000000 ) ) ;
#27891 = CARTESIAN_POINT ( 'NONE',  ( -3.175426480542816066, 5.499999999999865885, -104.8750000000000142 ) ) ;
#27892 = CARTESIAN_POINT ( 'NONE',  ( 6.000000000000000888, 7.762456499804234384E-14, -122.1636751345948397 ) ) ;
#27893 = EDGE_CURVE ( 'NONE', #28223, #20037, #6426, .T. ) ;
#27894 = CARTESIAN_POINT ( 'NONE',  ( -4.763139720814407951, 2.749999999999946709, -100.2500000000000000 ) ) ;
#27895 = CARTESIAN_POINT ( 'NONE',  ( 161.7336002691896510, -4.999999999999989342, 2.071067811865468400 ) ) ;
#27896 = ORIENTED_EDGE ( 'NONE', *, *, #12275, .T. ) ;
#27897 = CARTESIAN_POINT ( 'NONE',  ( 13.18750000000012967, -2.649519052838238409, -1.097466725451559322 ) ) ;
#27898 = CARTESIAN_POINT ( 'NONE',  ( 118.3124999999997726, -1.035533905932598975, 2.500000000000205169 ) ) ;
#27899 = CARTESIAN_POINT ( 'NONE',  ( 6.000000000000014211, -1.607695154586730180, -161.2306624327026157 ) ) ;
#27900 = CARTESIAN_POINT ( 'NONE',  ( 105.8752832217621602, -1.849990392679412565, 2.220446049250313081E-13 ) ) ;
#27901 = CARTESIAN_POINT ( 'NONE',  ( 3.464101615137757051, -5.999999999999979572, -85.83632486540520290 ) ) ;
#27902 = ORIENTED_EDGE ( 'NONE', *, *, #19488, .T. ) ;
#27903 = CARTESIAN_POINT ( 'NONE',  ( 107.6247167782376124, 1.849990392679523588, 0.000000000000000000 ) ) ;
#27904 = ORIENTED_EDGE ( 'NONE', *, *, #19615, .F. ) ;
#27905 = CARTESIAN_POINT ( 'NONE',  ( 106.8363248654050750, 1.414213562373256572, 1.414213562373256572 ) ) ;
#27906 = CARTESIAN_POINT ( 'NONE',  ( 147.9375000000000284, -4.242640687119298093, -4.242640687119298093 ) ) ;
#27907 = CARTESIAN_POINT ( 'NONE',  ( 3.175426480543072749, -5.500000000000105693, -111.6249999999999858 ) ) ;
#27908 = AXIS2_PLACEMENT_3D ( 'NONE', #3461, #24967, #1161 ) ;
#27909 = CARTESIAN_POINT ( 'NONE',  ( 23.12500000000011724, 1.665334536937734811E-13, -2.649519052838333888 ) ) ;
#27910 = CARTESIAN_POINT ( 'NONE',  ( -3.608439182435052128, -6.250000000000110134, -133.3080127018922667 ) ) ;
#27911 = ORIENTED_EDGE ( 'NONE', *, *, #16946, .T. ) ;
#27912 = FACE_OUTER_BOUND ( 'NONE', #18166, .T. ) ;
#27913 = CIRCLE ( 'NONE', #14709, 5.500000000000000000 ) ;
#27914 = CARTESIAN_POINT ( 'NONE',  ( -3.608439182435052128, -6.250000000000110134, -169.9419872981078470 ) ) ;
#27915 = CARTESIAN_POINT ( 'NONE',  ( -3.608439182435115633, 6.249999999999965361, -174.9419872981078470 ) ) ;
#27916 = FACE_OUTER_BOUND ( 'NONE', #15955, .T. ) ;
#27917 = ADVANCED_FACE ( 'NONE', ( #11391 ), #15861, .F. ) ;
#27918 = CARTESIAN_POINT ( 'NONE',  ( 10.68750000000004263, -0.8284271247460552878, -1.999999999999971800 ) ) ;
#27919 = CARTESIAN_POINT ( 'NONE',  ( -5.999999999999957367, 1.607695154586737507, -163.4806624327025588 ) ) ;
#27920 = EDGE_CURVE ( 'NONE', #21920, #1067, #8386, .T. ) ;
#27921 = CARTESIAN_POINT ( 'NONE',  ( -6.000000000000000888, 1.067854986875958443E-15, 7.560779664488942560E-35 ) ) ;
#27922 = CARTESIAN_POINT ( 'NONE',  ( -5.196152422706601826, 2.999999999999975131, -132.9613248654052313 ) ) ;
#27923 = PLANE ( 'NONE',  #158 ) ;
#27924 = CARTESIAN_POINT ( 'NONE',  ( 109.1252832217621744, -1.665334536937734811E-13, -1.849990392679523588 ) ) ;
#27925 = CARTESIAN_POINT ( 'NONE',  ( -5.412658773652739619, 3.124999999999975131, -75.81698729810781856 ) ) ;
#27926 = CARTESIAN_POINT ( 'NONE',  ( -5.412658773652684552, -3.125000000000099920, -59.06698729810783277 ) ) ;
#27927 = CARTESIAN_POINT ( 'NONE',  ( 2.775557561562891351E-14, -6.250000000000061284, -181.1830127018922383 ) ) ;
#27928 = CARTESIAN_POINT ( 'NONE',  ( 161.0000000000000284, 0.000000000000000000, -5.500000000000000000 ) ) ;
#27929 = DIRECTION ( 'NONE',  ( 1.000000000000000000, -5.551115123125773458E-17, -1.260129944081490338E-35 ) ) ;
#27930 = CARTESIAN_POINT ( 'NONE',  ( 5.196152422706629359, -2.999999999999988898, -53.28867513459483973 ) ) ;
#27931 = CARTESIAN_POINT ( 'NONE',  ( -3.175426480542816510, -5.500000000000057732, -117.8750000000000142 ) ) ;
#27932 = ORIENTED_EDGE ( 'NONE', *, *, #18299, .F. ) ;
#27933 = CARTESIAN_POINT ( 'NONE',  ( 20.62500000000011369, 2.649519052838500421, -5.551115123125782702E-14 ) ) ;
#27934 = CIRCLE ( 'NONE', #13766, 10.49999999999998224 ) ;
#27935 = DIRECTION ( 'NONE',  ( 0.000000000000000000, 0.000000000000000000, -1.000000000000000000 ) ) ;
#27936 = CIRCLE ( 'NONE', #5852, 10.49999999999999645 ) ;
#27937 = ORIENTED_EDGE ( 'NONE', *, *, #30127, .F. ) ;
#27938 = CARTESIAN_POINT ( 'NONE',  ( 108.4372167782374419, 0.7662911109078588412, -1.849990392679231599 ) ) ;
#27939 = PRESENTATION_LAYER_ASSIGNMENT (  '', '', ( #26946 ) ) ;
#27940 = LINE ( 'NONE', #20914, #15270 ) ;
#27941 = CARTESIAN_POINT ( 'NONE',  ( -3.608439182435052128, -6.250000000000110134, -108.4419872981078043 ) ) ;
#27942 = PLANE ( 'NONE',  #8196 ) ;
#27943 =( BOUNDED_CURVE ( )  B_SPLINE_CURVE ( 2, ( #1663, #22111, #1191, #19951, #24854, #24545, #11057, #17981, #12924 ),
 .UNSPECIFIED., .F., .T. ) 
 B_SPLINE_CURVE_WITH_KNOTS ( ( 3, 2, 2, 2, 3 ),
 ( 0.6138888888888889284, 0.6148148148148148140, 0.6166666666666666963, 0.6185185185185184675, 0.6194444444444444642 ),
 .UNSPECIFIED. ) 
 CURVE ( )  GEOMETRIC_REPRESENTATION_ITEM ( )  RATIONAL_B_SPLINE_CURVE ( ( 0.9330127018922194093, 0.9330127018922234061, 1.000000000000000000, 0.8660254037844388186, 1.000000000000000000, 0.8660254037844388186, 1.000000000000000000, 0.9330127018922154125, 0.9330127018922194093 ) ) 
 REPRESENTATION_ITEM ( '' )  );
#27944 = CARTESIAN_POINT ( 'NONE',  ( 104.7401757384974417, 1.849990392679521589, 1.011113220803300925E-30 ) ) ;
#27945 = VERTEX_POINT ( 'NONE', #18594 ) ;
#27946 = ORIENTED_EDGE ( 'NONE', *, *, #14847, .F. ) ;
#27947 = CARTESIAN_POINT ( 'NONE',  ( 135.2812500000000284, 2.485281374238585972, 6.000000000000005329 ) ) ;
#27948 = CARTESIAN_POINT ( 'NONE',  ( -3.608439182435115633, 6.249999999999965361, -135.9419872981077901 ) ) ;
#27949 = CARTESIAN_POINT ( 'NONE',  ( 10.62500000000010658, 1.665334536937734811E-13, 2.649519052838333888 ) ) ;
#27950 = CARTESIAN_POINT ( 'NONE',  ( 6.000000000000000888, -1.607695154586752384, -93.15331216351302146 ) ) ;
#27951 = VECTOR ( 'NONE', #10001, 1000.000000000000000 ) ;
#27952 = CARTESIAN_POINT ( 'NONE',  ( 22.75000000000015987, 1.110223024625156540E-13, -2.000000000000168310 ) ) ;
#27953 = CARTESIAN_POINT ( 'NONE',  ( 117.6011751345946266, -0.8284271247461453269, 2.000000000000212275 ) ) ;
#27954 = CARTESIAN_POINT ( 'NONE',  ( 117.3988248654050892, -0.8284271247460250898, -1.999999999999851674 ) ) ;
#27955 = CARTESIAN_POINT ( 'NONE',  ( 5.412658773652712085, -3.125000000000086153, -60.93301270189221697 ) ) ;
#27956 = ADVANCED_FACE ( 'NONE', ( #27916 ), #6893, .T. ) ;
#27957 = CARTESIAN_POINT ( 'NONE',  ( 142.8601497308104058, -3.535533905932725318, -3.535533905932725318 ) ) ;
#27958 = DIRECTION ( 'NONE',  ( -1.000000000000000000, -0.000000000000000000, -0.000000000000000000 ) ) ;
#27959 = DIRECTION ( 'NONE',  ( 1.000000000000000000, -5.551115123125773458E-17, -1.260129944081490338E-35 ) ) ;
#27960 = CARTESIAN_POINT ( 'NONE',  ( 0.000000000000000000, 5.999999999999977796, -165.2886751345948824 ) ) ;
#27961 = DIRECTION ( 'NONE',  ( 1.000000000000000000, 1.067522139062651904E-16, -0.000000000000000000 ) ) ;
#27962 = CARTESIAN_POINT ( 'NONE',  ( 0.000000000000000000, 0.000000000000000000, 0.000000000000000000 ) ) ;
#27963 = CARTESIAN_POINT ( 'NONE',  ( 111.9999999999999716, 2.500000000000002220, 0.000000000000000000 ) ) ;
#27964 = CARTESIAN_POINT ( 'NONE',  ( 5.196152422706629359, -2.999999999999988898, -94.71132486540523132 ) ) ;
#27965 = CARTESIAN_POINT ( 'NONE',  ( 0.000000000000000000, 5.499999999999991118, -127.5000000000000568 ) ) ;
#27966 = CARTESIAN_POINT ( 'NONE',  ( 115.0386751345947403, 1.110223024625156540E-13, -1.999999999999668709 ) ) ;
#27967 = CARTESIAN_POINT ( 'NONE',  ( 2.775557561562891351E-14, 6.250000000000033751, -145.9330127018922383 ) ) ;
#27968 = SURFACE_STYLE_USAGE ( .BOTH. , #13911 ) ;
#27969 = CARTESIAN_POINT ( 'NONE',  ( 3.464101615137852974, 5.999999999999884537, -142.9136751345948255 ) ) ;
#27970 = ORIENTED_EDGE ( 'NONE', *, *, #21101, .F. ) ;
#27971 = CARTESIAN_POINT ( 'NONE',  ( 6.350852961086080661, -9.614813431917819062E-14, -51.37500000000002132 ) ) ;
#27972 = CARTESIAN_POINT ( 'NONE',  ( 0.000000000000000000, 0.000000000000000000, 0.000000000000000000 ) ) ;
#27973 = CARTESIAN_POINT ( 'NONE',  ( 116.0000000000000142, 0.000000000000000000, -5.500000000000000000 ) ) ;
#27974 = CARTESIAN_POINT ( 'NONE',  ( 3.464101615137757051, -5.999999999999979572, -178.8363248654052029 ) ) ;
#27975 = ORIENTED_EDGE ( 'NONE', *, *, #17846, .T. ) ;
#27976 = CARTESIAN_POINT ( 'NONE',  ( 105.4374999999998153, -2.499999999999994671, 1.035533905932929599 ) ) ;
#27977 = CARTESIAN_POINT ( 'NONE',  ( 140.5312500000000284, -2.485281374238556218, -6.000000000000005329 ) ) ;
#27978 = CARTESIAN_POINT ( 'NONE',  ( 2.775557561562891351E-14, -6.250000000000061284, -100.8169872981078470 ) ) ;
#27979 = CIRCLE ( 'NONE', #5409, 1.000000000000000888 ) ;
#27980 = DIRECTION ( 'NONE',  ( 0.000000000000000000, 0.000000000000000000, -1.000000000000000000 ) ) ;
#27981 = CARTESIAN_POINT ( 'NONE',  ( 133.8750000000000284, 0.000000000000000000, 6.000000000000005329 ) ) ;
#27982 = DIRECTION ( 'NONE',  ( -1.000000000000000000, 0.000000000000000000, 0.000000000000000000 ) ) ;
#27983 = VERTEX_POINT ( 'NONE', #10529 ) ;
#27984 = EDGE_CURVE ( 'NONE', #8808, #30157, #26769, .T. ) ;
#27985 = CARTESIAN_POINT ( 'NONE',  ( 3.175426480543072749, 5.499999999999865885, -141.1250000000000000 ) ) ;
#27986 = VECTOR ( 'NONE', #26009, 1000.000000000000000 ) ;
#27987 = VERTEX_POINT ( 'NONE', #19593 ) ;
#27988 = ORIENTED_EDGE ( 'NONE', *, *, #5104, .T. ) ;
#27989 = CARTESIAN_POINT ( 'NONE',  ( -2.775557561562891351E-14, -5.500000000000115463, -65.25000000000002842 ) ) ;
#27990 =( BOUNDED_CURVE ( )  B_SPLINE_CURVE ( 2, ( #1062, #26843, #3505, #24110, #21821, #1980, #6276, #13541, #1513 ),
 .UNSPECIFIED., .F., .F. ) 
 B_SPLINE_CURVE_WITH_KNOTS ( ( 3, 2, 2, 2, 3 ),
 ( 0.1374999999999996780, 0.1437499999999998779, 0.1500000000000001332, 0.1562500000000003886, 0.1625000000000006162 ),
 .UNSPECIFIED. ) 
 CURVE ( )  GEOMETRIC_REPRESENTATION_ITEM ( )  RATIONAL_B_SPLINE_CURVE ( ( 1.000000000000003997, 0.9238795325112826307, 1.000000000000000000, 0.9238795325112867385, 1.000000000000000000, 0.9238795325112867385, 1.000000000000000000, 0.9238795325112793000, 1.000000000000007327 ) ) 
 REPRESENTATION_ITEM ( '' )  );
#27991 = DIRECTION ( 'NONE',  ( 1.000000000000000000, 0.000000000000000000, 0.000000000000000000 ) ) ;
#27992 = CARTESIAN_POINT ( 'NONE',  ( -5.999999999999956479, -1.607695154586745057, -124.3466878364870496 ) ) ;
#27993 = CARTESIAN_POINT ( 'NONE',  ( 2.775557561562891351E-14, 6.250000000000033751, -88.93301270189223828 ) ) ;
#27994 = EDGE_CURVE ( 'NONE', #18584, #4636, #8630, .T. ) ;
#27995 = ORIENTED_EDGE ( 'NONE', *, *, #9746, .F. ) ;
#27996 = CARTESIAN_POINT ( 'NONE',  ( -5.999999999999956479, -1.607695154586745057, -113.8466878364870496 ) ) ;
#27997 = CARTESIAN_POINT ( 'NONE',  ( 140.1944936379390754, -11.19449363793808239, -4.371599137206734653 ) ) ;
#27998 = VECTOR ( 'NONE', #9893, 1000.000000000000000 ) ;
#27999 = CARTESIAN_POINT ( 'NONE',  ( 6.000000000000000888, 1.743066579297358182E-13, -86.16367513459481131 ) ) ;
#28000 = CARTESIAN_POINT ( 'NONE',  ( 118.7502832217622455, -1.308140751793529510, 1.308140751793640533 ) ) ;
#28001 = CARTESIAN_POINT ( 'NONE',  ( -4.763139720814407951, -2.750000000000016431, -149.5000000000000284 ) ) ;
#28002 = CARTESIAN_POINT ( 'NONE',  ( 140.4148756743437048, -9.242664784350015594, -7.657040506132355873 ) ) ;
#28003 = CARTESIAN_POINT ( 'NONE',  ( -4.763139720814407951, -2.750000000000016431, -140.5000000000000000 ) ) ;
#28004 = VECTOR ( 'NONE', #9504, 1000.000000000000000 ) ;
#28005 = CARTESIAN_POINT ( 'NONE',  ( 2.775557561562891351E-14, 6.250000000000033751, -159.4330127018922383 ) ) ;
#28006 = CARTESIAN_POINT ( 'NONE',  ( 105.5238248654050750, 0.8284271247462654530, -1.999999999999851674 ) ) ;
#28007 = CARTESIAN_POINT ( 'NONE',  ( -3.175426480542816066, -5.500000000000057732, -77.37500000000001421 ) ) ;
#28008 = CARTESIAN_POINT ( 'NONE',  ( 3.175426480543072749, 5.499999999999865885, -67.62500000000002842 ) ) ;
#28009 = CARTESIAN_POINT ( 'NONE',  ( -5.999999999999956479, -1.607695154586745057, -88.34668783648706381 ) ) ;
#28010 = CARTESIAN_POINT ( 'NONE',  ( 144.6636751345948255, 0.000000000000000000, 5.500000000000005329 ) ) ;
#28011 = STYLED_ITEM ( 'NONE', ( #11643 ), #11474 ) ;
#28012 = CARTESIAN_POINT ( 'NONE',  ( 158.0625000000000284, -4.242640687119298093, 4.242640687119298093 ) ) ;
#28013 =( LENGTH_UNIT ( ) NAMED_UNIT ( * ) SI_UNIT ( .MILLI., .METRE. ) );
#28014 = CARTESIAN_POINT ( 'NONE',  ( 21.12500000000011724, 1.414213562373201061, 1.414213562373034527 ) ) ;
#28015 = CARTESIAN_POINT ( 'NONE',  ( -19.49999999999998224, -54.99999999999990763, 8.000000000000007105 ) ) ;
#28016 = DIRECTION ( 'NONE',  ( -7.147005652999508048E-36, 5.642372883946980038E-36, 1.000000000000000000 ) ) ;
#28017 = CARTESIAN_POINT ( 'NONE',  ( 116.8747167782375556, 0.000000000000000000, 1.849990392679523588 ) ) ;
#28018 = CARTESIAN_POINT ( 'NONE',  ( -5.999999999999963585, 1.780251999655701777E-13, -98.33632486540520290 ) ) ;
#28019 = VERTEX_POINT ( 'NONE', #537 ) ;
#28020 = CARTESIAN_POINT ( 'NONE',  ( 148.7812500000000284, 2.485281374238585972, 6.000000000000005329 ) ) ;
#28021 = FILL_AREA_STYLE_COLOUR ( '', #25339 ) ;
#28022 = CARTESIAN_POINT ( 'NONE',  ( 114.0002832217621602, -1.308140751793585022, -1.308140751793640533 ) ) ;
#28023 = EDGE_CURVE ( 'NONE', #16823, #22218, #16297, .T. ) ;
#28024 = CARTESIAN_POINT ( 'NONE',  ( 10.00000000000001421, -5.551115123125781716E-16, -44.99152654425658682 ) ) ;
#28025 = ORIENTED_EDGE ( 'NONE', *, *, #19956, .T. ) ;
#28026 = VERTEX_POINT ( 'NONE', #19301 ) ;
#28027 = ORIENTED_EDGE ( 'NONE', *, *, #25800, .F. ) ;
#28028 = CARTESIAN_POINT ( 'NONE',  ( 3.175426480543072749, -5.500000000000105693, -89.12500000000000000 ) ) ;
#28029 = EDGE_CURVE ( 'NONE', #19511, #25088, #28623, .T. ) ;
#28030 =( BOUNDED_CURVE ( )  B_SPLINE_CURVE ( 2, ( #26944, #10867, #11016, #20223, #8689, #27399, #6364, #24950, #29573 ),
 .UNSPECIFIED., .F., .T. ) 
 B_SPLINE_CURVE_WITH_KNOTS ( ( 3, 2, 2, 2, 3 ),
 ( 0.4416666666666666519, 0.4425925925925925375, 0.4444444444444444198, 0.4462962962962963021, 0.4472222222222221877 ),
 .UNSPECIFIED. ) 
 CURVE ( )  GEOMETRIC_REPRESENTATION_ITEM ( )  RATIONAL_B_SPLINE_CURVE ( ( 0.9330127018922194093, 0.9330127018922194093, 1.000000000000000000, 0.8660254037844388186, 1.000000000000000000, 0.8660254037844388186, 1.000000000000000000, 0.9330127018922234061, 0.9330127018922194093 ) ) 
 REPRESENTATION_ITEM ( '' )  );
#28031 = CARTESIAN_POINT ( 'NONE',  ( 2.775557561562891351E-14, -6.250000000000061284, -110.6830127018922383 ) ) ;
#28032 = ADVANCED_FACE ( 'NONE', ( #10232 ), #3132, .T. ) ;
#28033 = ORIENTED_EDGE ( 'NONE', *, *, #168, .T. ) ;
#28034 = CARTESIAN_POINT ( 'NONE',  ( 5.681812044562478903, 9.420575401947205663, -23.03339967402430943 ) ) ;
#28035 = STYLED_ITEM ( 'NONE', ( #1923 ), #11505 ) ;
#28036 = CARTESIAN_POINT ( 'NONE',  ( 158.1413997308104058, 2.071067811865468400, -4.999999999999989342 ) ) ;
#28037 = CARTESIAN_POINT ( 'NONE',  ( -5.196152422706573404, -3.000000000000002665, -63.71132486540520290 ) ) ;
#28038 = EDGE_LOOP ( 'NONE', ( #14410, #17847, #13810, #10338 ) ) ;
#28039 = CARTESIAN_POINT ( 'NONE',  ( 0.000000000000000000, 0.000000000000000000, 0.000000000000000000 ) ) ;
#28040 = CARTESIAN_POINT ( 'NONE',  ( -4.763139720814407951, -2.750000000000016431, -175.0000000000000568 ) ) ;
#28041 = CARTESIAN_POINT ( 'NONE',  ( 23.10117513459496763, 1.035533905932809473, -2.499999999999904521 ) ) ;
#28042 = MECHANICAL_DESIGN_GEOMETRIC_PRESENTATION_REPRESENTATION (  '', ( #101 ), #14580 ) ;
#28043 = CARTESIAN_POINT ( 'NONE',  ( 3.175426480543072749, 5.499999999999865885, -153.1250000000000284 ) ) ;
#28044 = CARTESIAN_POINT ( 'NONE',  ( 113.1249999999998295, 1.767766952966376426, 1.767766952966320915 ) ) ;
#28045 = VECTOR ( 'NONE', #5070, 1000.000000000000000 ) ;
#28046 = CARTESIAN_POINT ( 'NONE',  ( 21.08632486540515316, -1.767766952966154381, 1.767766952966376426 ) ) ;
#28047 = CARTESIAN_POINT ( 'NONE',  ( -5.999999999999919176, 1.607695154586804565, -86.98066243270262987 ) ) ;
#28048 = CARTESIAN_POINT ( 'NONE',  ( 0.000000000000000000, 5.499999999999991118, -94.50000000000002842 ) ) ;
#28049 = CARTESIAN_POINT ( 'NONE',  ( 134.9999999999997158, -6.982120021894168360, 8.500000000000007105 ) ) ;
#28050 = ORIENTED_EDGE ( 'NONE', *, *, #22793, .T. ) ;
#28051 = CARTESIAN_POINT ( 'NONE',  ( 11.06249999999994671, -2.649519052838298805, 1.097466725451499370 ) ) ;
#28052 = CARTESIAN_POINT ( 'NONE',  ( 114.8124999999998010, 1.035533905932749299, -2.499999999999844569 ) ) ;
#28053 = CARTESIAN_POINT ( 'NONE',  ( 15.53867513459491967, 1.110223024625156540E-13, 2.499999999999835687 ) ) ;
#28054 = CARTESIAN_POINT ( 'NONE',  ( 108.0002832217622597, -1.308140751793585022, -1.308140751793640533 ) ) ;
#28055 = CARTESIAN_POINT ( 'NONE',  ( 6.000000000000000888, 1.743066579297358182E-13, -50.16367513459482552 ) ) ;
#28056 = VERTEX_POINT ( 'NONE', #29080 ) ;
#28057 = CARTESIAN_POINT ( 'NONE',  ( 6.000000000000000888, -3.330669073875464691E-16, -7.560779664488942560E-35 ) ) ;
#28058 = FACE_OUTER_BOUND ( 'NONE', #7810, .T. ) ;
#28059 = CARTESIAN_POINT ( 'NONE',  ( 105.4997167782376550, 1.308140751793668288, -1.308140751793640533 ) ) ;
#28060 = EDGE_CURVE ( 'NONE', #9068, #29150, #23187, .T. ) ;
#28061 = PRODUCT_DEFINITION_SHAPE ( 'NONE', 'NONE',  #29032 ) ;
#28062 = EDGE_LOOP ( 'NONE', ( #17000, #7326, #25663, #7916 ) ) ;
#28063 = CARTESIAN_POINT ( 'NONE',  ( -6.000000000000007105, -1.607695154586655129, -53.26933756729743408 ) ) ;
#28064 = CARTESIAN_POINT ( 'NONE',  ( 151.5000000000000284, 6.000000000000005329, 0.000000000000000000 ) ) ;
#28065 = ORIENTED_EDGE ( 'NONE', *, *, #7994, .T. ) ;
#28066 = CARTESIAN_POINT ( 'NONE',  ( 4.763139720814407951, 2.750000000000002665, -111.2500000000000142 ) ) ;
#28067 = CARTESIAN_POINT ( 'NONE',  ( 22.74999999999999289, -1.873492889144900975, 1.873492889144845464 ) ) ;
#28068 = ADVANCED_FACE ( 'NONE', ( #12259 ), #8192, .T. ) ;
#28069 = CARTESIAN_POINT ( 'NONE',  ( 2.775557561562891351E-14, -6.250000000000061284, -133.1830127018922667 ) ) ;
#28070 = ORIENTED_EDGE ( 'NONE', *, *, #11726, .F. ) ;
#28071 = CARTESIAN_POINT ( 'NONE',  ( 158.8988248654052313, 3.889087296526011706, 3.889087296526011706 ) ) ;
#28072 = CARTESIAN_POINT ( 'NONE',  ( -3.608439182435115633, 6.249999999999965361, -167.4419872981078186 ) ) ;
#28073 = CARTESIAN_POINT ( 'NONE',  ( 110.1249999999998437, 1.767766952966265404, 1.767766952966431937 ) ) ;
#28074 = ORIENTED_EDGE ( 'NONE', *, *, #25322, .T. ) ;
#28075 = PRESENTATION_LAYER_ASSIGNMENT (  '', '', ( #637 ) ) ;
#28076 = CARTESIAN_POINT ( 'NONE',  ( 153.3824251345948539, 5.500000000000012434, 2.278174593052012309 ) ) ;
#28077 = DIRECTION ( 'NONE',  ( 1.000000000000000000, -5.551115123125773458E-17, -1.260129944081490338E-35 ) ) ;
#28078 = CARTESIAN_POINT ( 'NONE',  ( 3.175426480543072749, 5.499999999999865885, -180.1250000000000000 ) ) ;
#28079 = CARTESIAN_POINT ( 'NONE',  ( 106.7502832217622597, -1.308140751793529510, 1.308140751793973600 ) ) ;
#28080 = CARTESIAN_POINT ( 'NONE',  ( -3.608439182435052128, -6.250000000000110134, -179.8080127018922383 ) ) ;
#28081 = CARTESIAN_POINT ( 'NONE',  ( 3.464101615137757051, -5.999999999999979572, -111.3363248654051745 ) ) ;
#28082 = CARTESIAN_POINT ( 'NONE',  ( 125.0000000000000568, -55.00000000000000711, 8.000000000000007105 ) ) ;
#28083 = DIRECTION ( 'NONE',  ( 1.000000000000000000, 1.674905425081055330E-15, 0.000000000000000000 ) ) ;
#28084 = CARTESIAN_POINT ( 'NONE',  ( 6.350852961086080661, -9.614813431917819062E-14, -123.3749999999999858 ) ) ;
#28085 = LINE ( 'NONE', #23804, #6812 ) ;
#28086 = CARTESIAN_POINT ( 'NONE',  ( -5.196152422706601826, 2.999999999999975131, -153.9613248654052597 ) ) ;
#28087 = ORIENTED_EDGE ( 'NONE', *, *, #16303, .T. ) ;
#28088 = CARTESIAN_POINT ( 'NONE',  ( 21.00000000000012790, -1.873492889144789952, 1.873492889144845464 ) ) ;
#28089 = CARTESIAN_POINT ( 'NONE',  ( 0.2151077267762193934, -15.80992884008447241, 7.511547624681091051 ) ) ;
#28090 = CARTESIAN_POINT ( 'NONE',  ( 143.4449251345948539, -5.500000000000012434, 2.278174593052012309 ) ) ;
#28091 = DIRECTION ( 'NONE',  ( 1.000000000000000000, -5.551115123125773458E-17, -1.260129944081490338E-35 ) ) ;
#28092 = COLOUR_RGB ( '', 0.31764706, 0.68627451, 0.89019608) ;
#28093 = VERTEX_POINT ( 'NONE', #12554 ) ;
#28094 = CARTESIAN_POINT ( 'NONE',  ( 109.9997167782376835, -1.308140751793612777, 1.308140751793640533 ) ) ;
#28095 = CARTESIAN_POINT ( 'NONE',  ( 5.412658773652712085, -3.125000000000086153, -108.0669872981078186 ) ) ;
#28096 = EDGE_CURVE ( 'NONE', #27528, #13966, #6805, .T. ) ;
#28097 = CARTESIAN_POINT ( 'NONE',  ( 21.96132486540530593, 1.665334536937734811E-13, 2.499999999999946709 ) ) ;
#28098 = CARTESIAN_POINT ( 'NONE',  ( 156.6636751345948255, 0.000000000000000000, 5.500000000000005329 ) ) ;
#28099 = EDGE_CURVE ( 'NONE', #26686, #2098, #18372, .T. ) ;
#28100 = CARTESIAN_POINT ( 'NONE',  ( -5.999999999999962697, 3.323446944526963891E-14, -148.4136751345948255 ) ) ;
#28101 = ORIENTED_EDGE ( 'NONE', *, *, #1011, .F. ) ;
#28102 = ORIENTED_EDGE ( 'NONE', *, *, #25346, .F. ) ;
#28103 = CARTESIAN_POINT ( 'NONE',  ( 20.53867513459481486, 0.000000000000000000, 2.500000000000002220 ) ) ;
#28104 = CARTESIAN_POINT ( 'NONE',  ( 136.3125000000000284, 4.242640687119298093, -4.242640687119298093 ) ) ;
#28105 = VERTEX_POINT ( 'NONE', #29853 ) ;
#28106 = CARTESIAN_POINT ( 'NONE',  ( -7.216878364870328078, 0.000000000000000000, -141.6919872981078186 ) ) ;
#28107 = CARTESIAN_POINT ( 'NONE',  ( 161.0000000000000284, 3.467572205841706889, 4.269185284954735593 ) ) ;
#28108 = CARTESIAN_POINT ( 'NONE',  ( 11.62500000000007994, 1.110223024625156540E-13, 2.649519052838167354 ) ) ;
#28109 = CARTESIAN_POINT ( 'NONE',  ( -3.464101615137757051, -5.999999999999979572, -93.58632486540523132 ) ) ;
#28110 = CARTESIAN_POINT ( 'NONE',  ( 18.25000000000009948, 1.110223024625156540E-13, 1.999999999999946265 ) ) ;
#28111 = CARTESIAN_POINT ( 'NONE',  ( -6.000000000000000888, 1.067854986875958443E-15, 7.560779664488942560E-35 ) ) ;
#28112 = B_SPLINE_CURVE_WITH_KNOTS ( 'NONE', 3,
 ( #8064, #11025, #3913, #17481, #3452, #10556, #22376, #5609, #20070, #13342, #15016, #26794, #5759, #29416 ),
 .UNSPECIFIED., .F., .F.,
 ( 4, 2, 2, 2, 2, 2, 4 ),
 ( 0.007875088219727693212, 0.008688851078647757617, 0.009095732508107790687, 0.009502613937567822022, 0.009909495367027855092, 0.01031637679648788816, 0.01113013965540795257 ),
 .UNSPECIFIED. ) ;
#28113 = CARTESIAN_POINT ( 'NONE',  ( 7.216878364870455975, -6.409875621278545621E-14, -59.30801270189222407 ) ) ;
#28114 = DIRECTION ( 'NONE',  ( 1.000000000000000000, -5.551115123125773458E-17, -1.260129944081490338E-35 ) ) ;
#28115 = CIRCLE ( 'NONE', #18836, 2.000000000000000000 ) ;
#28116 = CARTESIAN_POINT ( 'NONE',  ( 144.1726497308104058, -5.000000000000004441, 0.000000000000000000 ) ) ;
#28117 = CARTESIAN_POINT ( 'NONE',  ( 9.433704689814137012, 2.880675993249602881E-15, -16.18577070100374371 ) ) ;
#28118 = CARTESIAN_POINT ( 'NONE',  ( -6.000000000000007105, -1.607695154586655129, -161.2693375672974696 ) ) ;
#28119 = CARTESIAN_POINT ( 'NONE',  ( -5.999999999999982236, -1.607695154586700426, -146.8466878364870070 ) ) ;
#28120 = VECTOR ( 'NONE', #27064, 1000.000000000000000 ) ;
#28121 = CYLINDRICAL_SURFACE ( 'NONE', #3735, 1.000000000000000888 ) ;
#28122 = CARTESIAN_POINT ( 'NONE',  ( 3.464101615137852974, 5.999999999999884537, -113.8363248654051745 ) ) ;
#28123 = CARTESIAN_POINT ( 'NONE',  ( 111.8124999999997584, 1.035533905932779275, -2.499999999999964473 ) ) ;
#28124 =( BOUNDED_CURVE ( )  B_SPLINE_CURVE ( 2, ( #19385, #2921, #23543, #7683, #2482, #17091, #9862, #19236, #29014 ),
 .UNSPECIFIED., .F., .F. ) 
 B_SPLINE_CURVE_WITH_KNOTS ( ( 3, 2, 2, 2, 3 ),
 ( 0.6916666666666666519, 0.6925925925925926485, 0.6944444444444444198, 0.6962962962962963021, 0.6972222222222221877 ),
 .UNSPECIFIED. ) 
 CURVE ( )  GEOMETRIC_REPRESENTATION_ITEM ( )  RATIONAL_B_SPLINE_CURVE ( ( 0.9330127018922194093, 0.9330127018922154125, 1.000000000000000000, 0.8660254037844388186, 1.000000000000000000, 0.8660254037844388186, 1.000000000000000000, 0.9330127018922234061, 0.9330127018922194093 ) ) 
 REPRESENTATION_ITEM ( '' )  );
#28125 = SURFACE_STYLE_FILL_AREA ( #4927 ) ;
#28126 = DIRECTION ( 'NONE',  ( 6.938893903907222067E-15, -1.000000000000000000, 0.000000000000000000 ) ) ;
#28127 = VERTEX_POINT ( 'NONE', #27686 ) ;
#28128 = CARTESIAN_POINT ( 'NONE',  ( 6.350852961086080661, -9.614813431917819062E-14, -54.37500000000003553 ) ) ;
#28129 = FACE_OUTER_BOUND ( 'NONE', #5916, .T. ) ;
#28130 =( BOUNDED_CURVE ( )  B_SPLINE_CURVE ( 2, ( #27552, #3908, #24499, #1619, #8213, #29576, #20366, #10871, #6370 ),
 .UNSPECIFIED., .F., .T. ) 
 B_SPLINE_CURVE_WITH_KNOTS ( ( 3, 2, 2, 2, 3 ),
 ( 0.3625000000000007661, 0.3687500000000005773, 0.3750000000000003331, 0.3812500000000000888, 0.3874999999999999001 ),
 .UNSPECIFIED. ) 
 CURVE ( )  GEOMETRIC_REPRESENTATION_ITEM ( )  RATIONAL_B_SPLINE_CURVE ( ( 0.9999999999999905631, 0.9238795325112961754, 1.000000000000000000, 0.9238795325112867385, 1.000000000000000000, 0.9238795325112867385, 1.000000000000000000, 0.9238795325112880708, 0.9999999999999986677 ) ) 
 REPRESENTATION_ITEM ( '' )  );
#28131 = CARTESIAN_POINT ( 'NONE',  ( -6.000000000000007105, -1.607695154586655129, -179.2693375672974696 ) ) ;
#28132 = ORIENTED_EDGE ( 'NONE', *, *, #28158, .T. ) ;
#28133 = CARTESIAN_POINT ( 'NONE',  ( 106.1249999999999858, 1.767766952966320915, 1.767766952966431937 ) ) ;
#28134 = CARTESIAN_POINT ( 'NONE',  ( 141.8437500000000568, -6.000000000000005329, -2.485281374238556218 ) ) ;
#28135 = CARTESIAN_POINT ( 'NONE',  ( 11.43750000000003197, -1.999999999999911626, 0.8284271247462955401 ) ) ;
#28136 = CARTESIAN_POINT ( 'NONE',  ( 5.412658773652739619, 3.124999999999988898, -104.8169872981078470 ) ) ;
#28137 = DIRECTION ( 'NONE',  ( 1.000000000000000000, -5.551115123125773458E-17, -1.260129944081490338E-35 ) ) ;
#28138 = EDGE_CURVE ( 'NONE', #16010, #15961, #22350, .T. ) ;
#28139 = CARTESIAN_POINT ( 'NONE',  ( 132.5625000000000284, -4.242640687119298093, 4.242640687119298093 ) ) ;
#28140 = ORIENTED_EDGE ( 'NONE', *, *, #565, .T. ) ;
#28141 = CLOSED_SHELL ( 'NONE', ( #1185, #15198, #27507, #3859, #5179, #11474, #3817, #12843, #30120, #6884, #14454, #979, #17033, #27288, #21334, #4571, #25177, #27262, #3790, #27917, #3422, #24848, #23960, #10017, #15922, #27156, #5546, #3263, #12368, #23889, #13558, #3252, #2852, #16057, #26910, #25858, #14331, #6354, #23989, #29379, #7443, #16776, #943, #10296, #328, #22508, #7471, #19286, #9, #19292, #13276, #27197, #21849, #139, #29410, #13311, #19722, #18571, #16674, #7065, #10399, #16810, #29092, #14513, #29627, #5900, #98, #6324, #29496, #5129, #10870, #25921, #23110, #15738, #28636, #18363, #18162, #7957, #13310, #9576, #25993, #2364, #13845, #12132, #10259, #4906, #5167, #7131, #24129, #2220, #7737, #20695, #2508, #22155, #6788, #16651, #6089, #23581, #3883, #9279, #26664, #27775, #9723, #20155, #4379, #27336, #169, #16033, #13451, #24351, #25626, #30341, #15893, #790, #17004, #10628, #28571, #21199, #29191, #10909, #21405, #12964, #11763, #23460, #11827, #6379, #3187, #7634, #26651, #19323, #18543, #9541, #26570, #21086, #19781, #29265, #29201, #17807, #26879, #28887, #20530, #3948, #24911, #22956, #18677, #13286, #23035, #14226, #8474, #9076, #28363, #25892, #24286, #6817, #26361, #19562, #18401, #7572, #11137, #29226, #56, #8743, #29340, #16818, #2179, #18190, #16643, #25504, #11403, #24453, #14617, #8665, #780, #8107, #12436, #20643, #9473, #26691, #5037, #23821, #26163, #26222, #4202, #22999, #12893, #10530, #19821, #25998, #7544, #7074 ) ) ;
#28142 = CARTESIAN_POINT ( 'NONE',  ( -4.763139720814407951, 2.749999999999946709, -136.2499999999999716 ) ) ;
#28143 = ORIENTED_EDGE ( 'NONE', *, *, #16540, .T. ) ;
#28144 = CARTESIAN_POINT ( 'NONE',  ( 3.175426480543072749, -5.500000000000105693, -65.12500000000001421 ) ) ;
#28145 = CARTESIAN_POINT ( 'NONE',  ( -5.999999999999963585, 8.134310703387671600E-14, -115.4136751345948397 ) ) ;
#28146 = CARTESIAN_POINT ( 'NONE',  ( 3.464101615137852974, 5.999999999999884537, -66.41367513459485394 ) ) ;
#28147 = CARTESIAN_POINT ( 'NONE',  ( 2.775557561562891351E-14, -6.250000000000061284, -83.68301270189226670 ) ) ;
#28148 = CARTESIAN_POINT ( 'NONE',  ( -5.999999999999956479, -1.607695154586745057, -101.2693375672974554 ) ) ;
#28149 = CARTESIAN_POINT ( 'NONE',  ( 154.7886751345948255, 5.500000000000005329, 0.000000000000000000 ) ) ;
#28150 = CARTESIAN_POINT ( 'NONE',  ( 105.9372167782374135, -0.7662911109076184779, 1.849990392679652151 ) ) ;
#28151 = DIRECTION ( 'NONE',  ( 0.000000000000000000, -1.000000000000000000, -0.000000000000000000 ) ) ;
#28152 = CARTESIAN_POINT ( 'NONE',  ( 117.3752832217622029, 1.849990392679523588, 0.000000000000000000 ) ) ;
#28153 = CARTESIAN_POINT ( 'NONE',  ( -4.763139720814407951, -2.750000000000016431, -148.0000000000000284 ) ) ;
#28154 = FACE_OUTER_BOUND ( 'NONE', #7768, .T. ) ;
#28155 = CARTESIAN_POINT ( 'NONE',  ( 2.775557561562891351E-14, 6.250000000000033751, -160.9330127018922667 ) ) ;
#28156 = CARTESIAN_POINT ( 'NONE',  ( 5.196152422706629359, -2.999999999999988898, -148.7113248654052313 ) ) ;
#28157 = CARTESIAN_POINT ( 'NONE',  ( 5.999999999999949374, 1.607695154586804565, -49.51933756729743408 ) ) ;
#28158 = EDGE_CURVE ( 'NONE', #19684, #6844, #12341, .T. ) ;
#28159 = CARTESIAN_POINT ( 'NONE',  ( -2.775557561562891351E-14, -5.500000000000115463, -77.25000000000004263 ) ) ;
#28160 = DIRECTION ( 'NONE',  ( 0.000000000000000000, 8.881784197001252323E-16, 1.000000000000000000 ) ) ;
#28161 = CARTESIAN_POINT ( 'NONE',  ( -2.775557561562891351E-14, -5.500000000000115463, -62.25000000000002842 ) ) ;
#28162 = SURFACE_STYLE_USAGE ( .BOTH. , #14105 ) ;
#28163 = CARTESIAN_POINT ( 'NONE',  ( 143.9211002691896510, -4.999999999999989342, -2.071067811865468400 ) ) ;
#28164 = LINE ( 'NONE', #25570, #10293 ) ;
#28165 = CARTESIAN_POINT ( 'NONE',  ( -6.000000000000060396, -1.607695154586566089, -144.7693375672974696 ) ) ;
#28166 = CARTESIAN_POINT ( 'NONE',  ( 158.4375000000000284, -4.242640687119298093, -4.242640687119298093 ) ) ;
#28167 = SURFACE_STYLE_USAGE ( .BOTH. , #4827 ) ;
#28168 = CARTESIAN_POINT ( 'NONE',  ( -5.999999999999962697, 3.323446944526963260E-14, -147.8363248654052313 ) ) ;
#28169 = CARTESIAN_POINT ( 'NONE',  ( 119.6872167782376408, 1.849990392679562001, 0.7662911109079489913 ) ) ;
#28170 = CARTESIAN_POINT ( 'NONE',  ( -5.196152422706573404, -3.000000000000002665, -98.21132486540523132 ) ) ;
#28171 = EDGE_CURVE ( 'NONE', #10146, #28423, #1351, .T. ) ;
#28172 = ORIENTED_EDGE ( 'NONE', *, *, #3158, .T. ) ;
#28173 = CARTESIAN_POINT ( 'NONE',  ( 147.5625000000000284, -4.242640687119298093, 4.242640687119298093 ) ) ;
#28174 = CARTESIAN_POINT ( 'NONE',  ( -4.999999999999990230, -24.99999999999999289, 7.500000000000007105 ) ) ;
#28175 = CARTESIAN_POINT ( 'NONE',  ( 114.3127832217620465, 1.849990392679562001, -0.7662911109076485650 ) ) ;
#28176 = ORIENTED_EDGE ( 'NONE', *, *, #11751, .T. ) ;
#28177 = CARTESIAN_POINT ( 'NONE',  ( 20.62500000000014211, -1.414213562372979016, -1.414213562373145550 ) ) ;
#28178 = ORIENTED_EDGE ( 'NONE', *, *, #9401, .T. ) ;
#28179 = CARTESIAN_POINT ( 'NONE',  ( 4.763139720814407951, 2.750000000000002665, -90.25000000000005684 ) ) ;
#28180 = COLOUR_RGB ( '', 0.72549020, 0.75294118, 0.79215686) ;
#28181 = EDGE_LOOP ( 'NONE', ( #9954, #2433, #14610, #1343 ) ) ;
#28182 = CARTESIAN_POINT ( 'NONE',  ( 140.0000000000000284, -54.99999999999990763, 8.000000000000007105 ) ) ;
#28183 = CARTESIAN_POINT ( 'NONE',  ( 156.1726497308104058, -5.000000000000004441, 0.000000000000000000 ) ) ;
#28184 = CARTESIAN_POINT ( 'NONE',  ( 4.763139720814407951, 2.750000000000002665, -165.2500000000000000 ) ) ;
#28185 = DIRECTION ( 'NONE',  ( -1.000000000000000000, -1.665334536937736783E-16, -2.220446049250315546E-16 ) ) ;
#28186 =( NAMED_UNIT ( * ) PLANE_ANGLE_UNIT ( ) SI_UNIT ( $, .RADIAN. ) );
#28187 = CARTESIAN_POINT ( 'NONE',  ( -4.763139720814407951, 2.749999999999946709, -172.2500000000000000 ) ) ;
#28188 = CARTESIAN_POINT ( 'NONE',  ( 147.0863248654052313, 0.000000000000000000, 5.500000000000005329 ) ) ;
#28189 = CARTESIAN_POINT ( 'NONE',  ( -3.175426480542816510, 5.499999999999865885, -152.8749999999999716 ) ) ;
#28190 = CARTESIAN_POINT ( 'NONE',  ( 110.6249999999998437, -1.767766952966376426, -1.767766952966320915 ) ) ;
#28191 = AXIS2_PLACEMENT_3D ( 'NONE', #4529, #8997, #2239 ) ;
#28192 = EDGE_CURVE ( 'NONE', #13355, #18612, #12355, .T. ) ;
#28193 = CARTESIAN_POINT ( 'NONE',  ( -4.763139720814407951, -2.750000000000016431, -100.0000000000000284 ) ) ;
#28194 = CARTESIAN_POINT ( 'NONE',  ( 116.0000000000000142, 0.000000000000000000, 0.000000000000000000 ) ) ;
#28195 = CARTESIAN_POINT ( 'NONE',  ( 115.6636751345946550, -1.414213562373090038, 1.414213562373145550 ) ) ;
#28197 = CARTESIAN_POINT ( 'NONE',  ( -4.763139720814407951, 2.749999999999946709, -86.75000000000000000 ) ) ;
#28196 = CARTESIAN_POINT ( 'NONE',  ( 0.000000000000000000, 5.499999999999991118, -154.5000000000000284 ) ) ;
#28198 = CARTESIAN_POINT ( 'NONE',  ( 161.2648502691896510, 3.535533905932725318, 3.535533905932752852 ) ) ;
#28199 = CARTESIAN_POINT ( 'NONE',  ( 0.2111556581636949148, -15.49108841857535168, 8.141471415412047108 ) ) ;
#28200 = ORIENTED_EDGE ( 'NONE', *, *, #1608, .T. ) ;
#28201 = CARTESIAN_POINT ( 'NONE',  ( 23.68750000000013500, -0.8284271247461152399, -1.999999999999911626 ) ) ;
#28202 = CARTESIAN_POINT ( 'NONE',  ( 113.1249999999998295, 1.767766952966376426, 1.767766952966320915 ) ) ;
#28203 = DIRECTION ( 'NONE',  ( 1.000000000000000000, 0.000000000000000000, 0.000000000000000000 ) ) ;
#28204 = CARTESIAN_POINT ( 'NONE',  ( 105.3127832217621034, 1.849990392679562001, -0.7662911109076485650 ) ) ;
#28205 = EDGE_CURVE ( 'NONE', #9697, #3256, #27385, .T. ) ;
#28206 = CARTESIAN_POINT ( 'NONE',  ( -3.464101615137757051, -5.999999999999979572, -86.08632486540520290 ) ) ;
#28207 = ORIENTED_EDGE ( 'NONE', *, *, #2191, .T. ) ;
#28208 = TOROIDAL_SURFACE ( 'NONE', #15993, 10.49999999999999822, 0.5000000000000000000 ) ;
#28209 = CARTESIAN_POINT ( 'NONE',  ( 0.000000000000000000, 0.000000000000000000, 0.000000000000000000 ) ) ;
#28210 = CARTESIAN_POINT ( 'NONE',  ( 0.000000000000000000, 0.000000000000000000, 0.000000000000000000 ) ) ;
#28211 = EDGE_CURVE ( 'NONE', #2390, #17791, #13975, .T. ) ;
#28212 = CARTESIAN_POINT ( 'NONE',  ( 107.1247167782375556, -1.849990392679301543, 2.220446049250313081E-13 ) ) ;
#28213 = ORIENTED_EDGE ( 'NONE', *, *, #3679, .F. ) ;
#28214 = CARTESIAN_POINT ( 'NONE',  ( 124.9999999999999432, -65.50000000000000000, 8.000000000000007105 ) ) ;
#28215 =( BOUNDED_CURVE ( )  B_SPLINE_CURVE ( 2, ( #2750, #12469, #28685, #9834, #23812, #28843, #21809, #16634, #444 ),
 .UNSPECIFIED., .F., .T. ) 
 B_SPLINE_CURVE_WITH_KNOTS ( ( 3, 2, 2, 2, 3 ),
 ( 0.3823529411764705621, 0.3897058823529411242, 0.3970588235294117974, 0.4044117647058823595, 0.4117647058823529216 ),
 .UNSPECIFIED. ) 
 CURVE ( )  GEOMETRIC_REPRESENTATION_ITEM ( )  RATIONAL_B_SPLINE_CURVE ( ( 1.000000000000000000, 0.9238795325112867385, 1.000000000000000000, 0.9238795325112867385, 1.000000000000000000, 0.9238795325112867385, 1.000000000000000000, 0.9238795325112867385, 1.000000000000000000 ) ) 
 REPRESENTATION_ITEM ( '' )  );
#28216 = ORIENTED_EDGE ( 'NONE', *, *, #1506, .F. ) ;
#28217 = CARTESIAN_POINT ( 'NONE',  ( 151.0312500000000568, -2.485281374238555774, -6.000000000000005329 ) ) ;
#28218 = VERTEX_POINT ( 'NONE', #3739 ) ;
#28219 = AXIS2_PLACEMENT_3D ( 'NONE', #18089, #17790, #8214 ) ;
#28220 = CARTESIAN_POINT ( 'NONE',  ( -3.175426480542816510, 5.499999999999865885, -115.3750000000000000 ) ) ;
#28221 = CARTESIAN_POINT ( 'NONE',  ( 23.43750000000010303, 2.649519052838419153, 1.097466725451499370 ) ) ;
#28222 = CARTESIAN_POINT ( 'NONE',  ( -5.412658773652739619, 3.124999999999975131, -129.1830127018922667 ) ) ;
#28223 = VERTEX_POINT ( 'NONE', #4353 ) ;
#28224 = CARTESIAN_POINT ( 'NONE',  ( -5.412658773652739619, 3.124999999999975131, -167.3169872981078470 ) ) ;
#28225 = CARTESIAN_POINT ( 'NONE',  ( 110.1874999999997584, 1.035533905932779275, 2.500000000000205169 ) ) ;
#28226 = CARTESIAN_POINT ( 'NONE',  ( 131.5163997308104626, 4.999999999999989342, 2.071067811865468400 ) ) ;
#28227 = EDGE_LOOP ( 'NONE', ( #4044, #3865, #18766, #8399 ) ) ;
#28228 = VECTOR ( 'NONE', #19599, 1000.000000000000000 ) ;
#28229 = CARTESIAN_POINT ( 'NONE',  ( 109.6636751345946976, -1.414213562373145550, 1.414213562373256572 ) ) ;
#28230 = DIRECTION ( 'NONE',  ( 0.000000000000000000, -2.081668171172248940E-17, 1.000000000000000000 ) ) ;
#28231 = CARTESIAN_POINT ( 'NONE',  ( -4.763139720814407951, -2.750000000000016431, -179.5000000000000000 ) ) ;
#28232 = CARTESIAN_POINT ( 'NONE',  ( 108.4377832217621318, 1.849990392679532247, 0.7662911109080692285 ) ) ;
#28233 = CARTESIAN_POINT ( 'NONE',  ( 2.775557561562891351E-14, -6.250000000000061284, -178.1830127018922383 ) ) ;
#28234 = CARTESIAN_POINT ( 'NONE',  ( 119.5386751345946692, 2.775557561562891351E-14, 2.000000000000223821 ) ) ;
#28235 = EDGE_CURVE ( 'NONE', #29963, #18576, #20217, .T. ) ;
#28236 = DIRECTION ( 'NONE',  ( -7.147005652999508048E-36, 5.642372883946980038E-36, 1.000000000000000000 ) ) ;
#28237 = CARTESIAN_POINT ( 'NONE',  ( -5.999999999999963585, -1.487416814333745711E-14, -122.9136751345948255 ) ) ;
#28238 = CARTESIAN_POINT ( 'NONE',  ( 4.763139720814407951, 2.750000000000002665, -111.2500000000000142 ) ) ;
#28239 = CARTESIAN_POINT ( 'NONE',  ( 134.9999999999992895, -6.982120021884476557, -8.500000000000007105 ) ) ;
#28240 = DIRECTION ( 'NONE',  ( -8.326672684688675286E-17, -2.081668171172168821E-17, 1.000000000000000000 ) ) ;
#28241 = ORIENTED_EDGE ( 'NONE', *, *, #16101, .F. ) ;
#28242 = CARTESIAN_POINT ( 'NONE',  ( 19.93750000000012434, -1.097466725451379244, 2.649519052838238409 ) ) ;
#28243 = CARTESIAN_POINT ( 'NONE',  ( 8.673617379884035472E-16, -16.43939393939395188, 5.999693900976774685 ) ) ;
#28244 = CYLINDRICAL_SURFACE ( 'NONE', #8178, 2.000000000000012879 ) ;
#28245 = CARTESIAN_POINT ( 'NONE',  ( 116.6011751345946408, -0.8284271247461753029, 2.000000000000332179 ) ) ;
#28246 = EDGE_CURVE ( 'NONE', #18017, #28127, #11817, .T. ) ;
#28247 = EDGE_CURVE ( 'NONE', #19083, #23968, #11074, .T. ) ;
#28248 = ORIENTED_EDGE ( 'NONE', *, *, #24090, .T. ) ;
#28249 = DIRECTION ( 'NONE',  ( -0.000000000000000000, 1.000000000000000000, 0.000000000000000000 ) ) ;
#28250 = CARTESIAN_POINT ( 'NONE',  ( 116.0000000000000142, 6.735557395310442023E-16, 5.500000000000000000 ) ) ;
#28251 = DIRECTION ( 'NONE',  ( -7.147005652999508048E-36, 5.642372883946980038E-36, 1.000000000000000000 ) ) ;
#28252 = CARTESIAN_POINT ( 'NONE',  ( 5.196152422706629359, -2.999999999999988898, -95.28867513459482552 ) ) ;
#28253 = CARTESIAN_POINT ( 'NONE',  ( 140.7113248654052313, 5.500000000000005329, 0.000000000000000000 ) ) ;
#28254 = EDGE_LOOP ( 'NONE', ( #9273, #20884, #28684, #20948, #18465 ) ) ;
#28255 = ORIENTED_EDGE ( 'NONE', *, *, #9466, .T. ) ;
#28256 = CARTESIAN_POINT ( 'NONE',  ( 152.3363248654052029, 0.000000000000000000, -5.500000000000005329 ) ) ;
#28257 = CARTESIAN_POINT ( 'NONE',  ( 136.9687500000000000, -2.485281374238585972, 6.000000000000005329 ) ) ;
#28258 = CIRCLE ( 'NONE', #22889, 30.00000000000000000 ) ;
#28259 = CARTESIAN_POINT ( 'NONE',  ( -3.608439182435115633, 6.249999999999965361, -140.4419872981078470 ) ) ;
#28260 = FACE_OUTER_BOUND ( 'NONE', #2362, .T. ) ;
#28261 = CARTESIAN_POINT ( 'NONE',  ( 144.1011751345948539, 3.889087296526011706, -3.889087296526011706 ) ) ;
#28262 = CARTESIAN_POINT ( 'NONE',  ( 18.81250000000011013, 0.8284271247462354770, -2.000000000000091926 ) ) ;
#28263 = CARTESIAN_POINT ( 'NONE',  ( 8.673617379884035472E-16, -14.14213562373095634, 8.500000000000007105 ) ) ;
#28264 = DIRECTION ( 'NONE',  ( 1.000000000000000000, -0.000000000000000000, -0.000000000000000000 ) ) ;
#28265 = CARTESIAN_POINT ( 'NONE',  ( 144.4538997308104626, -2.071067811865468400, -4.999999999999989342 ) ) ;
#28266 = DIRECTION ( 'NONE',  ( 0.000000000000000000, 5.551115123125767911E-17, -1.000000000000000000 ) ) ;
#28267 = CARTESIAN_POINT ( 'NONE',  ( 6.000000000000052403, -1.607695154586662678, -69.73066243270262987 ) ) ;
#28268 = CARTESIAN_POINT ( 'NONE',  ( -5.196152422706601826, 2.999999999999975131, -146.4613248654052029 ) ) ;
#28269 = CARTESIAN_POINT ( 'NONE',  ( 156.6636751345948255, 0.000000000000000000, 5.500000000000005329 ) ) ;
#28270 = DIRECTION ( 'NONE',  ( 0.000000000000000000, 0.000000000000000000, -1.000000000000000000 ) ) ;
#28271 = CARTESIAN_POINT ( 'NONE',  ( 109.2499999999999147, 0.000000000000000000, 2.499999999999946709 ) ) ;
#28272 = EDGE_CURVE ( 'NONE', #24844, #12427, #6427, .T. ) ;
#28273 = AXIS2_PLACEMENT_3D ( 'NONE', #23874, #3409, #24169 ) ;
#28274 = VERTEX_POINT ( 'NONE', #30164 ) ;
#28275 = AXIS2_PLACEMENT_3D ( 'NONE', #25979, #23839, #2774 ) ;
#28276 = CARTESIAN_POINT ( 'NONE',  ( 6.350852961086080661, -9.614813431917819062E-14, -48.37500000000000711 ) ) ;
#28277 = CARTESIAN_POINT ( 'NONE',  ( 6.000000000000000888, 1.743066579297358182E-13, -53.16367513459481131 ) ) ;
#28278 = EDGE_CURVE ( 'NONE', #6130, #13456, #22148, .T. ) ;
#28279 = CARTESIAN_POINT ( 'NONE',  ( 0.000000000000000000, 5.999999999999977796, -79.21132486540521711 ) ) ;
#28280 = CARTESIAN_POINT ( 'NONE',  ( 5.999999999999999112, 2.951592740943527306E-14, -163.5863248654052313 ) ) ;
#28281 = VERTEX_POINT ( 'NONE', #9127 ) ;
#28282 = CARTESIAN_POINT ( 'NONE',  ( 117.4372167782373566, 0.7662911109078888172, -1.849990392679411677 ) ) ;
#28283 = CARTESIAN_POINT ( 'NONE',  ( 139.5937500000000568, 6.000000000000005329, 2.485281374238585972 ) ) ;
#28284 = CARTESIAN_POINT ( 'NONE',  ( -3.608439182435115633, 6.249999999999965361, -101.4419872981078328 ) ) ;
#28285 = CARTESIAN_POINT ( 'NONE',  ( 142.5074251345948255, 2.278174593051965235, -5.500000000000058620 ) ) ;
#28286 = CARTESIAN_POINT ( 'NONE',  ( 133.9687500000000284, -2.485281374238585972, 6.000000000000005329 ) ) ;
#28287 = CARTESIAN_POINT ( 'NONE',  ( 118.8749999999998295, 1.767766952966320915, -1.767766952966320915 ) ) ;
#28288 = VERTEX_POINT ( 'NONE', #18520 ) ;
#28289 = AXIS2_PLACEMENT_3D ( 'NONE', #1517, #22587, #6280 ) ;
#28290 = AXIS2_PLACEMENT_3D ( 'NONE', #25105, #26826, #8097 ) ;
#28291 = CARTESIAN_POINT ( 'NONE',  ( -4.763139720814407951, -2.750000000000016431, -131.5000000000000000 ) ) ;
#28292 = ORIENTED_EDGE ( 'NONE', *, *, #20411, .F. ) ;
#28293 = CARTESIAN_POINT ( 'NONE',  ( 6.000000000000000888, 1.743066579297358182E-13, -81.66367513459481131 ) ) ;
#28294 = CARTESIAN_POINT ( 'NONE',  ( 0.000000000000000000, 5.499999999999991118, -63.00000000000000000 ) ) ;
#28295 = CARTESIAN_POINT ( 'NONE',  ( -20.99999999999998224, -25.00000000000010658, 4.000000000000003553 ) ) ;
#28296 =( BOUNDED_CURVE ( )  B_SPLINE_CURVE ( 2, ( #27253, #8057, #7911, #15488, #27106, #5751, #24498, #13032, #24812 ),
 .UNSPECIFIED., .F., .F. ) 
 B_SPLINE_CURVE_WITH_KNOTS ( ( 3, 2, 2, 2, 3 ),
 ( 0.8805555555555555358, 0.8814814814814815325, 0.8833333333333333037, 0.8851851851851851860, 0.8861111111111110716 ),
 .UNSPECIFIED. ) 
 CURVE ( )  GEOMETRIC_REPRESENTATION_ITEM ( )  RATIONAL_B_SPLINE_CURVE ( ( 0.9330127018922194093, 0.9330127018922154125, 1.000000000000000000, 0.8660254037844388186, 1.000000000000000000, 0.8660254037844388186, 1.000000000000000000, 0.9330127018922234061, 0.9330127018922194093 ) ) 
 REPRESENTATION_ITEM ( '' )  );
#28297 = CARTESIAN_POINT ( 'NONE',  ( 5.412658773652712085, -3.125000000000086153, -86.43301270189223828 ) ) ;
#28298 = LINE ( 'NONE', #659, #2518 ) ;
#28299 = STYLED_ITEM ( 'NONE', ( #6841 ), #17780 ) ;
#28300 = CARTESIAN_POINT ( 'NONE',  ( 139.5000000000000000, -9.165151389911669000, 8.000000000000007105 ) ) ;
#28301 = CARTESIAN_POINT ( 'NONE',  ( 104.9372167782373566, -0.7662911109077388261, 1.849990392679772278 ) ) ;
#28302 = CARTESIAN_POINT ( 'NONE',  ( 5.196152422706629359, -2.999999999999988898, -175.7113248654052029 ) ) ;
#28303 = EDGE_CURVE ( 'NONE', #13966, #16234, #11911, .T. ) ;
#28304 = CARTESIAN_POINT ( 'NONE',  ( 117.3127832217621318, 1.849990392679532247, -0.7662911109076485650 ) ) ;
#28305 = EDGE_CURVE ( 'NONE', #11174, #6130, #28485, .T. ) ;
#28306 =( BOUNDED_CURVE ( )  B_SPLINE_CURVE ( 2, ( #24281, #14510, #19694, #5536, #484, #3381, #3228, #17260, #26287 ),
 .UNSPECIFIED., .F., .T. ) 
 B_SPLINE_CURVE_WITH_KNOTS ( ( 3, 2, 2, 2, 3 ),
 ( 0.9694444444444444420, 0.9703703703703703276, 0.9722222222222222099, 0.9740740740740740922, 0.9750000000000000888 ),
 .UNSPECIFIED. ) 
 CURVE ( )  GEOMETRIC_REPRESENTATION_ITEM ( )  RATIONAL_B_SPLINE_CURVE ( ( 0.9330127018922194093, 0.9330127018922194093, 1.000000000000000000, 0.8660254037844388186, 1.000000000000000000, 0.8660254037844388186, 1.000000000000000000, 0.9330127018922154125, 0.9330127018922194093 ) ) 
 REPRESENTATION_ITEM ( '' )  );
#28307 = CARTESIAN_POINT ( 'NONE',  ( -6.350852961085760029, -1.281975124255709124E-13, -137.6250000000000568 ) ) ;
#28308 = DIRECTION ( 'NONE',  ( -5.551115123125785167E-17, 1.000000000000000000, 8.881784197001256268E-16 ) ) ;
#28309 = CARTESIAN_POINT ( 'NONE',  ( 7.216878364870455975, -6.409875621278545621E-14, -156.8080127018922667 ) ) ;
#28310 = SURFACE_SIDE_STYLE ('',( #9750 ) ) ;
#28311 = CARTESIAN_POINT ( 'NONE',  ( -5.999999999999963585, 1.780251999655701777E-13, -73.41367513459483973 ) ) ;
#28312 = CARTESIAN_POINT ( 'NONE',  ( -3.175426480542816066, -5.500000000000057732, -81.87500000000002842 ) ) ;
#28313 = CIRCLE ( 'NONE', #12194, 11.00000000000000355 ) ;
#28314 = CARTESIAN_POINT ( 'NONE',  ( -3.464101615137725076, 5.999999999999979572, -114.1636751345948113 ) ) ;
#28315 = PLANE ( 'NONE',  #23474 ) ;
#28316 = CARTESIAN_POINT ( 'NONE',  ( -4.763139720814407951, -2.750000000000016431, -68.50000000000000000 ) ) ;
#28317 = CARTESIAN_POINT ( 'NONE',  ( -5.196152422706573404, -3.000000000000002665, -148.2886751345948824 ) ) ;
#28318 = CARTESIAN_POINT ( 'NONE',  ( 160.5000000000000284, 6.000000000000005329, 0.000000000000000000 ) ) ;
#28319 =( LENGTH_UNIT ( ) NAMED_UNIT ( * ) SI_UNIT ( .MILLI., .METRE. ) );
#28320 = DIRECTION ( 'NONE',  ( -7.147005652999508048E-36, 5.642372883946980038E-36, 1.000000000000000000 ) ) ;
#28321 = CARTESIAN_POINT ( 'NONE',  ( 118.6872167782374703, 1.849990392679501827, 0.7662911109080090544 ) ) ;
#28322 = CARTESIAN_POINT ( 'NONE',  ( 0.000000000000000000, -5.999999999999991118, -145.0386751345948539 ) ) ;
#28323 = VERTEX_POINT ( 'NONE', #4657 ) ;
#28324 = CARTESIAN_POINT ( 'NONE',  ( 152.0625000000000568, -4.242640687119298093, 4.242640687119298093 ) ) ;
#28325 = CARTESIAN_POINT ( 'NONE',  ( 14.52382486540527928, 1.035533905932809473, -2.499999999999904521 ) ) ;
#28326 = AXIS2_PLACEMENT_3D ( 'NONE', #13944, #16691, #4961 ) ;
#28327 = CARTESIAN_POINT ( 'NONE',  ( 6.000000000000000888, -3.330669073875464691E-16, -7.560779664488942560E-35 ) ) ;
#28328 = VECTOR ( 'NONE', #4229, 1000.000000000000000 ) ;
#28329 = CARTESIAN_POINT ( 'NONE',  ( 20.93750000000008171, 2.000000000000212275, -0.8284271247463557142 ) ) ;
#28330 = VERTEX_POINT ( 'NONE', #28300 ) ;
#28331 = ORIENTED_EDGE ( 'NONE', *, *, #2719, .F. ) ;
#28332 = CARTESIAN_POINT ( 'NONE',  ( 0.000000000000000000, 5.499999999999991118, -87.00000000000002842 ) ) ;
#28333 = VECTOR ( 'NONE', #12879, 1000.000000000000000 ) ;
#28334 = CARTESIAN_POINT ( 'NONE',  ( 7.216878364870455975, -6.409875621278545621E-14, -99.80801270189222407 ) ) ;
#28335 = VERTEX_POINT ( 'NONE', #7280 ) ;
#28336 = CARTESIAN_POINT ( 'NONE',  ( 153.8288997308104058, 4.999999999999989342, -2.071067811865468400 ) ) ;
#28337 = CARTESIAN_POINT ( 'NONE',  ( -3.175426480542816510, -5.500000000000057732, -167.3750000000000568 ) ) ;
#28338 = DIRECTION ( 'NONE',  ( -1.000000000000000000, -1.665334536937736783E-16, -2.220446049250315546E-16 ) ) ;
#28339 = DIRECTION ( 'NONE',  ( 0.000000000000000000, 0.000000000000000000, -1.000000000000000000 ) ) ;
#28340 = CARTESIAN_POINT ( 'NONE',  ( -5.196152422706601826, 2.999999999999975131, -93.03867513459485394 ) ) ;
#28341 = EDGE_CURVE ( 'NONE', #3216, #6343, #29878, .T. ) ;
#28342 = CARTESIAN_POINT ( 'NONE',  ( 144.0863248654052313, 0.000000000000000000, 5.500000000000005329 ) ) ;
#28343 = CARTESIAN_POINT ( 'NONE',  ( -4.763139720814407951, -2.750000000000016431, -158.5000000000000284 ) ) ;
#28344 = CARTESIAN_POINT ( 'NONE',  ( 110.7499999999998010, 2.775557561562891351E-14, -2.499999999999946709 ) ) ;
#28345 = CARTESIAN_POINT ( 'NONE',  ( -6.350852961085760029, -1.281975124255709124E-13, -103.1250000000000142 ) ) ;
#28346 = CARTESIAN_POINT ( 'NONE',  ( 3.464101615137852974, 5.999999999999884537, -59.83632486540521001 ) ) ;
#28348 = CARTESIAN_POINT ( 'NONE',  ( 0.000000000000000000, 5.499999999999991118, -93.00000000000002842 ) ) ;
#28347 = CARTESIAN_POINT ( 'NONE',  ( -4.763139720814407951, 2.749999999999946709, -155.7500000000000568 ) ) ;
#28349 = CARTESIAN_POINT ( 'NONE',  ( 155.7336002691896226, -4.999999999999989342, 2.071067811865468400 ) ) ;
#28350 = DIRECTION ( 'NONE',  ( -1.000000000000000000, -1.067522139062651411E-16, 0.000000000000000000 ) ) ;
#28351 = ORIENTED_EDGE ( 'NONE', *, *, #7338, .F. ) ;
#28352 = CARTESIAN_POINT ( 'NONE',  ( 23.93750000000006750, 2.000000000000151879, -0.8284271247462955401 ) ) ;
#28353 = UNCERTAINTY_MEASURE_WITH_UNIT (LENGTH_MEASURE( 1.000000000000000082E-05 ), #21236, 'distance_accuracy_value', 'NONE');
#28354 = CARTESIAN_POINT ( 'NONE',  ( 111.1874999999999858, 1.035533905932749299, 2.500000000000265121 ) ) ;
#28355 = CARTESIAN_POINT ( 'NONE',  ( 112.1488248654050892, -1.999999999999941602, 0.8284271247463557142 ) ) ;
#28356 = CARTESIAN_POINT ( 'NONE',  ( 106.4377832217622029, 1.849990392679562001, 0.7662911109078287542 ) ) ;
#28357 = CARTESIAN_POINT ( 'NONE',  ( 112.8363248654051318, 1.414213562373201061, 1.414213562373256572 ) ) ;
#28358 = EDGE_LOOP ( 'NONE', ( #6378, #27524, #19580, #15777 ) ) ;
#28359 = CARTESIAN_POINT ( 'NONE',  ( 146.1636751345948255, 0.000000000000000000, 5.500000000000005329 ) ) ;
#28360 = VERTEX_POINT ( 'NONE', #10498 ) ;
#28361 = VERTEX_POINT ( 'NONE', #28449 ) ;
#28362 = EDGE_LOOP ( 'NONE', ( #4544, #18500, #27719 ) ) ;
#28363 = ADVANCED_FACE ( 'NONE', ( #26301 ), #10042, .T. ) ;
#28364 = CARTESIAN_POINT ( 'NONE',  ( -4.763139720814407951, 2.749999999999946709, -112.2500000000000142 ) ) ;
#28365 = CARTESIAN_POINT ( 'NONE',  ( 18.18750000000008882, 1.097466725451619718, -2.649519052838358757 ) ) ;
#28366 = CARTESIAN_POINT ( 'NONE',  ( 2.775557561562891351E-14, 6.250000000000033751, -120.4330127018922099 ) ) ;
#28367 = UNCERTAINTY_MEASURE_WITH_UNIT (LENGTH_MEASURE( 1.000000000000000082E-05 ), #26791, 'distance_accuracy_value', 'NONE');
#28368 = ORIENTED_EDGE ( 'NONE', *, *, #12482, .T. ) ;
#28369 = FILL_AREA_STYLE ('',( #6890 ) ) ;
#28370 = CARTESIAN_POINT ( 'NONE',  ( 7.216878364870455975, -6.409875621278545621E-14, -172.4419872981078470 ) ) ;
#28371 = CARTESIAN_POINT ( 'NONE',  ( 106.6249999999999289, -1.767766952966376426, -1.767766952966320915 ) ) ;
#28372 = CARTESIAN_POINT ( 'NONE',  ( 131.4226497308104058, 5.000000000000004441, 0.000000000000000000 ) ) ;
#28373 = VERTEX_POINT ( 'NONE', #5552 ) ;
#28374 = EDGE_CURVE ( 'NONE', #16705, #3266, #14239, .T. ) ;
#28375 = CYLINDRICAL_SURFACE ( 'NONE', #10101, 0.5000000000000004441 ) ;
#28376 = CYLINDRICAL_SURFACE ( 'NONE', #4979, 5.500000000000000000 ) ;
#28377 = CARTESIAN_POINT ( 'NONE',  ( -4.763139720814407951, 2.749999999999946709, -178.2500000000000284 ) ) ;
#28378 = CARTESIAN_POINT ( 'NONE',  ( 107.7502832217622881, -1.308140751793585022, 1.308140751793751555 ) ) ;
#28379 = CARTESIAN_POINT ( 'NONE',  ( 5.412658773652739619, 3.124999999999988898, -173.1830127018922383 ) ) ;
#28380 = DIRECTION ( 'NONE',  ( 1.000000000000000000, 0.000000000000000000, 0.000000000000000000 ) ) ;
#28381 = CARTESIAN_POINT ( 'NONE',  ( -5.196152422706573404, -3.000000000000002665, -101.7886751345948255 ) ) ;
#28382 = CARTESIAN_POINT ( 'NONE',  ( 162.0000000000000284, 0.000000000000000000, -11.00000000000000355 ) ) ;
#28383 = UNCERTAINTY_MEASURE_WITH_UNIT (LENGTH_MEASURE( 1.000000000000000082E-05 ), #314, 'distance_accuracy_value', 'NONE');
#28384 = CARTESIAN_POINT ( 'NONE',  ( -6.350852961085760029, -1.281975124255709124E-13, -115.1250000000000000 ) ) ;
#28385 = CARTESIAN_POINT ( 'NONE',  ( -5.999999999999963585, -1.487416814333745711E-14, -165.8363248654052029 ) ) ;
#28386 = CARTESIAN_POINT ( 'NONE',  ( 10.00000000000012079, -0.6095397823829284967, 2.424553825692621345 ) ) ;
#28387 = ORIENTED_EDGE ( 'NONE', *, *, #15058, .F. ) ;
#28388 = CARTESIAN_POINT ( 'NONE',  ( 17.18750000000004263, -2.649519052838178457, -1.097466725451619718 ) ) ;
#28389 = CARTESIAN_POINT ( 'NONE',  ( 6.000000000000000888, -3.330669073875464691E-16, -7.560779664488942560E-35 ) ) ;
#28390 = CARTESIAN_POINT ( 'NONE',  ( 0.000000000000000000, 5.999999999999977796, -109.2113248654051887 ) ) ;
#28391 = CARTESIAN_POINT ( 'NONE',  ( 135.0525775163646074, 3.054031077158521068, -4.724143515893503675 ) ) ;
#28392 =( BOUNDED_CURVE ( )  B_SPLINE_CURVE ( 2, ( #24602, #3399, #8017, #17123, #7717, #1251, #26893, #15274, #10660 ),
 .UNSPECIFIED., .F., .T. ) 
 B_SPLINE_CURVE_WITH_KNOTS ( ( 3, 2, 2, 2, 3 ),
 ( 0.2138888888888888784, 0.2148148148148148195, 0.2166666666666666741, 0.2185185185185185286, 0.2194444444444444697 ),
 .UNSPECIFIED. ) 
 CURVE ( )  GEOMETRIC_REPRESENTATION_ITEM ( )  RATIONAL_B_SPLINE_CURVE ( ( 0.9330127018922196314, 0.9330127018922185211, 1.000000000000000000, 0.8660254037844388186, 1.000000000000000000, 0.8660254037844388186, 1.000000000000000000, 0.9330127018922184101, 0.9330127018922194093 ) ) 
 REPRESENTATION_ITEM ( '' )  );
#28393 = ORIENTED_EDGE ( 'NONE', *, *, #8773, .F. ) ;
#28394 = CARTESIAN_POINT ( 'NONE',  ( -5.999999999999963585, 1.780251999655701777E-13, -98.91367513459483973 ) ) ;
#28395 = CARTESIAN_POINT ( 'NONE',  ( 3.175426480543072749, -5.500000000000105693, -177.6250000000000284 ) ) ;
#28396 = CIRCLE ( 'NONE', #17644, 0.5000000000000000000 ) ;
#28397 = ORIENTED_EDGE ( 'NONE', *, *, #2756, .T. ) ;
#28398 = CARTESIAN_POINT ( 'NONE',  ( 5.196152422706629359, -2.999999999999988898, -77.28867513459481131 ) ) ;
#28399 = MECHANICAL_DESIGN_GEOMETRIC_PRESENTATION_REPRESENTATION (  '', ( #18137 ), #29381 ) ;
#28400 = CARTESIAN_POINT ( 'NONE',  ( 141.0863248654052313, 0.000000000000000000, 5.500000000000005329 ) ) ;
#28401 = ORIENTED_EDGE ( 'NONE', *, *, #24850, .T. ) ;
#28402 = EDGE_LOOP ( 'NONE', ( #10220, #26465, #9771, #17404 ) ) ;
#28403 = CARTESIAN_POINT ( 'NONE',  ( -5.999999999999944933, 1.607695154586759934, -140.9806624327026157 ) ) ;
#28404 = CARTESIAN_POINT ( 'NONE',  ( 133.9687500000000284, -2.485281374238585972, 6.000000000000005329 ) ) ;
#28405 = ADVANCED_FACE ( 'NONE', ( #8016 ), #16975, .T. ) ;
#28406 = CARTESIAN_POINT ( 'NONE',  ( -5.412658773652739619, 3.124999999999975131, -138.8169872981078186 ) ) ;
#28407 = CARTESIAN_POINT ( 'NONE',  ( 0.000000000000000000, 0.000000000000000000, 0.000000000000000000 ) ) ;
#28408 = CARTESIAN_POINT ( 'NONE',  ( 11.00000000000001599, -6.106226635438360972E-16, -1.386142938489641429E-34 ) ) ;
#28409 = CARTESIAN_POINT ( 'NONE',  ( 20.00000000000004619, 2.000000000000057288, -5.551115123125782702E-14 ) ) ;
#28410 = CARTESIAN_POINT ( 'NONE',  ( -6.000000000000000888, 1.067854986875958443E-15, 7.560779664488942560E-35 ) ) ;
#28411 = ADVANCED_FACE ( 'NONE', ( #3396 ), #13837, .F. ) ;
#28412 = CARTESIAN_POINT ( 'NONE',  ( -0.5000000000000014433, -10.00000000000000711, 4.414213562373099364 ) ) ;
#28413 = ADVANCED_FACE ( 'NONE', ( #22008 ), #17122, .T. ) ;
#28414 = CARTESIAN_POINT ( 'NONE',  ( 138.5476497308104058, 0.000000000000000000, -5.000000000000004441 ) ) ;
#28415 = CARTESIAN_POINT ( 'NONE',  ( 3.464101615137757051, -5.999999999999979572, -119.4136751345948397 ) ) ;
#28416 = CARTESIAN_POINT ( 'NONE',  ( 3.464101615137852974, 5.999999999999884537, -92.83632486540514606 ) ) ;
#28417 = DIRECTION ( 'NONE',  ( 1.526556658859587038E-16, -2.081668171172187002E-17, 1.000000000000000000 ) ) ;
#28418 = CARTESIAN_POINT ( 'NONE',  ( 24.56825942016106623, -1.021360606787547365, 2.212070257063908585 ) ) ;
#28419 =( LENGTH_UNIT ( ) NAMED_UNIT ( * ) SI_UNIT ( .MILLI., .METRE. ) );
#28420 = CARTESIAN_POINT ( 'NONE',  ( 105.2499999999999147, -2.775557561562891351E-14, 2.499999999999946709 ) ) ;
#28421 = CARTESIAN_POINT ( 'NONE',  ( 114.7886751345947403, -1.999999999999946265, 0.000000000000000000 ) ) ;
#28422 = CARTESIAN_POINT ( 'NONE',  ( 154.3199251345948539, -2.278174593051950136, -5.500000000000074607 ) ) ;
#28423 = VERTEX_POINT ( 'NONE', #500 ) ;
#28424 =( GEOMETRIC_REPRESENTATION_CONTEXT ( 3 ) GLOBAL_UNCERTAINTY_ASSIGNED_CONTEXT ( ( #13044 ) ) GLOBAL_UNIT_ASSIGNED_CONTEXT ( ( #10235, #21302, #26189 ) ) REPRESENTATION_CONTEXT ( 'NONE', 'WORKASPACE' ) );
#28425 = CARTESIAN_POINT ( 'NONE',  ( -4.763139720814407951, -2.750000000000016431, -50.49999999999998579 ) ) ;
#28426 = CARTESIAN_POINT ( 'NONE',  ( -5.999999999999956479, -1.607695154586745057, -133.3466878364870354 ) ) ;
#28427 = CARTESIAN_POINT ( 'NONE',  ( 1.110223024625156540E-13, 6.000000000000172307, 0.000000000000000000 ) ) ;
#28428 = ORIENTED_EDGE ( 'NONE', *, *, #21100, .T. ) ;
#28429 = CARTESIAN_POINT ( 'NONE',  ( 116.2497167782374845, -1.308140751793585022, -1.308140751793640533 ) ) ;
#28430 = DIRECTION ( 'NONE',  ( 0.000000000000000000, -2.755434769241566700E-14, 1.000000000000000000 ) ) ;
#28431 = CARTESIAN_POINT ( 'NONE',  ( -5.412658773652739619, 3.124999999999975131, -102.8169872981078470 ) ) ;
#28432 = CARTESIAN_POINT ( 'NONE',  ( 138.3675748654052029, -5.500000000000012434, 2.278174593052012309 ) ) ;
#28433 = CARTESIAN_POINT ( 'NONE',  ( 160.6726497308104058, -5.000000000000004441, 0.000000000000000000 ) ) ;
#28434 = CARTESIAN_POINT ( 'NONE',  ( 119.4999999999999289, -2.499999999999919176, 0.000000000000000000 ) ) ;
#28435 =( BOUNDED_CURVE ( )  B_SPLINE_CURVE ( 2, ( #10775, #1064, #17683, #29004, #5505, #7969, #20123, #14913, #26694 ),
 .UNSPECIFIED., .F., .F. ) 
 B_SPLINE_CURVE_WITH_KNOTS ( ( 3, 2, 2, 2, 3 ),
 ( 0.6583333333333333259, 0.6592592592592592116, 0.6611111111111110938, 0.6629629629629629761, 0.6638888888888889728 ),
 .UNSPECIFIED. ) 
 CURVE ( )  GEOMETRIC_REPRESENTATION_ITEM ( )  RATIONAL_B_SPLINE_CURVE ( ( 0.9330127018922194093, 0.9330127018922194093, 1.000000000000000000, 0.8660254037844388186, 1.000000000000000000, 0.8660254037844388186, 1.000000000000000000, 0.9330127018922114157, 0.9330127018922194093 ) ) 
 REPRESENTATION_ITEM ( '' )  );
#28436 = EDGE_CURVE ( 'NONE', #22235, #11502, #21864, .T. ) ;
#28437 = COLOUR_RGB ( '', 0.40784314, 0.44705882, 0.49803922) ;
#28438 = CARTESIAN_POINT ( 'NONE',  ( -3.175426480542816510, 5.499999999999865885, -131.8750000000000000 ) ) ;
#28439 = PRESENTATION_LAYER_ASSIGNMENT (  '', '', ( #1477 ) ) ;
#28440 = ORIENTED_EDGE ( 'NONE', *, *, #24185, .T. ) ;
#28441 = ORIENTED_EDGE ( 'NONE', *, *, #19582, .T. ) ;
#28442 = CARTESIAN_POINT ( 'NONE',  ( -2.775557561562891351E-14, -5.500000000000115463, -56.25000000000002132 ) ) ;
#28443 = LINE ( 'NONE', #16826, #820 ) ;
#28444 = DIRECTION ( 'NONE',  ( -1.000000000000000000, -0.000000000000000000, 0.000000000000000000 ) ) ;
#28445 = EDGE_CURVE ( 'NONE', #2534, #4196, #26720, .T. ) ;
#28446 = CARTESIAN_POINT ( 'NONE',  ( -5.412658773652684552, -3.125000000000099920, -85.43301270189223828 ) ) ;
#28447 = UNCERTAINTY_MEASURE_WITH_UNIT (LENGTH_MEASURE( 1.000000000000000082E-05 ), #19456, 'distance_accuracy_value', 'NONE');
#28448 = CARTESIAN_POINT ( 'NONE',  ( 9.999999999999841904, 2.000000000000057288, -4.274358644806852681E-12 ) ) ;
#28449 = CARTESIAN_POINT ( 'NONE',  ( -1.000000000000000888, 10.00000000000000888, 3.000000000000002665 ) ) ;
#28450 = CARTESIAN_POINT ( 'NONE',  ( 107.5622167782374561, 1.849990392679472073, -0.7662911109077686911 ) ) ;
#28451 = CARTESIAN_POINT ( 'NONE',  ( 124.9999999999999432, -65.50000000000000000, -7.500000000000007105 ) ) ;
#28452 = CARTESIAN_POINT ( 'NONE',  ( 6.000000000000000888, -1.859271017917181981E-14, -110.1636751345948397 ) ) ;
#28453 = CARTESIAN_POINT ( 'NONE',  ( 115.2502832217623592, 1.308140751793696044, -1.308140751793529510 ) ) ;
#28454 = CARTESIAN_POINT ( 'NONE',  ( -2.775557561562891351E-14, -5.500000000000115463, -140.2500000000000000 ) ) ;
#28455 = CARTESIAN_POINT ( 'NONE',  ( -5.999999999999956479, -1.607695154586745057, -105.7693375672974696 ) ) ;
#28456 = CARTESIAN_POINT ( 'NONE',  ( -3.608439182435115633, 6.249999999999965361, -154.8080127018922383 ) ) ;
#28457 = CARTESIAN_POINT ( 'NONE',  ( 6.000000000000000000, -3.330669073875464198E-16, -180.0000000000000568 ) ) ;
#28458 = STYLED_ITEM ( 'NONE', ( #23536 ), #27507 ) ;
#28459 = CARTESIAN_POINT ( 'NONE',  ( -2.775557561562891351E-14, -5.500000000000115463, -68.25000000000002842 ) ) ;
#28460 = CARTESIAN_POINT ( 'NONE',  ( 145.2113248654052313, 5.500000000000005329, 0.000000000000000000 ) ) ;
#28461 =( LENGTH_UNIT ( ) NAMED_UNIT ( * ) SI_UNIT ( .MILLI., .METRE. ) );
#28462 = CARTESIAN_POINT ( 'NONE',  ( -4.763139720814407951, 2.749999999999946709, -67.25000000000002842 ) ) ;
#28463 = CARTESIAN_POINT ( 'NONE',  ( 145.3273502691896510, -5.000000000000004441, 0.000000000000000000 ) ) ;
#28464 = CYLINDRICAL_SURFACE ( 'NONE', #13054, 6.000000000000000888 ) ;
#28465 = CARTESIAN_POINT ( 'NONE',  ( 159.0000000000000284, 6.000000000000005329, 0.000000000000000000 ) ) ;
#28466 = LINE ( 'NONE', #7434, #27071 ) ;
#28467 = CARTESIAN_POINT ( 'NONE',  ( 17.93750000000012434, 2.000000000000091926, -0.8284271247463557142 ) ) ;
#28468 = CARTESIAN_POINT ( 'NONE',  ( 6.000000000000000888, -1.859271017917181981E-14, -147.0863248654052313 ) ) ;
#28469 = DIRECTION ( 'NONE',  ( -7.147005652999508048E-36, 5.642372883946980038E-36, 1.000000000000000000 ) ) ;
#28471 = ORIENTED_EDGE ( 'NONE', *, *, #22087, .T. ) ;
#28470 = AXIS2_PLACEMENT_3D ( 'NONE', #9443, #16541, #11778 ) ;
#28472 = CARTESIAN_POINT ( 'NONE',  ( 148.1250000000000284, 0.000000000000000000, -6.000000000000005329 ) ) ;
#28473 = CARTESIAN_POINT ( 'NONE',  ( 112.5002832217623023, 1.308140751793696044, 1.308140751793640533 ) ) ;
#28474 = EDGE_CURVE ( 'NONE', #1220, #13422, #14811, .T. ) ;
#28475 = DIRECTION ( 'NONE',  ( 1.000000000000000000, -0.000000000000000000, -0.000000000000000000 ) ) ;
#28476 = UNCERTAINTY_MEASURE_WITH_UNIT (LENGTH_MEASURE( 1.000000000000000082E-05 ), #14760, 'distance_accuracy_value', 'NONE');
#28477 =( BOUNDED_CURVE ( )  B_SPLINE_CURVE ( 2, ( #16548, #6975, #28156, #2380, #63, #7126, #25870, #23580, #2517 ),
 .UNSPECIFIED., .F., .T. ) 
 B_SPLINE_CURVE_WITH_KNOTS ( ( 3, 2, 2, 2, 3 ),
 ( 0.7583333333333333037, 0.7592592592592593004, 0.7611111111111110716, 0.7629629629629629539, 0.7638888888888888395 ),
 .UNSPECIFIED. ) 
 CURVE ( )  GEOMETRIC_REPRESENTATION_ITEM ( )  RATIONAL_B_SPLINE_CURVE ( ( 0.9330127018922194093, 0.9330127018922154125, 1.000000000000000000, 0.8660254037844388186, 1.000000000000000000, 0.8660254037844388186, 1.000000000000000000, 0.9330127018922234061, 0.9330127018922194093 ) ) 
 REPRESENTATION_ITEM ( '' )  );
#28478 = EDGE_CURVE ( 'NONE', #16758, #18552, #7560, .T. ) ;
#28479 = CARTESIAN_POINT ( 'NONE',  ( 0.000000000000000000, 5.999999999999977796, -64.21132486540520290 ) ) ;
#28480 = CARTESIAN_POINT ( 'NONE',  ( -6.350852961085760029, -1.281975124255709124E-13, -179.6250000000000284 ) ) ;
#28481 = CARTESIAN_POINT ( 'NONE',  ( 19.56250000000009592, -1.999999999999911626, -0.8284271247461753029 ) ) ;
#28482 = CARTESIAN_POINT ( 'NONE',  ( 2.775557561562891351E-14, 6.250000000000033751, -154.0669872981078470 ) ) ;
#28483 = ORIENTED_EDGE ( 'NONE', *, *, #1328, .F. ) ;
#28484 = CARTESIAN_POINT ( 'NONE',  ( 4.763139720814407951, 2.750000000000002665, -79.74999999999998579 ) ) ;
#28485 = CIRCLE ( 'NONE', #2982, 10.49999999999999645 ) ;
#28486 =( BOUNDED_CURVE ( )  B_SPLINE_CURVE ( 2, ( #20676, #18386, #11328, #27703, #13637, #19650, #6525, #5644, #3489 ),
 .UNSPECIFIED., .F., .T. ) 
 B_SPLINE_CURVE_WITH_KNOTS ( ( 3, 2, 2, 2, 3 ),
 ( 0.8138888888888888840, 0.8148148148148147696, 0.8166666666666666519, 0.8185185185185185341, 0.8194444444444445308 ),
 .UNSPECIFIED. ) 
 CURVE ( )  GEOMETRIC_REPRESENTATION_ITEM ( )  RATIONAL_B_SPLINE_CURVE ( ( 0.9330127018922194093, 0.9330127018922194093, 1.000000000000000000, 0.8660254037844388186, 1.000000000000000000, 0.8660254037844388186, 1.000000000000000000, 0.9330127018922154125, 0.9330127018922194093 ) ) 
 REPRESENTATION_ITEM ( '' )  );
#28487 = ORIENTED_EDGE ( 'NONE', *, *, #5864, .F. ) ;
#28488 = AXIS2_PLACEMENT_3D ( 'NONE', #11688, #25622, #29757 ) ;
#28489 = CARTESIAN_POINT ( 'NONE',  ( -5.196152422706601826, 2.999999999999975131, -147.0386751345948539 ) ) ;
#28490 = CARTESIAN_POINT ( 'NONE',  ( 153.2663997308103774, -4.999999999999989342, -2.071067811865468400 ) ) ;
#28491 = CARTESIAN_POINT ( 'NONE',  ( 111.0386751345947118, 5.551115123125782702E-14, -2.000000000000001776 ) ) ;
#28492 = DIRECTION ( 'NONE',  ( -7.147005652999508048E-36, 5.642372883946980038E-36, 1.000000000000000000 ) ) ;
#28493 = DIRECTION ( 'NONE',  ( 1.000000000000000000, 0.000000000000000000, 0.000000000000000000 ) ) ;
#28494 = CARTESIAN_POINT ( 'NONE',  ( 4.763139720814407951, 2.750000000000002665, -160.7500000000000568 ) ) ;
#28495 = CARTESIAN_POINT ( 'NONE',  ( 3.464101615137852974, 5.999999999999884537, -161.8363248654052313 ) ) ;
#28496 = CARTESIAN_POINT ( 'NONE',  ( -4.763139720814407951, -2.750000000000016431, -155.5000000000000284 ) ) ;
#28497 = CARTESIAN_POINT ( 'NONE',  ( 111.7499999999998010, 0.000000000000000000, -2.499999999999946709 ) ) ;
#28498 = CARTESIAN_POINT ( 'NONE',  ( 6.350852961086080661, -9.614813431917819062E-14, -91.87500000000001421 ) ) ;
#28499 = CARTESIAN_POINT ( 'NONE',  ( 24.03867513459490013, 1.665334536937734811E-13, -2.500000000000002220 ) ) ;
#28500 = CARTESIAN_POINT ( 'NONE',  ( -6.350852961085760029, -1.281975124255709124E-13, -86.62499999999998579 ) ) ;
#28501 = CARTESIAN_POINT ( 'NONE',  ( 155.1711002691897079, 4.999999999999989342, 2.071067811865468400 ) ) ;
#28502 = CARTESIAN_POINT ( 'NONE',  ( 106.9761751345946266, -0.8284271247461453269, -1.999999999999791278 ) ) ;
#28503 = CARTESIAN_POINT ( 'NONE',  ( 114.9999999999999716, 2.500000000000002220, 0.000000000000000000 ) ) ;
#28504 = LINE ( 'NONE', #7330, #23242 ) ;
#28505 = CARTESIAN_POINT ( 'NONE',  ( -5.999999999999963585, 8.134310703387671600E-14, -119.3363248654052455 ) ) ;
#28506 = ORIENTED_EDGE ( 'NONE', *, *, #1744, .F. ) ;
#28507 = CARTESIAN_POINT ( 'NONE',  ( 0.000000000000000000, 5.999999999999977796, -178.7886751345948539 ) ) ;
#28508 = CYLINDRICAL_SURFACE ( 'NONE', #10881, 6.000000000000000888 ) ;
#28509 = CARTESIAN_POINT ( 'NONE',  ( 106.3747167782374703, -5.551115123125782702E-14, -1.849990392679523588 ) ) ;
#28510 = ORIENTED_EDGE ( 'NONE', *, *, #27230, .T. ) ;
#28511 = EDGE_CURVE ( 'NONE', #567, #6844, #5255, .T. ) ;
#28512 = CARTESIAN_POINT ( 'NONE',  ( -3.175426480542816510, 5.499999999999865885, -110.8750000000000426 ) ) ;
#28513 = CARTESIAN_POINT ( 'NONE',  ( 16.93750000000004619, -2.649519052838238409, -1.097466725451559322 ) ) ;
#28514 = CARTESIAN_POINT ( 'NONE',  ( 2.775557561562891351E-14, -6.250000000000061284, -127.1830127018922525 ) ) ;
#28515 = EDGE_LOOP ( 'NONE', ( #19946, #11456, #23195, #11225, #29023, #25382 ) ) ;
#28516 = CARTESIAN_POINT ( 'NONE',  ( 3.464101615137757051, -5.999999999999979572, -68.41367513459479710 ) ) ;
#28517 = CARTESIAN_POINT ( 'NONE',  ( 3.608439182435180470, -6.249999999999997335, -160.6919872981078470 ) ) ;
#28518 = CARTESIAN_POINT ( 'NONE',  ( 107.7499999999998579, 5.551115123125782702E-14, -2.499999999999946709 ) ) ;
#28519 =( BOUNDED_CURVE ( )  B_SPLINE_CURVE ( 2, ( #29785, #29160, #8123, #24565, #26856, #5815, #5982, #15232, #3516 ),
 .UNSPECIFIED., .F., .F. ) 
 B_SPLINE_CURVE_WITH_KNOTS ( ( 3, 2, 2, 2, 3 ),
 ( 0.5472222222222221655, 0.5481481481481481621, 0.5500000000000000444, 0.5518518518518518157, 0.5527777777777778123 ),
 .UNSPECIFIED. ) 
 CURVE ( )  GEOMETRIC_REPRESENTATION_ITEM ( )  RATIONAL_B_SPLINE_CURVE ( ( 0.9330127018922194093, 0.9330127018922154125, 1.000000000000000000, 0.8660254037844388186, 1.000000000000000000, 0.8660254037844388186, 1.000000000000000000, 0.9330127018922154125, 0.9330127018922194093 ) ) 
 REPRESENTATION_ITEM ( '' )  );
#28520 = CIRCLE ( 'NONE', #17788, 6.000000000000012434 ) ;
#28521 = VERTEX_POINT ( 'NONE', #19563 ) ;
#28522 = CARTESIAN_POINT ( 'NONE',  ( -5.196152422706573404, -3.000000000000002665, -132.7113248654052597 ) ) ;
#28523 = CARTESIAN_POINT ( 'NONE',  ( 0.000000000000000000, 5.499999999999991118, -177.0000000000000568 ) ) ;
#28524 = CARTESIAN_POINT ( 'NONE',  ( 107.1877832217621886, 0.7662911109078588412, -1.849990392679231599 ) ) ;
#28525 = CARTESIAN_POINT ( 'NONE',  ( 6.000000000000000888, -1.607695154586752384, -168.7306624327026157 ) ) ;
#28526 = CARTESIAN_POINT ( 'NONE',  ( 3.608439182435180470, -6.249999999999997335, -179.5580127018922383 ) ) ;
#28527 = CARTESIAN_POINT ( 'NONE',  ( 6.000000000000000888, 1.743066579297358182E-13, -76.58632486540521711 ) ) ;
#28528 = CARTESIAN_POINT ( 'NONE',  ( -4.999999999999886313, -71.00000000000002842, -5.000000000000004441 ) ) ;
#28529 = CARTESIAN_POINT ( 'NONE',  ( -4.763139720814407951, -2.750000000000016431, -127.0000000000000000 ) ) ;
#28530 = CARTESIAN_POINT ( 'NONE',  ( 116.0000000000000142, 0.000000000000000000, 0.000000000000000000 ) ) ;
#28531 = CARTESIAN_POINT ( 'NONE',  ( 3.175426480543072749, -5.500000000000105693, -110.1249999999999858 ) ) ;
#28532 = CYLINDRICAL_SURFACE ( 'NONE', #17104, 5.500000000000000000 ) ;
#28533 = CARTESIAN_POINT ( 'NONE',  ( 16.27382486540525619, -2.499999999999964473, -1.035533905932749299 ) ) ;
#28534 = ORIENTED_EDGE ( 'NONE', *, *, #7037, .F. ) ;
#28535 = CARTESIAN_POINT ( 'NONE',  ( 17.50000000000007105, 1.873492889145123019, -1.873492889145011997 ) ) ;
#28536 = CIRCLE ( 'NONE', #15346, 1.000000000000000000 ) ;
#28537 = ADVANCED_FACE ( 'NONE', ( #28898 ), #24296, .T. ) ;
#28538 = DIRECTION ( 'NONE',  ( -7.147005652999508048E-36, 5.642372883946980038E-36, 1.000000000000000000 ) ) ;
#28539 = DIRECTION ( 'NONE',  ( -7.147005652999508048E-36, 5.642372883946980038E-36, 1.000000000000000000 ) ) ;
#28540 = CARTESIAN_POINT ( 'NONE',  ( 116.5386751345946408, 1.110223024625156540E-13, 2.000000000000112799 ) ) ;
#28541 = CARTESIAN_POINT ( 'NONE',  ( 6.000000000000000888, -1.859271017917181981E-14, -145.5863248654052029 ) ) ;
#28542 = VERTEX_POINT ( 'NONE', #22778 ) ;
#28543 = CARTESIAN_POINT ( 'NONE',  ( -4.763139720814407951, -2.750000000000016431, -178.0000000000000568 ) ) ;
#28544 = CARTESIAN_POINT ( 'NONE',  ( 110.1247167782376124, -1.849990392679412565, 2.220446049250313081E-13 ) ) ;
#28545 =( NAMED_UNIT ( * ) SI_UNIT ( $, .STERADIAN. ) SOLID_ANGLE_UNIT ( ) );
#28546 = EDGE_LOOP ( 'NONE', ( #6186, #18816, #3303, #27332 ) ) ;
#28547 = CARTESIAN_POINT ( 'NONE',  ( 3.464101615137757051, -5.999999999999979572, -95.41367513459479710 ) ) ;
#28548 = EDGE_CURVE ( 'NONE', #13349, #13602, #21175, .T. ) ;
#28549 = VERTEX_POINT ( 'NONE', #8320 ) ;
#28550 = AXIS2_PLACEMENT_3D ( 'NONE', #15435, #22314, #1246 ) ;
#28551 = CARTESIAN_POINT ( 'NONE',  ( 134.8273502691896510, -5.000000000000004441, 0.000000000000000000 ) ) ;
#28552 = ORIENTED_EDGE ( 'NONE', *, *, #23526, .F. ) ;
#28553 = CARTESIAN_POINT ( 'NONE',  ( -5.412658773652739619, 3.124999999999975131, -129.8169872981078186 ) ) ;
#28554 = DIRECTION ( 'NONE',  ( -7.147005652999508048E-36, 5.642372883946980038E-36, 1.000000000000000000 ) ) ;
#28555 = CARTESIAN_POINT ( 'NONE',  ( 11.37499999999999645, 2.649519052838500421, -5.551115123125782702E-14 ) ) ;
#28556 = CARTESIAN_POINT ( 'NONE',  ( 0.000000000000000000, 0.000000000000000000, 0.000000000000000000 ) ) ;
#28557 = EDGE_LOOP ( 'NONE', ( #21854, #8332, #21439, #14084 ) ) ;
#28558 = CARTESIAN_POINT ( 'NONE',  ( 18.12500000000000355, 1.414213562373090038, 1.414213562373090038 ) ) ;
#28559 = CARTESIAN_POINT ( 'NONE',  ( 6.000000000000026645, -1.607695154586707753, -129.7306624327025872 ) ) ;
#28560 = CARTESIAN_POINT ( 'NONE',  ( 139.5000000000000284, -9.165151389911669000, -8.000000000000007105 ) ) ;
#28561 = CARTESIAN_POINT ( 'NONE',  ( 141.0788997308104058, -4.999999999999989342, 2.071067811865468400 ) ) ;
#28562 = CARTESIAN_POINT ( 'NONE',  ( 137.7113248654052029, 5.500000000000005329, 0.000000000000000000 ) ) ;
#28563 = LINE ( 'NONE', #10160, #8994 ) ;
#28564 =( NAMED_UNIT ( * ) SI_UNIT ( $, .STERADIAN. ) SOLID_ANGLE_UNIT ( ) );
#28565 = CARTESIAN_POINT ( 'NONE',  ( 107.4374999999997868, -2.499999999999964473, 1.035533905932989551 ) ) ;
#28566 =( BOUNDED_CURVE ( )  B_SPLINE_CURVE ( 2, ( #10281, #12457, #15197, #27430, #20094, #6397, #6106, #18266, #24981 ),
 .UNSPECIFIED., .F., .T. ) 
 B_SPLINE_CURVE_WITH_KNOTS ( ( 3, 2, 2, 2, 3 ),
 ( 0.9124999999999995337, 0.9187499999999997335, 0.9250000000000000444, 0.9312500000000002442, 0.9375000000000004441 ),
 .UNSPECIFIED. ) 
 CURVE ( )  GEOMETRIC_REPRESENTATION_ITEM ( )  RATIONAL_B_SPLINE_CURVE ( ( 1.000000000000005329, 0.9238795325112812984, 1.000000000000000000, 0.9238795325112867385, 1.000000000000000000, 0.9238795325112867385, 1.000000000000000000, 0.9238795325112812984, 1.000000000000005329 ) ) 
 REPRESENTATION_ITEM ( '' )  );
#28567 = CARTESIAN_POINT ( 'NONE',  ( -4.763139720814407951, 2.749999999999946709, -137.7500000000000284 ) ) ;
#28568 = AXIS2_PLACEMENT_3D ( 'NONE', #17386, #3209, #22437 ) ;
#28569 = CARTESIAN_POINT ( 'NONE',  ( -4.999999999999990230, -55.00000000000002132, 4.000000000000003553 ) ) ;
#28570 = ORIENTED_EDGE ( 'NONE', *, *, #22214, .F. ) ;
#28571 = ADVANCED_FACE ( 'NONE', ( #10973 ), #29521, .F. ) ;
#28572 = CARTESIAN_POINT ( 'NONE',  ( 107.7886751345947403, -1.999999999999835243, 1.110223024625156540E-13 ) ) ;
#28573 = CYLINDRICAL_SURFACE ( 'NONE', #8520, 6.000000000000000888 ) ;
#28574 = CARTESIAN_POINT ( 'NONE',  ( 5.196152422706629359, 3.000000000000002665, -79.46132486540524553 ) ) ;
#28575 = STYLED_ITEM ( 'NONE', ( #15824 ), #13685 ) ;
#28576 = CARTESIAN_POINT ( 'NONE',  ( 0.000000000000000000, 5.999999999999977796, -152.7113248654052313 ) ) ;
#28577 = ORIENTED_EDGE ( 'NONE', *, *, #2646, .T. ) ;
#28578 = CARTESIAN_POINT ( 'NONE',  ( 119.4372167782374419, 0.7662911109078888172, -1.849990392679291551 ) ) ;
#28579 = CARTESIAN_POINT ( 'NONE',  ( 136.4062500000000284, 6.000000000000005329, -2.485281374238556218 ) ) ;
#28580 = CARTESIAN_POINT ( 'NONE',  ( 3.608439182435180470, 6.249999999999982236, -94.19198729810779014 ) ) ;
#28581 = CARTESIAN_POINT ( 'NONE',  ( -5.999999999999963585, 1.780251999655701777E-13, -78.83632486540523132 ) ) ;
#28582 = EDGE_CURVE ( 'NONE', #14144, #4583, #20321, .T. ) ;
#28583 = CARTESIAN_POINT ( 'NONE',  ( 161.4226497308104058, 5.000000000000004441, 0.000000000000000000 ) ) ;
#28584 = CARTESIAN_POINT ( 'NONE',  ( 118.3124999999997726, -1.035533905932598975, 2.500000000000205169 ) ) ;
#28585 = CARTESIAN_POINT ( 'NONE',  ( 3.175426480543072749, 5.499999999999865885, -129.1250000000000284 ) ) ;
#28586 = ORIENTED_EDGE ( 'NONE', *, *, #21254, .F. ) ;
#28587 = CARTESIAN_POINT ( 'NONE',  ( 115.3363248654051461, -1.414213562372979016, -1.414213562372812483 ) ) ;
#28588 = CARTESIAN_POINT ( 'NONE',  ( 3.175426480543072749, -5.500000000000105693, -59.12499999999999289 ) ) ;
#28589 = FACE_OUTER_BOUND ( 'NONE', #5543, .T. ) ;
#28590 = LINE ( 'NONE', #16534, #17163 ) ;
#28591 = CARTESIAN_POINT ( 'NONE',  ( -3.608439182435052128, -6.250000000000110134, -85.30801270189222407 ) ) ;
#28592 = CARTESIAN_POINT ( 'NONE',  ( 6.000000000000000888, -1.859271017917181981E-14, -169.5863248654052029 ) ) ;
#28593 = CARTESIAN_POINT ( 'NONE',  ( 104.9997167782376692, -1.308140751793585022, 1.308140751793640533 ) ) ;
#28594 = CARTESIAN_POINT ( 'NONE',  ( 116.0000000000000142, 0.000000000000000000, 0.000000000000000000 ) ) ;
#28595 = CARTESIAN_POINT ( 'NONE',  ( 113.9377832217623450, -1.849990392679441875, -0.7662911109076485650 ) ) ;
#28596 = CARTESIAN_POINT ( 'NONE',  ( -4.763139720814407951, 2.749999999999946709, -143.7500000000000568 ) ) ;
#28597 = CARTESIAN_POINT ( 'NONE',  ( 6.000000000000000888, -3.330669073875464691E-16, -7.560779664488942560E-35 ) ) ;
#28598 = CARTESIAN_POINT ( 'NONE',  ( 2.775557561562891351E-14, -6.250000000000061284, -155.6830127018922099 ) ) ;
#28599 = CARTESIAN_POINT ( 'NONE',  ( -5.196152422706601826, 2.999999999999975131, -158.4613248654052029 ) ) ;
#28600 = CARTESIAN_POINT ( 'NONE',  ( 3.464101615137852974, 5.999999999999884537, -51.41367513459485394 ) ) ;
#28601 = ADVANCED_FACE ( 'NONE', ( #18186 ), #1872, .T. ) ;
#28602 = CARTESIAN_POINT ( 'NONE',  ( -6.350852961085760029, -1.281975124255709124E-13, -71.62500000000005684 ) ) ;
#28603 = CARTESIAN_POINT ( 'NONE',  ( 3.175426480543072749, 5.499999999999865885, -64.62500000000001421 ) ) ;
#28604 = CARTESIAN_POINT ( 'NONE',  ( 142.7023502691896510, 0.000000000000000000, -5.000000000000004441 ) ) ;
#28605 = AXIS2_PLACEMENT_3D ( 'NONE', #24647, #22522, #1455 ) ;
#28606 = CARTESIAN_POINT ( 'NONE',  ( 151.4062500000000284, 6.000000000000005329, -2.485281374238556218 ) ) ;
#28607 = CARTESIAN_POINT ( 'NONE',  ( 0.000000000000000000, 0.000000000000000000, 0.000000000000000000 ) ) ;
#28608 = CARTESIAN_POINT ( 'NONE',  ( 18.00000000000012790, 2.000000000000112799, 0.000000000000000000 ) ) ;
#28609 = MECHANICAL_DESIGN_GEOMETRIC_PRESENTATION_REPRESENTATION (  '', ( #10514 ), #19333 ) ;
#28610 =( BOUNDED_CURVE ( )  B_SPLINE_CURVE ( 2, ( #26116, #23828, #14627, #5507, #14915, #2764, #3202, #12192, #21533 ),
 .UNSPECIFIED., .F., .F. ) 
 B_SPLINE_CURVE_WITH_KNOTS ( ( 3, 2, 2, 2, 3 ),
 ( 0.3281250000000000000, 0.3359375000000000000, 0.3437500000000000000, 0.3515625000000000000, 0.3593750000000000000 ),
 .UNSPECIFIED. ) 
 CURVE ( )  GEOMETRIC_REPRESENTATION_ITEM ( )  RATIONAL_B_SPLINE_CURVE ( ( 1.000000000000000000, 0.9238795325112867385, 1.000000000000000000, 0.9238795325112867385, 1.000000000000000000, 0.9238795325112867385, 1.000000000000000000, 0.9238795325112867385, 1.000000000000000000 ) ) 
 REPRESENTATION_ITEM ( '' )  );
#28611 = CARTESIAN_POINT ( 'NONE',  ( 3.464101615137757051, -5.999999999999979572, -88.83632486540521711 ) ) ;
#28612 = EDGE_CURVE ( 'NONE', #10004, #22416, #18731, .T. ) ;
#28613 = ORIENTED_EDGE ( 'NONE', *, *, #7508, .F. ) ;
#28614 = CARTESIAN_POINT ( 'NONE',  ( 151.3125000000000568, 4.242640687119298093, -4.242640687119298093 ) ) ;
#28615 = CARTESIAN_POINT ( 'NONE',  ( 119.2261751345946266, 2.000000000000001776, -0.8284271247459350507 ) ) ;
#28616 = CARTESIAN_POINT ( 'NONE',  ( 0.000000000000000000, 0.000000000000000000, 0.000000000000000000 ) ) ;
#28617 = CARTESIAN_POINT ( 'NONE',  ( -3.608439182435052128, -6.250000000000110134, -46.94198729810782567 ) ) ;
#28618 = CARTESIAN_POINT ( 'NONE',  ( 22.12500000000006040, 1.414213562373145550, 1.414213562373201061 ) ) ;
#28619 = VERTEX_POINT ( 'NONE', #10822 ) ;
#28620 = CARTESIAN_POINT ( 'NONE',  ( -2.775557561562891351E-14, -5.500000000000115463, -78.74999999999998579 ) ) ;
#28621 = CARTESIAN_POINT ( 'NONE',  ( -3.608439182435052128, -6.250000000000110134, -101.8080127018922241 ) ) ;
#28622 = ORIENTED_EDGE ( 'NONE', *, *, #23310, .T. ) ;
#28623 = LINE ( 'NONE', #19732, #11370 ) ;
#28624 = DIRECTION ( 'NONE',  ( 1.000000000000000000, 0.000000000000000000, 0.000000000000000000 ) ) ;
#28625 = DIRECTION ( 'NONE',  ( -0.000000000000000000, -0.000000000000000000, -1.000000000000000000 ) ) ;
#28626 = CARTESIAN_POINT ( 'NONE',  ( 134.5000410784367944, -6.964617708436220411, 8.000000000000007105 ) ) ;
#28627 = CARTESIAN_POINT ( 'NONE',  ( 4.763139720814407951, 2.750000000000002665, -162.2500000000000000 ) ) ;
#28628 = CARTESIAN_POINT ( 'NONE',  ( 6.000000000000000888, -1.859271017917181981E-14, -80.16367513459481131 ) ) ;
#28629 = CARTESIAN_POINT ( 'NONE',  ( -4.763139720814407951, -2.750000000000016431, -157.0000000000000284 ) ) ;
#28630 = CARTESIAN_POINT ( 'NONE',  ( 134.9999999999999716, 4.954201571808754423, 2.980857315194011203 ) ) ;
#28631 = CARTESIAN_POINT ( 'NONE',  ( 149.2425748654052029, -2.278174593052245012, -5.499999999999781508 ) ) ;
#28632 = EDGE_CURVE ( 'NONE', #23931, #18612, #11890, .T. ) ;
#28633 = CARTESIAN_POINT ( 'NONE',  ( -6.350852961085760029, -1.281975124255709124E-13, -91.12500000000001421 ) ) ;
#28634 = CARTESIAN_POINT ( 'NONE',  ( 3.464101615137852974, 5.999999999999884537, -125.8363248654051887 ) ) ;
#28635 = CARTESIAN_POINT ( 'NONE',  ( -5.999999999999971578, 1.607695154586715303, -59.40331216351300014 ) ) ;
#28636 = ADVANCED_FACE ( 'NONE', ( #3705 ), #1249, .F. ) ;
#28637 = CARTESIAN_POINT ( 'NONE',  ( 3.175426480543072749, 5.499999999999865885, -93.12500000000002842 ) ) ;
#28638 = FACE_OUTER_BOUND ( 'NONE', #6312, .T. ) ;
#28639 = CARTESIAN_POINT ( 'NONE',  ( 158.1711002691896510, 4.999999999999989342, 2.071067811865468400 ) ) ;
#28640 = CARTESIAN_POINT ( 'NONE',  ( 6.000000000000000888, -1.859271017917181981E-14, -72.08632486540521711 ) ) ;
#28641 = CARTESIAN_POINT ( 'NONE',  ( 109.2738248654049045, -1.999999999999941602, -0.8284271247458748766 ) ) ;
#28642 = CARTESIAN_POINT ( 'NONE',  ( 23.62500000000000711, -1.414213562372923505, -1.414213562373145550 ) ) ;
#28643 = CARTESIAN_POINT ( 'NONE',  ( 111.1249999999999289, 1.767766952966320915, 1.767766952966431937 ) ) ;
#28644 = DIRECTION ( 'NONE',  ( 1.000000000000000000, -0.000000000000000000, -0.000000000000000000 ) ) ;
#28645 = CARTESIAN_POINT ( 'NONE',  ( 5.196152422706629359, 3.000000000000002665, -72.53867513459482552 ) ) ;
#28646 = DIRECTION ( 'NONE',  ( -0.2768592823360735977, 0.4367774878841475528, -0.8559055811606602893 ) ) ;
#28647 =( BOUNDED_CURVE ( )  B_SPLINE_CURVE ( 2, ( #23736, #514, #24580, #5833, #21134, #29030, #71, #28165, #7135 ),
 .UNSPECIFIED., .F., .T. ) 
 B_SPLINE_CURVE_WITH_KNOTS ( ( 3, 2, 2, 2, 3 ),
 ( 0.7249999999999999778, 0.7259259259259258634, 0.7277777777777778567, 0.7296296296296296280, 0.7305555555555556246 ),
 .UNSPECIFIED. ) 
 CURVE ( )  GEOMETRIC_REPRESENTATION_ITEM ( )  RATIONAL_B_SPLINE_CURVE ( ( 0.9330127018922194093, 0.9330127018922194093, 1.000000000000000000, 0.8660254037844388186, 1.000000000000000000, 0.8660254037844388186, 1.000000000000000000, 0.9330127018922114157, 0.9330127018922194093 ) ) 
 REPRESENTATION_ITEM ( '' )  );
#28648 = ORIENTED_EDGE ( 'NONE', *, *, #28948, .F. ) ;
#28649 = CARTESIAN_POINT ( 'NONE',  ( -0.05795336459416459973, -14.59255675236215666, -8.264483820923475221 ) ) ;
#28650 = CARTESIAN_POINT ( 'NONE',  ( 120.3752832217621460, 1.849990392679579099, 0.000000000000000000 ) ) ;
#28651 = ORIENTED_EDGE ( 'NONE', *, *, #13614, .T. ) ;
#28652 =( BOUNDED_CURVE ( )  B_SPLINE_CURVE ( 2, ( #20799, #16518, #18355, #21245, #18962, #25689, #11755, #16666, #18806 ),
 .UNSPECIFIED., .F., .T. ) 
 B_SPLINE_CURVE_WITH_KNOTS ( ( 3, 2, 2, 2, 3 ),
 ( 0.7805555555555555580, 0.7814814814814814437, 0.7833333333333333259, 0.7851851851851852082, 0.7861111111111110938 ),
 .UNSPECIFIED. ) 
 CURVE ( )  GEOMETRIC_REPRESENTATION_ITEM ( )  RATIONAL_B_SPLINE_CURVE ( ( 0.9330127018922194093, 0.9330127018922194093, 1.000000000000000000, 0.8660254037844388186, 1.000000000000000000, 0.8660254037844388186, 1.000000000000000000, 0.9330127018922194093, 0.9330127018922194093 ) ) 
 REPRESENTATION_ITEM ( '' )  );
#28653 = ORIENTED_EDGE ( 'NONE', *, *, #20777, .T. ) ;
#28654 = CARTESIAN_POINT ( 'NONE',  ( -3.175426480542816510, -5.500000000000057732, -105.8750000000000284 ) ) ;
#28655 = CARTESIAN_POINT ( 'NONE',  ( 18.31250000000011724, 2.649519052838478661, -1.097466725451679892 ) ) ;
#28656 = CARTESIAN_POINT ( 'NONE',  ( 0.000000000000000000, 5.499999999999991118, -150.0000000000000284 ) ) ;
#28657 = CARTESIAN_POINT ( 'NONE',  ( 3.608439182435180470, 6.249999999999982236, -125.0580127018921957 ) ) ;
#28658 = EDGE_LOOP ( 'NONE', ( #14197, #23817, #13273, #15622 ) ) ;
#28659 = CARTESIAN_POINT ( 'NONE',  ( 2.775557561562891351E-14, 6.250000000000033751, -161.5669872981078186 ) ) ;
#28660 = CARTESIAN_POINT ( 'NONE',  ( 106.9999999999999716, 2.500000000000030198, 0.000000000000000000 ) ) ;
#28661 = CARTESIAN_POINT ( 'NONE',  ( 131.6101497308104342, 3.535533905932725318, 3.535533905932725318 ) ) ;
#28662 = AXIS2_PLACEMENT_3D ( 'NONE', #12635, #15236, #22134 ) ;
#28663 = CARTESIAN_POINT ( 'NONE',  ( 2.775557561562891351E-14, -6.250000000000061284, -56.68301270189224539 ) ) ;
#28664 = ORIENTED_EDGE ( 'NONE', *, *, #424, .F. ) ;
#28665 = CARTESIAN_POINT ( 'NONE',  ( 0.000000000000000000, -5.999999999999991118, -132.4613248654051745 ) ) ;
#28666 = CARTESIAN_POINT ( 'NONE',  ( 6.000000000000000888, -3.330669073875464691E-16, -7.560779664488942560E-35 ) ) ;
#28667 = CARTESIAN_POINT ( 'NONE',  ( 0.000000000000000000, 5.499999999999991118, -178.5000000000000000 ) ) ;
#28668 = CARTESIAN_POINT ( 'NONE',  ( 119.3124999999998437, -1.035533905932689347, 2.500000000000265121 ) ) ;
#28669 = CARTESIAN_POINT ( 'NONE',  ( -5.196152422706573404, -3.000000000000002665, -169.2886751345948255 ) ) ;
#28670 = CARTESIAN_POINT ( 'NONE',  ( -3.608439182435115633, 6.249999999999965361, -178.8080127018922667 ) ) ;
#28671 = CARTESIAN_POINT ( 'NONE',  ( 113.7886751345947687, -1.999999999999918510, 0.000000000000000000 ) ) ;
#28672 = DIRECTION ( 'NONE',  ( 0.000000000000000000, 0.000000000000000000, 1.000000000000000000 ) ) ;
#28673 = ADVANCED_FACE ( 'NONE', ( #4015 ), #2616, .F. ) ;
#28674 = CARTESIAN_POINT ( 'NONE',  ( -5.999999999999983125, 1.067854986875956076E-15, -44.99152654425658682 ) ) ;
#28675 = EDGE_CURVE ( 'NONE', #9700, #17985, #15006, .T. ) ;
#28676 = CARTESIAN_POINT ( 'NONE',  ( 3.175426480543072749, -5.500000000000105693, -111.6249999999999858 ) ) ;
#28677 = CARTESIAN_POINT ( 'NONE',  ( -3.464101615137725076, 5.999999999999979572, -142.6636751345948255 ) ) ;
#28678 = MECHANICAL_DESIGN_GEOMETRIC_PRESENTATION_REPRESENTATION (  '', ( #6624 ), #8596 ) ;
#28679 = CARTESIAN_POINT ( 'NONE',  ( -5.196152422706601826, 2.999999999999975131, -88.53867513459483973 ) ) ;
#28680 = ORIENTED_EDGE ( 'NONE', *, *, #195, .T. ) ;
#28681 = CARTESIAN_POINT ( 'NONE',  ( 18.00000000000007105, -1.873492889144845464, 1.873492889144900975 ) ) ;
#28682 = CARTESIAN_POINT ( 'NONE',  ( 0.7669223171414760731, -15.58766199952930620, 7.954545454545462135 ) ) ;
#28683 = CARTESIAN_POINT ( 'NONE',  ( -3.464101615137757051, -5.999999999999979572, -56.08632486540518158 ) ) ;
#28684 = ORIENTED_EDGE ( 'NONE', *, *, #17804, .F. ) ;
#28685 = CARTESIAN_POINT ( 'NONE',  ( 111.4136751345947260, 1.414213562373145550, 1.414213562373034527 ) ) ;
#28686 = CARTESIAN_POINT ( 'NONE',  ( 0.000000000000000000, 5.499999999999991118, -180.0000000000000568 ) ) ;
#28687 = CARTESIAN_POINT ( 'NONE',  ( 109.6872167782374561, 1.849990392679562001, 0.7662911109080090544 ) ) ;
#28688 = AXIS2_PLACEMENT_3D ( 'NONE', #29714, #9144, #18385 ) ;
#28689 = CARTESIAN_POINT ( 'NONE',  ( 136.0000000000000284, 0.000000000000000000, 0.000000000000000000 ) ) ;
#28690 = VERTEX_POINT ( 'NONE', #16205 ) ;
#28691 = CARTESIAN_POINT ( 'NONE',  ( -1.110223024625164676E-16, 2.000000000000012879, 2.021286199229734960E-15 ) ) ;
#28692 = ORIENTED_EDGE ( 'NONE', *, *, #28632, .T. ) ;
#28693 = ORIENTED_EDGE ( 'NONE', *, *, #22809, .T. ) ;
#28694 = CARTESIAN_POINT ( 'NONE',  ( 6.000000000000000888, 1.743066579297358182E-13, -85.58632486540523132 ) ) ;
#28695 = CARTESIAN_POINT ( 'NONE',  ( 160.5000000000000284, 6.000000000000005329, 0.000000000000000000 ) ) ;
#28696 = ORIENTED_EDGE ( 'NONE', *, *, #19432, .F. ) ;
#28697 = AXIS2_PLACEMENT_3D ( 'NONE', #2411, #23473, #21162 ) ;
#28698 = CARTESIAN_POINT ( 'NONE',  ( -5.412658773652684552, -3.125000000000099920, -134.0669872981078470 ) ) ;
#28699 = CYLINDRICAL_SURFACE ( 'NONE', #9830, 5.500000000000000000 ) ;
#28700 = CARTESIAN_POINT ( 'NONE',  ( 0.000000000000000000, 5.999999999999977796, -130.7886751345947971 ) ) ;
#28701 = EDGE_CURVE ( 'NONE', #29595, #12702, #17259, .T. ) ;
#28702 = CARTESIAN_POINT ( 'NONE',  ( 144.3824251345948255, 5.500000000000012434, 2.278174593052012309 ) ) ;
#28703 = ORIENTED_EDGE ( 'NONE', *, *, #2366, .F. ) ;
#28704 = CARTESIAN_POINT ( 'NONE',  ( 19.56250000000009948, -1.999999999999911626, -0.8284271247461753029 ) ) ;
#28705 = CARTESIAN_POINT ( 'NONE',  ( -15.49999999999999289, -25.00000000000007816, 7.500000000000007105 ) ) ;
#28706 = LINE ( 'NONE', #7528, #11802 ) ;
#28707 = DIRECTION ( 'NONE',  ( 0.000000000000000000, -2.081668171172247091E-17, 1.000000000000000000 ) ) ;
#28708 = CARTESIAN_POINT ( 'NONE',  ( 138.2663997308104342, -4.999999999999989342, -2.071067811865468400 ) ) ;
#28709 = LINE ( 'NONE', #10009, #3476 ) ;
#28710 = CARTESIAN_POINT ( 'NONE',  ( 15.47617513459492500, 1.035533905932809473, 2.499999999999844569 ) ) ;
#28711 = CARTESIAN_POINT ( 'NONE',  ( 0.000000000000000000, 0.000000000000000000, 0.000000000000000000 ) ) ;
#28712 = CARTESIAN_POINT ( 'NONE',  ( 108.9613248654050892, 1.110223024625156540E-13, 2.000000000000001776 ) ) ;
#28713 = CARTESIAN_POINT ( 'NONE',  ( 107.1249999999998437, 1.767766952966265404, 1.767766952966320915 ) ) ;
#28714 = CARTESIAN_POINT ( 'NONE',  ( -5.999999999999963585, 8.134310703387671600E-14, -115.4136751345948397 ) ) ;
#28715 = EDGE_CURVE ( 'NONE', #15499, #22218, #21085, .T. ) ;
#28716 = CARTESIAN_POINT ( 'NONE',  ( 3.175426480543072749, -5.500000000000105693, -135.6250000000000000 ) ) ;
#28717 = CYLINDRICAL_SURFACE ( 'NONE', #18621, 6.000000000000000888 ) ;
#28718 = ORIENTED_EDGE ( 'NONE', *, *, #8908, .F. ) ;
#28719 = CARTESIAN_POINT ( 'NONE',  ( 108.2886751345946834, 2.000000000000057288, 2.220446049250313081E-13 ) ) ;
#28720 = CARTESIAN_POINT ( 'NONE',  ( 6.000000000000000888, 1.607695154586715303, -88.51933756729746960 ) ) ;
#28721 = LINE ( 'NONE', #26871, #649 ) ;
#28722 = CARTESIAN_POINT ( 'NONE',  ( -5.196152422706573404, -3.000000000000002665, -164.2113248654052313 ) ) ;
#28723 = ORIENTED_EDGE ( 'NONE', *, *, #20751, .F. ) ;
#28724 = CARTESIAN_POINT ( 'NONE',  ( 116.0622167782373566, -1.849990392679381701, 0.7662911109079489913 ) ) ;
#28725 = CARTESIAN_POINT ( 'NONE',  ( 135.6562500000000284, -6.000000000000005329, 2.485281374238556218 ) ) ;
#28726 = CARTESIAN_POINT ( 'NONE',  ( -3.608439182435115633, 6.249999999999965361, -92.44198729810784698 ) ) ;
#28727 = CARTESIAN_POINT ( 'NONE',  ( -6.000000000000007105, -1.607695154586655129, -78.76933756729745539 ) ) ;
#28728 = MECHANICAL_DESIGN_GEOMETRIC_PRESENTATION_REPRESENTATION (  '', ( #8651 ), #868 ) ;
#28729 = CARTESIAN_POINT ( 'NONE',  ( 20.64882486540534501, 2.500000000000084821, -1.035533905932869425 ) ) ;
#28730 = CARTESIAN_POINT ( 'NONE',  ( 117.3124999999997300, -1.035533905932689347, 2.500000000000265121 ) ) ;
#28731 = CARTESIAN_POINT ( 'NONE',  ( 5.000000000000018652, 6.000000000000081712, 1.170861610602048163E-13 ) ) ;
#28732 = AXIS2_PLACEMENT_3D ( 'NONE', #18499, #27821, #25 ) ;
#28733 = CARTESIAN_POINT ( 'NONE',  ( 3.175426480543072749, 5.499999999999865885, -126.1250000000000426 ) ) ;
#28734 = EDGE_CURVE ( 'NONE', #9152, #2251, #12078, .T. ) ;
#28735 = ORIENTED_EDGE ( 'NONE', *, *, #16971, .T. ) ;
#28736 = EDGE_CURVE ( 'NONE', #29376, #23842, #6557, .T. ) ;
#28737 = CARTESIAN_POINT ( 'NONE',  ( 4.763139720814407951, 2.750000000000002665, -60.25000000000002842 ) ) ;
#28738 = DIRECTION ( 'NONE',  ( 1.000000000000000000, -5.551115123125773458E-17, -1.260129944081490338E-35 ) ) ;
#28739 = CARTESIAN_POINT ( 'NONE',  ( 6.000000000000000888, -3.330669073875464691E-16, -7.560779664488942560E-35 ) ) ;
#28740 = CARTESIAN_POINT ( 'NONE',  ( 5.960408494996782380, 9.245657484109267799, -25.79492440527508990 ) ) ;
#28741 = CARTESIAN_POINT ( 'NONE',  ( -3.608439182435115633, 6.249999999999965361, -81.30801270189226670 ) ) ;
#28742 =( BOUNDED_CURVE ( )  B_SPLINE_CURVE ( 2, ( #290, #26095, #20750, #27779, #11710, #6754, #23213, #9370, #30249 ),
 .UNSPECIFIED., .F., .T. ) 
 B_SPLINE_CURVE_WITH_KNOTS ( ( 3, 2, 2, 2, 3 ),
 ( 0.1638888888888888895, 0.1648148148148148029, 0.1666666666666666574, 0.1685185185185185119, 0.1694444444444444253 ),
 .UNSPECIFIED. ) 
 CURVE ( )  GEOMETRIC_REPRESENTATION_ITEM ( )  RATIONAL_B_SPLINE_CURVE ( ( 0.9330127018922194093, 0.9330127018922194093, 1.000000000000000000, 0.8660254037844388186, 1.000000000000000000, 0.8660254037844388186, 1.000000000000000000, 0.9330127018922205195, 0.9330127018922196314 ) ) 
 REPRESENTATION_ITEM ( '' )  );
#28743 = CARTESIAN_POINT ( 'NONE',  ( 0.000000000000000000, -5.999999999999991118, -100.9613248654052171 ) ) ;
#28744 = CARTESIAN_POINT ( 'NONE',  ( -3.464101615137725076, 5.999999999999979572, -169.0863248654052029 ) ) ;
#28745 =( GEOMETRIC_REPRESENTATION_CONTEXT ( 3 ) GLOBAL_UNCERTAINTY_ASSIGNED_CONTEXT ( ( #2873 ) ) GLOBAL_UNIT_ASSIGNED_CONTEXT ( ( #8792, #18034, #1864 ) ) REPRESENTATION_CONTEXT ( 'NONE', 'WORKASPACE' ) );
#28746 = MECHANICAL_DESIGN_GEOMETRIC_PRESENTATION_REPRESENTATION (  '', ( #24836 ), #2299 ) ;
#28747 = CARTESIAN_POINT ( 'NONE',  ( 0.000000000000000000, 0.000000000000000000, 0.000000000000000000 ) ) ;
#28748 = SURFACE_SIDE_STYLE ('',( #21721 ) ) ;
#28749 = CARTESIAN_POINT ( 'NONE',  ( 114.6252832217623450, 0.000000000000000000, 1.849990392679523588 ) ) ;
#28750 = ADVANCED_FACE ( 'NONE', ( #30285 ), #7089, .T. ) ;
#28751 = CARTESIAN_POINT ( 'NONE',  ( 3.175426480543072749, 5.499999999999865885, -139.6250000000000000 ) ) ;
#28752 = CARTESIAN_POINT ( 'NONE',  ( 139.7122326009735218, -8.976976166826791115, 7.966489656652901985 ) ) ;
#28753 = CARTESIAN_POINT ( 'NONE',  ( 5.412658773652712085, -3.125000000000086153, -155.4330127018922383 ) ) ;
#28754 = CARTESIAN_POINT ( 'NONE',  ( -5.196152422706601826, 2.999999999999975131, -101.4613248654052171 ) ) ;
#28755 = CARTESIAN_POINT ( 'NONE',  ( -3.464101615137725076, 5.999999999999979572, -67.08632486540523132 ) ) ;
#28756 = CARTESIAN_POINT ( 'NONE',  ( -4.763139720814407951, 2.749999999999946709, -73.25000000000004263 ) ) ;
#28757 = CARTESIAN_POINT ( 'NONE',  ( 3.175426480543072749, 5.499999999999865885, -54.12500000000003553 ) ) ;
#28758 = FILL_AREA_STYLE ('',( #21732 ) ) ;
#28759 = CARTESIAN_POINT ( 'NONE',  ( 145.8898502691896510, 3.535533905932725318, -3.535533905932725318 ) ) ;
#28760 = CARTESIAN_POINT ( 'NONE',  ( 149.6250000000000284, 0.000000000000000000, -6.000000000000005329 ) ) ;
#28761 = CARTESIAN_POINT ( 'NONE',  ( 6.000000000000000888, 1.607695154586715303, -127.5193375672974412 ) ) ;
#28762 = CARTESIAN_POINT ( 'NONE',  ( 17.18750000000013145, 0.8284271247463557142, 1.999999999999971800 ) ) ;
#28763 = FACE_OUTER_BOUND ( 'NONE', #4302, .T. ) ;
#28764 = DIRECTION ( 'NONE',  ( 1.000000000000000000, 0.000000000000000000, 0.000000000000000000 ) ) ;
#28765 = VERTEX_POINT ( 'NONE', #9243 ) ;
#28766 = CARTESIAN_POINT ( 'NONE',  ( 144.3750000000000284, 0.000000000000000000, 6.000000000000005329 ) ) ;
#28767 = DIRECTION ( 'NONE',  ( 1.000000000000000000, -5.551115123125774074E-17, 0.000000000000000000 ) ) ;
#28768 = DIRECTION ( 'NONE',  ( 0.000000000000000000, -0.7999999999999996003, -0.6000000000000006439 ) ) ;
#28769 = CARTESIAN_POINT ( 'NONE',  ( 4.763139720814407951, -2.749999999999988454, -180.5000000000000000 ) ) ;
#28770 = CARTESIAN_POINT ( 'NONE',  ( 21.75000000000007461, 2.220446049250313081E-13, -2.000000000000001776 ) ) ;
#28771 = VERTEX_POINT ( 'NONE', #20629 ) ;
#28772 = ADVANCED_FACE ( 'NONE', ( #18638 ), #29973, .T. ) ;
#28773 = CARTESIAN_POINT ( 'NONE',  ( 3.175426480543072749, -5.500000000000105693, -83.12500000000004263 ) ) ;
#28774 = CARTESIAN_POINT ( 'NONE',  ( 3.608439182435180470, 6.249999999999982236, -99.55801270189222407 ) ) ;
#28775 = AXIS2_PLACEMENT_3D ( 'NONE', #12450, #7641, #14170 ) ;
#28776 = DIRECTION ( 'NONE',  ( 1.000000000000000000, -0.000000000000000000, -0.000000000000000000 ) ) ;
#28777 = CARTESIAN_POINT ( 'NONE',  ( -5.999999999999963585, -1.487416814333745711E-14, -96.83632486540520290 ) ) ;
#28778 = CARTESIAN_POINT ( 'NONE',  ( -5.999999999999963585, 1.780251999655701777E-13, -100.4136751345948255 ) ) ;
#28779 = CARTESIAN_POINT ( 'NONE',  ( 111.3988248654049613, -0.8284271247461153509, -1.999999999999791278 ) ) ;
#28780 = CARTESIAN_POINT ( 'NONE',  ( 24.99999999999999289, 1.110223024625156540E-13, -2.220446049250313081E-13 ) ) ;
#28781 = VECTOR ( 'NONE', #9569, 1000.000000000000000 ) ;
#28782 = EDGE_CURVE ( 'NONE', #19300, #605, #27658, .T. ) ;
#28783 =( NAMED_UNIT ( * ) SI_UNIT ( $, .STERADIAN. ) SOLID_ANGLE_UNIT ( ) );
#28784 = EDGE_CURVE ( 'NONE', #22616, #11342, #2481, .T. ) ;
#28785 = CARTESIAN_POINT ( 'NONE',  ( -2.775557561562891351E-14, -5.500000000000115463, -164.2500000000000000 ) ) ;
#28786 = CARTESIAN_POINT ( 'NONE',  ( 6.000000000000000888, -1.859271017917181981E-14, -58.58632486540521001 ) ) ;
#28787 = CARTESIAN_POINT ( 'NONE',  ( 0.000000000000000000, 5.499999999999991118, -145.5000000000000284 ) ) ;
#28788 = FACE_OUTER_BOUND ( 'NONE', #22074, .T. ) ;
#28789 = CARTESIAN_POINT ( 'NONE',  ( 6.000000000000052403, -1.607695154586662678, -103.6533121635130072 ) ) ;
#28790 =( BOUNDED_CURVE ( )  B_SPLINE_CURVE ( 2, ( #15741, #8795, #25050, #22771, #1715, #27953, #4917, #174, #19231 ),
 .UNSPECIFIED., .F., .F. ) 
 B_SPLINE_CURVE_WITH_KNOTS ( ( 3, 2, 2, 2, 3 ),
 ( 0.7352941176470588758, 0.7426470588235294379, 0.7500000000000000000, 0.7573529411764705621, 0.7647058823529411242 ),
 .UNSPECIFIED. ) 
 CURVE ( )  GEOMETRIC_REPRESENTATION_ITEM ( )  RATIONAL_B_SPLINE_CURVE ( ( 1.000000000000000000, 0.9238795325112867385, 1.000000000000000000, 0.9238795325112867385, 1.000000000000000000, 0.9238795325112867385, 1.000000000000000000, 0.9238795325112867385, 1.000000000000000000 ) ) 
 REPRESENTATION_ITEM ( '' )  );
#28791 = CARTESIAN_POINT ( 'NONE',  ( -3.175426480542816066, -5.500000000000057732, -92.37500000000002842 ) ) ;
#28792 = CARTESIAN_POINT ( 'NONE',  ( 145.2261751345948539, -3.889087296526011706, -3.889087296526011706 ) ) ;
#28793 = CARTESIAN_POINT ( 'NONE',  ( 4.763139720814407951, -2.749999999999988454, -80.00000000000001421 ) ) ;
#28794 = FACE_OUTER_BOUND ( 'NONE', #14477, .T. ) ;
#28795 = DIRECTION ( 'NONE',  ( 1.000000000000000000, -5.551115123125773458E-17, -1.260129944081490338E-35 ) ) ;
#28796 = CARTESIAN_POINT ( 'NONE',  ( 25.00000000000013500, 2.000000000000279332, -5.551115123125782702E-14 ) ) ;
#28797 = CARTESIAN_POINT ( 'NONE',  ( 111.0624999999998295, 2.500000000000055067, 1.035533905932929599 ) ) ;
#28798 = CARTESIAN_POINT ( 'NONE',  ( -4.999999999999984013, -10.50000000000000888, -8.000000000000007105 ) ) ;
#28799 = CARTESIAN_POINT ( 'NONE',  ( 0.000000000000000000, -5.999999999999991118, -73.96132486540524553 ) ) ;
#28800 = CARTESIAN_POINT ( 'NONE',  ( 20.22617513459488592, 2.500000000000205169, -1.035533905932929599 ) ) ;
#28801 = ORIENTED_EDGE ( 'NONE', *, *, #28445, .T. ) ;
#28802 = CARTESIAN_POINT ( 'NONE',  ( -5.196152422706601826, 2.999999999999975131, -178.5386751345948824 ) ) ;
#28803 = CARTESIAN_POINT ( 'NONE',  ( 0.000000000000000000, -5.999999999999991118, -79.03867513459483973 ) ) ;
#28804 = CARTESIAN_POINT ( 'NONE',  ( 119.5627832217620750, 0.7662911109078588412, 1.849990392679712103 ) ) ;
#28805 = ORIENTED_EDGE ( 'NONE', *, *, #28305, .F. ) ;
#28806 =( GEOMETRIC_REPRESENTATION_CONTEXT ( 3 ) GLOBAL_UNCERTAINTY_ASSIGNED_CONTEXT ( ( #16853 ) ) GLOBAL_UNIT_ASSIGNED_CONTEXT ( ( #16924, #7513, #28545 ) ) REPRESENTATION_CONTEXT ( 'NONE', 'WORKASPACE' ) );
#28807 = ORIENTED_EDGE ( 'NONE', *, *, #4729, .F. ) ;
#28808 = ORIENTED_EDGE ( 'NONE', *, *, #493, .T. ) ;
#28809 = EDGE_CURVE ( 'NONE', #19802, #30369, #9720, .T. ) ;
#28810 = CARTESIAN_POINT ( 'NONE',  ( -3.175426480542816510, 5.499999999999865885, -101.8750000000000000 ) ) ;
#28811 = CARTESIAN_POINT ( 'NONE',  ( 19.18750000000007461, 1.097466725451619718, -2.649519052838298805 ) ) ;
#28812 = CARTESIAN_POINT ( 'NONE',  ( 2.775557561562891351E-14, 6.250000000000033751, -123.4330127018922241 ) ) ;
#28813 = ORIENTED_EDGE ( 'NONE', *, *, #5344, .F. ) ;
#28814 = CARTESIAN_POINT ( 'NONE',  ( -5.999999999999963585, 1.780251999655701777E-13, -61.41367513459483973 ) ) ;
#28815 = CARTESIAN_POINT ( 'NONE',  ( 5.412658773652739619, 3.124999999999988898, -158.8169872981078470 ) ) ;
#28816 = CARTESIAN_POINT ( 'NONE',  ( 135.0000000000000284, -7.146604258052373204, 8.399325966929822584 ) ) ;
#28817 = AXIS2_PLACEMENT_3D ( 'NONE', #17331, #854, #26647 ) ;
#28818 = CARTESIAN_POINT ( 'NONE',  ( 131.8913997308104058, -2.071067811865468400, 4.999999999999989342 ) ) ;
#28819 = CARTESIAN_POINT ( 'NONE',  ( 5.412658773652739619, 3.124999999999988898, -56.18301270189224539 ) ) ;
#28820 = VERTEX_POINT ( 'NONE', #16804 ) ;
#28821 = EDGE_CURVE ( 'NONE', #2749, #23806, #7540, .T. ) ;
#28822 = CARTESIAN_POINT ( 'NONE',  ( -5.676437577760642839, 9.422458200488973645, -23.04620489006168782 ) ) ;
#28823 = CARTESIAN_POINT ( 'NONE',  ( -5.999999999999919176, 1.607695154586804565, -137.4033121635130215 ) ) ;
#28824 = CARTESIAN_POINT ( 'NONE',  ( -3.175426480542816510, 5.499999999999865885, -167.8750000000000568 ) ) ;
#28825 = CARTESIAN_POINT ( 'NONE',  ( 120.9999999999997300, 2.500000000000113243, 3.330669073875469621E-13 ) ) ;
#28826 = CARTESIAN_POINT ( 'NONE',  ( 5.196152422706629359, -2.999999999999988898, -112.7113248654052455 ) ) ;
#28827 = CARTESIAN_POINT ( 'NONE',  ( 5.412658773652712085, -3.125000000000086153, -165.9330127018922099 ) ) ;
#28828 = CARTESIAN_POINT ( 'NONE',  ( 0.000000000000000000, 0.000000000000000000, 0.000000000000000000 ) ) ;
#28829 = CARTESIAN_POINT ( 'NONE',  ( 24.50000000000015987, -1.999999999999835243, -5.551115123125782702E-14 ) ) ;
#28830 = CARTESIAN_POINT ( 'NONE',  ( 0.000000000000000000, 5.499999999999991118, -118.5000000000000568 ) ) ;
#28831 = CARTESIAN_POINT ( 'NONE',  ( -5.999999999999963585, 1.780251999655701777E-13, -83.91367513459482552 ) ) ;
#28832 =( BOUNDED_SURFACE ( )  B_SPLINE_SURFACE ( 3, 2, ( 
 ( #12165, #21354, #438 ),
 ( #6757, #16178, #16328 ),
 ( #150, #20907, #25482 ),
 ( #11563, #14323, #4449 ),
 ( #13874, #16473, #18918 ),
 ( #4751, #21056, #14178 ),
 ( #23215, #30251, #9220 ),
 ( #30404, #4892, #9373 ),
 ( #25945, #18764, #23515 ),
 ( #2456, #11872, #28239 ) ),
 .UNSPECIFIED., .F., .F., .T. ) 
 B_SPLINE_SURFACE_WITH_KNOTS ( ( 4, 2, 2, 2, 4 ),
 ( 3, 3 ),
 ( 0.0004283140159002545347, 0.001007014806553221432, 0.001585715597206188276, 0.002164416387859155119, 0.002743117178512121963 ),
 ( 0.000000000000000000, 1.000000000000000000 ),
 .UNSPECIFIED. ) 
 GEOMETRIC_REPRESENTATION_ITEM ( )  RATIONAL_B_SPLINE_SURFACE ( (
 ( 1.000000000000000000, 0.7071067811872737696, 1.000000000000000000),
 ( 1.000000000000000000, 0.7334468984528983437, 1.000000000000000000),
 ( 1.000000000000000000, 0.7709563466230319184, 1.000000000000000000),
 ( 1.000000000000000000, 0.8514970365135478003, 1.000000000000000000),
 ( 1.000000000000000000, 0.8914860584493291551, 1.000000000000000000),
 ( 1.000000000000000000, 0.9504033078762521569, 1.000000000000000000),
 ( 1.000000000000000000, 0.9703159229117922502, 1.000000000000000000),
 ( 1.000000000000000000, 0.9949510651229506175, 1.000000000000000000),
 ( 1.000000000000000000, 0.9999594700102402145, 1.000000000000000000),
 ( 1.000000000000000000, 1.000000000000000000, 1.000000000000000000) ) ) 
 REPRESENTATION_ITEM ( '' )  SURFACE ( )  );
#28833 = CARTESIAN_POINT ( 'NONE',  ( 4.763139720814407951, 2.750000000000002665, -114.2500000000000142 ) ) ;
#28834 =( NAMED_UNIT ( * ) SI_UNIT ( $, .STERADIAN. ) SOLID_ANGLE_UNIT ( ) );
#28835 = DIRECTION ( 'NONE',  ( 1.000000000000000000, -5.551115123125773458E-17, -1.260129944081490338E-35 ) ) ;
#28836 = CARTESIAN_POINT ( 'NONE',  ( -5.999999999999919176, 1.607695154586804565, -100.4806624327025872 ) ) ;
#28837 = ORIENTED_EDGE ( 'NONE', *, *, #4974, .T. ) ;
#28838 = CARTESIAN_POINT ( 'NONE',  ( 119.7499999999998721, 1.110223024625156540E-13, -2.499999999999946709 ) ) ;
#28839 = CARTESIAN_POINT ( 'NONE',  ( 5.196152422706629359, 3.000000000000002665, -168.5386751345947971 ) ) ;
#28840 =( BOUNDED_CURVE ( )  B_SPLINE_CURVE ( 2, ( #4955, #13291, #10348, #17279, #26739, #3401, #20009, #8020, #1570 ),
 .UNSPECIFIED., .F., .T. ) 
 B_SPLINE_CURVE_WITH_KNOTS ( ( 3, 2, 2, 2, 3 ),
 ( 0.6472222222222221433, 0.6481481481481481399, 0.6500000000000000222, 0.6518518518518519045, 0.6527777777777777901 ),
 .UNSPECIFIED. ) 
 CURVE ( )  GEOMETRIC_REPRESENTATION_ITEM ( )  RATIONAL_B_SPLINE_CURVE ( ( 0.9330127018922194093, 0.9330127018922154125, 1.000000000000000000, 0.8660254037844388186, 1.000000000000000000, 0.8660254037844388186, 1.000000000000000000, 0.9330127018922194093, 0.9330127018922194093 ) ) 
 REPRESENTATION_ITEM ( '' )  );
#28841 = CARTESIAN_POINT ( 'NONE',  ( -3.464101615137725076, 5.999999999999979572, -86.58632486540520290 ) ) ;
#28842 = ORIENTED_EDGE ( 'NONE', *, *, #16510, .F. ) ;
#28843 = CARTESIAN_POINT ( 'NONE',  ( 111.6011751345946692, -0.8284271247460852639, 2.000000000000212275 ) ) ;
#28844 = DIRECTION ( 'NONE',  ( -1.000000000000000000, 0.000000000000000000, 0.000000000000000000 ) ) ;
#28845 = CARTESIAN_POINT ( 'NONE',  ( 5.412658773652739619, 3.124999999999988898, -82.31698729810781856 ) ) ;
#28846 = SURFACE_STYLE_FILL_AREA ( #894 ) ;
#28847 = ORIENTED_EDGE ( 'NONE', *, *, #15951, .F. ) ;
#28848 = CARTESIAN_POINT ( 'NONE',  ( 0.000000000000000000, 5.999999999999977796, -144.2886751345948824 ) ) ;
#28849 = B_SPLINE_CURVE_WITH_KNOTS ( 'NONE', 1,
 ( #12416, #21614 ),
 .UNSPECIFIED., .F., .F.,
 ( 2, 2 ),
 ( 0.000000000000000000, 0.9099963204919845339 ),
 .UNSPECIFIED. ) ;
#28850 = VERTEX_POINT ( 'NONE', #26270 ) ;
#28851 = ORIENTED_EDGE ( 'NONE', *, *, #6714, .T. ) ;
#28852 = DIRECTION ( 'NONE',  ( -1.000000000000000000, -1.665334536937736783E-16, -2.220446049250315546E-16 ) ) ;
#28853 = CARTESIAN_POINT ( 'NONE',  ( 133.9836002691896510, 4.999999999999989342, -2.071067811865468400 ) ) ;
#28854 = EDGE_CURVE ( 'NONE', #28019, #13234, #26375, .T. ) ;
#28855 = EDGE_CURVE ( 'NONE', #10990, #15916, #21540, .T. ) ;
#28856 = CARTESIAN_POINT ( 'NONE',  ( 10.75000000000014921, 1.665334536937734811E-13, -2.000000000000168310 ) ) ;
#28857 = CARTESIAN_POINT ( 'NONE',  ( 2.775557561562891351E-14, 6.250000000000033751, -128.5669872981078470 ) ) ;
#28858 = CARTESIAN_POINT ( 'NONE',  ( -5.196152422706601826, 2.999999999999975131, -49.53867513459481131 ) ) ;
#28859 = CARTESIAN_POINT ( 'NONE',  ( 6.000000000000000888, 1.743066579297358182E-13, -90.66367513459483973 ) ) ;
#28860 = ORIENTED_EDGE ( 'NONE', *, *, #1575, .T. ) ;
#28861 = CARTESIAN_POINT ( 'NONE',  ( 17.37500000000011369, -1.414213562372979016, 1.414213562373034527 ) ) ;
#28862 = CARTESIAN_POINT ( 'NONE',  ( -5.196152422706573404, -3.000000000000002665, -139.2886751345948539 ) ) ;
#28863 = DIRECTION ( 'NONE',  ( 1.000000000000000000, -5.551115123125773458E-17, -1.260129944081490338E-35 ) ) ;
#28864 = CARTESIAN_POINT ( 'NONE',  ( 140.8913997308104626, -2.071067811865468400, 4.999999999999989342 ) ) ;
#28865 = CARTESIAN_POINT ( 'NONE',  ( 0.000000000000000000, 0.000000000000000000, 0.000000000000000000 ) ) ;
#28866 = CARTESIAN_POINT ( 'NONE',  ( -4.000000000000004441, 7.119033245839730840E-16, 5.040519776325966696E-35 ) ) ;
#28867 = CYLINDRICAL_SURFACE ( 'NONE', #29247, 6.000000000000000888 ) ;
#28868 = CARTESIAN_POINT ( 'NONE',  ( 0.000000000000000000, 0.000000000000000000, 0.000000000000000000 ) ) ;
#28869 = CARTESIAN_POINT ( 'NONE',  ( 105.9999999999998863, 2.500000000000002220, 1.110223024625156540E-13 ) ) ;
#28870 = CARTESIAN_POINT ( 'NONE',  ( 0.000000000000000000, 0.000000000000000000, 0.000000000000000000 ) ) ;
#28871 = CARTESIAN_POINT ( 'NONE',  ( -3.175426480542816510, -5.500000000000057732, -137.3750000000000568 ) ) ;
#28872 = CARTESIAN_POINT ( 'NONE',  ( 0.000000000000000000, 0.000000000000000000, 0.000000000000000000 ) ) ;
#28873 = ORIENTED_EDGE ( 'NONE', *, *, #642, .T. ) ;
#28874 = CARTESIAN_POINT ( 'NONE',  ( 4.763139720814407951, 2.750000000000002665, -48.25000000000001421 ) ) ;
#28875 = DIRECTION ( 'NONE',  ( -3.845925372767118265E-16, 1.000000000000000000, 8.881784197001258240E-16 ) ) ;
#28876 = DIRECTION ( 'NONE',  ( 0.000000000000000000, 0.000000000000000000, 1.000000000000000000 ) ) ;
#28877 = EDGE_LOOP ( 'NONE', ( #13650, #23222, #11927, #24790 ) ) ;
#28878 = CARTESIAN_POINT ( 'NONE',  ( 119.2497167782374987, -1.308140751793557266, -1.308140751793640533 ) ) ;
#28879 = SURFACE_STYLE_USAGE ( .BOTH. , #24138 ) ;
#28880 = APPLICATION_CONTEXT ( 'automotive_design' ) ;
#28881 = CARTESIAN_POINT ( 'NONE',  ( -5.412658773652684552, -3.125000000000099920, -95.06698729810780435 ) ) ;
#28882 = DIRECTION ( 'NONE',  ( -7.147005652999508048E-36, 5.642372883946980038E-36, 1.000000000000000000 ) ) ;
#28883 = CARTESIAN_POINT ( 'NONE',  ( 155.8199251345948255, -2.278174593051950136, -5.500000000000074607 ) ) ;
#28884 = CARTESIAN_POINT ( 'NONE',  ( 113.2499999999998437, 2.775557561562891351E-14, 2.500000000000168754 ) ) ;
#28885 = CARTESIAN_POINT ( 'NONE',  ( 6.000000000000000888, 1.743066579297358182E-13, -78.08632486540520290 ) ) ;
#28886 = CARTESIAN_POINT ( 'NONE',  ( -3.175426480542816510, -5.500000000000057732, -132.8750000000000284 ) ) ;
#28887 = ADVANCED_FACE ( 'NONE', ( #23979 ), #29502, .T. ) ;
#28888 = EDGE_LOOP ( 'NONE', ( #21361, #28393, #14157, #15882 ) ) ;
#28889 = ORIENTED_EDGE ( 'NONE', *, *, #17953, .T. ) ;
#28890 = FACE_OUTER_BOUND ( 'NONE', #18200, .T. ) ;
#28891 = CARTESIAN_POINT ( 'NONE',  ( 3.175426480543072749, 5.499999999999865885, -60.12499999999999289 ) ) ;
#28892 = AXIS2_PLACEMENT_3D ( 'NONE', #6013, #19845, #29193 ) ;
#28893 = CARTESIAN_POINT ( 'NONE',  ( -3.464101615137725076, 5.999999999999979572, -69.16367513459479710 ) ) ;
#28894 = CARTESIAN_POINT ( 'NONE',  ( 0.000000000000000000, -5.999999999999991118, -134.5386751345948255 ) ) ;
#28895 = CARTESIAN_POINT ( 'NONE',  ( 2.511346088335001170, 10.71107091704333847, -30.45263927933801540 ) ) ;
#28896 = CARTESIAN_POINT ( 'NONE',  ( 3.608439182435180470, -6.249999999999997335, -73.05801270189222407 ) ) ;
#28897 = VECTOR ( 'NONE', #18229, 1000.000000000000000 ) ;
#28898 = FACE_OUTER_BOUND ( 'NONE', #25785, .T. ) ;
#28899 = DIRECTION ( 'NONE',  ( -1.000000000000000000, -1.665334536937731113E-16, 1.526556658859586792E-16 ) ) ;
#28900 = CARTESIAN_POINT ( 'NONE',  ( 116.0000000000000142, 0.000000000000000000, 0.000000000000000000 ) ) ;
#28901 = CARTESIAN_POINT ( 'NONE',  ( 3.175426480543072749, -5.500000000000105693, -143.1250000000000000 ) ) ;
#28902 = CARTESIAN_POINT ( 'NONE',  ( -10.00000000000000178, -19.99999999999998934, 3.000000000000002665 ) ) ;
#28903 = CARTESIAN_POINT ( 'NONE',  ( -3.608439182435052128, -6.250000000000110134, -152.8080127018922099 ) ) ;
#28904 = DIRECTION ( 'NONE',  ( -7.147005652999508048E-36, 5.642372883946980038E-36, 1.000000000000000000 ) ) ;
#28905 = CARTESIAN_POINT ( 'NONE',  ( -5.196152422706601826, 2.999999999999975131, -66.96132486540523132 ) ) ;
#28906 = CARTESIAN_POINT ( 'NONE',  ( 0.000000000000000000, 5.499999999999991118, -73.50000000000001421 ) ) ;
#28907 = CARTESIAN_POINT ( 'NONE',  ( 5.999999999999949374, 1.607695154586804565, -86.09668783648704959 ) ) ;
#28908 = CARTESIAN_POINT ( 'NONE',  ( 4.763139720814407951, -2.749999999999988454, -60.50000000000000000 ) ) ;
#28909 = ORIENTED_EDGE ( 'NONE', *, *, #5445, .T. ) ;
#28910 = CARTESIAN_POINT ( 'NONE',  ( 138.1086002691896510, -2.071067811865468400, -4.999999999999989342 ) ) ;
#28911 = CARTESIAN_POINT ( 'NONE',  ( 149.2500000000000284, -6.000000000000005329, 0.000000000000000000 ) ) ;
#28912 = DIRECTION ( 'NONE',  ( 1.000000000000000000, -5.551115123125774074E-17, -1.260129944081490070E-35 ) ) ;
#28913 = EDGE_CURVE ( 'NONE', #23806, #29780, #26124, .T. ) ;
#28914 = DIRECTION ( 'NONE',  ( 1.000000000000000000, -5.551115123125773458E-17, -1.260129944081490338E-35 ) ) ;
#28915 = CARTESIAN_POINT ( 'NONE',  ( 114.6247167782376124, 1.849990392679523588, 0.000000000000000000 ) ) ;
#28916 = EDGE_LOOP ( 'NONE', ( #20757, #20311, #14483, #2617 ) ) ;
#28917 = COLOUR_RGB ( '', 0.66274510, 0.83137255, 0.94901961) ;
#28918 = CARTESIAN_POINT ( 'NONE',  ( 146.5312500000000284, -2.485281374238555774, -6.000000000000005329 ) ) ;
#28919 = LINE ( 'NONE', #22338, #27794 ) ;
#28920 = AXIS2_PLACEMENT_3D ( 'NONE', #6148, #15563, #29486 ) ;
#28921 = CARTESIAN_POINT ( 'NONE',  ( 104.8283649806521396, 0.8716379956768015580, 1.698308124453599799 ) ) ;
#28922 =( BOUNDED_CURVE ( )  B_SPLINE_CURVE ( 2, ( #28342, #10085, #11978, #14849, #12560, #23905, #17013, #10240, #543 ),
 .UNSPECIFIED., .F., .T. ) 
 B_SPLINE_CURVE_WITH_KNOTS ( ( 3, 2, 2, 2, 3 ),
 ( 0.5875000000000001332, 0.5937500000000003331, 0.6000000000000005329, 0.6062500000000007327, 0.6125000000000010436 ),
 .UNSPECIFIED. ) 
 CURVE ( )  GEOMETRIC_REPRESENTATION_ITEM ( )  RATIONAL_B_SPLINE_CURVE ( ( 0.9999999999999986677, 0.9238795325112880708, 1.000000000000000000, 0.9238795325112867385, 1.000000000000000000, 0.9238795325112867385, 1.000000000000000000, 0.9238795325112745260, 1.000000000000012212 ) ) 
 REPRESENTATION_ITEM ( '' )  );
#28923 = EDGE_CURVE ( 'NONE', #11992, #25088, #13886, .T. ) ;
#28924 = CARTESIAN_POINT ( 'NONE',  ( -5.412658773652684552, -3.125000000000099920, -47.06698729810781856 ) ) ;
#28925 = CARTESIAN_POINT ( 'NONE',  ( 15.68750000000012434, -0.8284271247459350507, -2.000000000000031530 ) ) ;
#28926 = CARTESIAN_POINT ( 'NONE',  ( 2.775557561562891351E-14, -6.250000000000061284, -148.8169872981078186 ) ) ;
#28927 = ORIENTED_EDGE ( 'NONE', *, *, #26499, .T. ) ;
#28928 = CARTESIAN_POINT ( 'NONE',  ( 3.175426480543072749, 5.499999999999865885, -78.12500000000001421 ) ) ;
#28929 = CARTESIAN_POINT ( 'NONE',  ( -3.608439182435115633, 6.249999999999965361, -94.80801270189219565 ) ) ;
#28930 = CARTESIAN_POINT ( 'NONE',  ( 5.999999999999998224, 1.607695154586720854, -176.0966878364870070 ) ) ;
#28931 = CARTESIAN_POINT ( 'NONE',  ( 21.53867513459484329, 0.000000000000000000, 2.500000000000002220 ) ) ;
#28932 = CARTESIAN_POINT ( 'NONE',  ( 162.0000000000000284, 0.000000000000000000, 0.000000000000000000 ) ) ;
#28933 = MECHANICAL_DESIGN_GEOMETRIC_PRESENTATION_REPRESENTATION (  '', ( #5393 ), #18219 ) ;
#28934 = SURFACE_STYLE_USAGE ( .BOTH. , #387 ) ;
#28935 = CARTESIAN_POINT ( 'NONE',  ( 6.000000000000000888, -1.607695154586752384, -58.65331216351298593 ) ) ;
#28936 = CARTESIAN_POINT ( 'NONE',  ( 0.000000000000000000, 0.000000000000000000, 0.000000000000000000 ) ) ;
#28937 = AXIS2_PLACEMENT_3D ( 'NONE', #6814, #11311, #25230 ) ;
#28938 = CARTESIAN_POINT ( 'NONE',  ( 3.175426480543072749, 5.499999999999865885, -165.1250000000000000 ) ) ;
#28939 = CARTESIAN_POINT ( 'NONE',  ( 6.000000000000000888, 1.743066579297358182E-13, -60.08632486540520290 ) ) ;
#28940 = CARTESIAN_POINT ( 'NONE',  ( 4.763139720814407951, 2.750000000000002665, -145.7500000000000568 ) ) ;
#28941 = DIRECTION ( 'NONE',  ( 0.000000000000000000, -1.000000000000000000, 0.000000000000000000 ) ) ;
#28942 = CARTESIAN_POINT ( 'NONE',  ( 148.6800748654052029, -2.278174593052027408, 5.499999999999996447 ) ) ;
#28943 = CARTESIAN_POINT ( 'NONE',  ( -4.763139720814407951, 2.749999999999946709, -97.25000000000000000 ) ) ;
#28944 = CARTESIAN_POINT ( 'NONE',  ( 3.175426480543072749, -5.500000000000105693, -81.62500000000002842 ) ) ;
#28945 = CARTESIAN_POINT ( 'NONE',  ( -5.999999999999962697, 3.323446944526963891E-14, -159.8363248654052597 ) ) ;
#28946 = CYLINDRICAL_SURFACE ( 'NONE', #6637, 6.000000000000000888 ) ;
#28947 = CARTESIAN_POINT ( 'NONE',  ( 22.62500000000017408, -1.414213562372867994, -1.414213562373034527 ) ) ;
#28948 = EDGE_CURVE ( 'NONE', #3793, #16482, #28709, .T. ) ;
#28949 = CARTESIAN_POINT ( 'NONE',  ( 10.64882486540527395, 2.500000000000144773, -1.035533905932929599 ) ) ;
#28950 = CARTESIAN_POINT ( 'NONE',  ( -6.000000000000007105, -1.607695154586655129, -74.26933756729742697 ) ) ;
#28951 = CARTESIAN_POINT ( 'NONE',  ( 20.03867513459486815, 1.665334536937734811E-13, -2.500000000000057732 ) ) ;
#28952 = ORIENTED_EDGE ( 'NONE', *, *, #21062, .T. ) ;
#28953 = CARTESIAN_POINT ( 'NONE',  ( 159.8437500000000000, -6.000000000000005329, -2.485281374238555774 ) ) ;
#28954 = CYLINDRICAL_SURFACE ( 'NONE', #22427, 11.00000000000001599 ) ;
#28955 = CARTESIAN_POINT ( 'NONE',  ( -3.464101615137757051, -5.999999999999979572, -79.16367513459483973 ) ) ;
#28956 = CARTESIAN_POINT ( 'NONE',  ( 104.3122167782373992, -0.7662911109076785410, -1.849990392679291551 ) ) ;
#28957 = ORIENTED_EDGE ( 'NONE', *, *, #29666, .T. ) ;
#28958 = ADVANCED_FACE ( 'NONE', ( #17090 ), #29013, .T. ) ;
#28959 = AXIS2_PLACEMENT_3D ( 'NONE', #7906, #1296, #20054 ) ;
#28960 = ORIENTED_EDGE ( 'NONE', *, *, #23760, .T. ) ;
#28961 = CARTESIAN_POINT ( 'NONE',  ( 146.5312500000000284, -2.485281374238555774, -6.000000000000005329 ) ) ;
#28962 = ORIENTED_EDGE ( 'NONE', *, *, #1817, .T. ) ;
#28963 = CARTESIAN_POINT ( 'NONE',  ( -3.175426480542816510, 5.499999999999865885, -106.3750000000000284 ) ) ;
#28964 = CARTESIAN_POINT ( 'NONE',  ( 19.75000000000009948, -1.873492889144789952, 1.873492889144900975 ) ) ;
#28965 = CARTESIAN_POINT ( 'NONE',  ( -5.412658773652684552, -3.125000000000099920, -124.4330127018922241 ) ) ;
#28966 = CARTESIAN_POINT ( 'NONE',  ( 114.0238248654048903, -0.8284271247461453269, 2.000000000000271783 ) ) ;
#28967 = CARTESIAN_POINT ( 'NONE',  ( 5.412658773652739619, 3.124999999999988898, -163.3169872981078470 ) ) ;
#28968 = DIRECTION ( 'NONE',  ( 0.000000000000000000, -1.000000000000000000, -8.881784197001262184E-16 ) ) ;
#28969 = VECTOR ( 'NONE', #19828, 1000.000000000000000 ) ;
#28970 = CARTESIAN_POINT ( 'NONE',  ( -5.412658773652684552, -3.125000000000099920, -62.93301270189222407 ) ) ;
#28971 = ORIENTED_EDGE ( 'NONE', *, *, #16238, .T. ) ;
#28972 = CARTESIAN_POINT ( 'NONE',  ( 6.000000000000000888, -3.330669073875464691E-16, -7.560779664488942560E-35 ) ) ;
#28973 = CARTESIAN_POINT ( 'NONE',  ( 22.78867513459492500, -2.499999999999891198, -5.551115123125782702E-14 ) ) ;
#28974 = CARTESIAN_POINT ( 'NONE',  ( -5.841785975170636469, 9.320713607846746740, -23.61690496628341407 ) ) ;
#28975 = CARTESIAN_POINT ( 'NONE',  ( -4.763139720814407951, 2.749999999999946709, -167.7500000000000000 ) ) ;
#28976 = CARTESIAN_POINT ( 'NONE',  ( 119.8749999999998863, 1.767766952966320915, -1.767766952966320915 ) ) ;
#28977 = CARTESIAN_POINT ( 'NONE',  ( -5.999999999999963585, 9.296355089585909904E-15, -169.4136751345948539 ) ) ;
#28978 = CARTESIAN_POINT ( 'NONE',  ( 2.775557561562891351E-14, 6.250000000000033751, -172.9330127018922099 ) ) ;
#28979 = CARTESIAN_POINT ( 'NONE',  ( -0.5130136762305975706, -9.973972647538824177, 4.738252045315890726 ) ) ;
#28980 = LINE ( 'NONE', #1031, #11399 ) ;
#28981 = AXIS2_PLACEMENT_3D ( 'NONE', #1412, #8638, #8481 ) ;
#28982 = CARTESIAN_POINT ( 'NONE',  ( -2.775557561562891351E-14, -5.500000000000115463, -117.7500000000000284 ) ) ;
#28983 = SURFACE_SIDE_STYLE ('',( #17058 ) ) ;
#28984 = CARTESIAN_POINT ( 'NONE',  ( -2.775557561562891351E-14, -5.500000000000115463, -102.7500000000000142 ) ) ;
#28985 = CARTESIAN_POINT ( 'NONE',  ( -5.196152422706573404, -3.000000000000002665, -131.7886751345947971 ) ) ;
#28986 = EDGE_LOOP ( 'NONE', ( #23529, #17941, #17950, #6005, #17524 ) ) ;
#28987 = CARTESIAN_POINT ( 'NONE',  ( 17.68750000000000355, 2.649519052838298805, 1.097466725451439196 ) ) ;
#28988 = CARTESIAN_POINT ( 'NONE',  ( 0.000000000000000000, 0.000000000000000000, 0.000000000000000000 ) ) ;
#28989 = EDGE_CURVE ( 'NONE', #1067, #13876, #15829, .T. ) ;
#28990 = DIRECTION ( 'NONE',  ( -1.000000000000000000, 0.000000000000000000, 0.000000000000000000 ) ) ;
#28991 = CARTESIAN_POINT ( 'NONE',  ( 3.464101615137852974, 5.999999999999884537, -86.83632486540520290 ) ) ;
#28992 = CARTESIAN_POINT ( 'NONE',  ( 6.000000000000000888, -1.859271017917181981E-14, -126.6636751345948397 ) ) ;
#28993 = CARTESIAN_POINT ( 'NONE',  ( 2.775557561562891351E-14, -6.250000000000061284, -78.31698729810781856 ) ) ;
#28994 = CYLINDRICAL_SURFACE ( 'NONE', #19996, 6.000000000000000888 ) ;
#28995 = EDGE_LOOP ( 'NONE', ( #10112, #4506, #22915, #24868, #3727, #17837, #12211, #18425, #27722, #14515, #28957, #12954, #21021, #26585, #24581, #24314, #4685, #17197, #11107, #16887, #13540, #11607, #16809, #15850, #12619, #21151, #21488, #15573, #22067, #25808, #28087, #16475, #26406, #18049, #3781, #21966, #27683, #6544, #3352 ) ) ;
#28996 = EDGE_CURVE ( 'NONE', #20381, #13576, #26417, .T. ) ;
#28997 = CARTESIAN_POINT ( 'NONE',  ( 116.0863248654050608, -1.414213562373090038, 1.414213562373256572 ) ) ;
#28998 = ORIENTED_EDGE ( 'NONE', *, *, #9883, .F. ) ;
#28999 = CARTESIAN_POINT ( 'NONE',  ( 132.8586002691896510, 2.071067811865468400, 4.999999999999989342 ) ) ;
#29000 = AXIS2_PLACEMENT_3D ( 'NONE', #6141, #15555, #28077 ) ;
#29001 = ORIENTED_EDGE ( 'NONE', *, *, #13341, .F. ) ;
#29002 = DIRECTION ( 'NONE',  ( 1.000000000000000000, 0.000000000000000000, 0.000000000000000000 ) ) ;
#29003 = CARTESIAN_POINT ( 'NONE',  ( -3.608439182435115633, 6.249999999999965361, -132.9419872981078186 ) ) ;
#29004 = CARTESIAN_POINT ( 'NONE',  ( 3.464101615137757051, -5.999999999999979572, -135.3363248654052313 ) ) ;
#29005 = CARTESIAN_POINT ( 'NONE',  ( 0.000000000000000000, -5.999999999999991118, -167.5386751345948539 ) ) ;
#29006 = CARTESIAN_POINT ( 'NONE',  ( 20.02382486540529172, -1.035533905932568999, 2.499999999999844569 ) ) ;
#29007 = ORIENTED_EDGE ( 'NONE', *, *, #14398, .T. ) ;
#29008 = CARTESIAN_POINT ( 'NONE',  ( 15.81250000000000178, 0.8284271247462354770, -2.000000000000151879 ) ) ;
#29009 = CARTESIAN_POINT ( 'NONE',  ( -6.000000000000000888, 1.067854986875958443E-15, 7.560779664488942560E-35 ) ) ;
#29010 =( BOUNDED_CURVE ( )  B_SPLINE_CURVE ( 2, ( #17872, #18735, #11687, #1546, #6160, #6458, #15577, #24890, #16448 ),
 .UNSPECIFIED., .F., .T. ) 
 B_SPLINE_CURVE_WITH_KNOTS ( ( 3, 2, 2, 2, 3 ),
 ( 0.5294117647058823595, 0.5367647058823529216, 0.5441176470588235947, 0.5514705882352941568, 0.5588235294117647189 ),
 .UNSPECIFIED. ) 
 CURVE ( )  GEOMETRIC_REPRESENTATION_ITEM ( )  RATIONAL_B_SPLINE_CURVE ( ( 1.000000000000000000, 0.9238795325112867385, 1.000000000000000000, 0.9238795325112867385, 1.000000000000000000, 0.9238795325112867385, 1.000000000000000000, 0.9238795325112867385, 1.000000000000000000 ) ) 
 REPRESENTATION_ITEM ( '' )  );
#29011 = CARTESIAN_POINT ( 'NONE',  ( 5.999999999999949374, 1.607695154586804565, -57.01933756729742697 ) ) ;
#29012 = CARTESIAN_POINT ( 'NONE',  ( 138.0788997308104342, -4.999999999999989342, 2.071067811865468400 ) ) ;
#29013 = CYLINDRICAL_SURFACE ( 'NONE', #20685, 6.000000000000000888 ) ;
#29014 = CARTESIAN_POINT ( 'NONE',  ( -5.999999999999963585, 8.134310703387671600E-14, -140.3363248654052313 ) ) ;
#29015 = CARTESIAN_POINT ( 'NONE',  ( 5.412658773652712085, -3.125000000000086153, -69.06698729810784698 ) ) ;
#29016 = CIRCLE ( 'NONE', #15844, 15.99999999999998579 ) ;
#29017 = CARTESIAN_POINT ( 'NONE',  ( -5.412658773652684552, -3.125000000000099920, -51.56698729810782567 ) ) ;
#29018 = CARTESIAN_POINT ( 'NONE',  ( 0.000000000000000000, 0.000000000000000000, 0.000000000000000000 ) ) ;
#29019 = DIRECTION ( 'NONE',  ( -1.000000000000000000, -3.469446951953614189E-15, 0.000000000000000000 ) ) ;
#29020 = CARTESIAN_POINT ( 'NONE',  ( 107.6874999999997868, -1.035533905932659149, -2.499999999999724221 ) ) ;
#29021 = CARTESIAN_POINT ( 'NONE',  ( -5.999999999999919176, 1.607695154586804565, -74.40331216351303567 ) ) ;
#29022 = CARTESIAN_POINT ( 'NONE',  ( 4.763139720814407951, -2.749999999999988454, -126.5000000000000568 ) ) ;
#29023 = ORIENTED_EDGE ( 'NONE', *, *, #25051, .T. ) ;
#29024 = PRESENTATION_STYLE_ASSIGNMENT (( #10318 ) ) ;
#29025 = EDGE_CURVE ( 'NONE', #15666, #2682, #20117, .T. ) ;
#29026 = DIRECTION ( 'NONE',  ( -0.000000000000000000, 1.000000000000000000, -0.000000000000000000 ) ) ;
#29027 = PLANE ( 'NONE',  #29613 ) ;
#29028 = DIRECTION ( 'NONE',  ( -1.000000000000000000, 0.000000000000000000, 0.000000000000000000 ) ) ;
#29029 = EDGE_CURVE ( 'NONE', #10410, #22270, #2268, .T. ) ;
#29030 = CARTESIAN_POINT ( 'NONE',  ( -3.464101615137757051, -5.999999999999979572, -144.5863248654052029 ) ) ;
#29031 = VERTEX_POINT ( 'NONE', #22130 ) ;
#29032 = PRODUCT_DEFINITION ( 'UNKNOWN', '', #15416, #23863 ) ;
#29033 = CARTESIAN_POINT ( 'NONE',  ( 113.7497167782375698, 1.308140751793557266, 1.308140751793751555 ) ) ;
#29034 = CARTESIAN_POINT ( 'NONE',  ( 135.3750000000000284, 0.000000000000000000, 6.000000000000005329 ) ) ;
#29035 = CARTESIAN_POINT ( 'NONE',  ( 10.56250000000007461, -1.999999999999971800, -0.8284271247462354770 ) ) ;
#29036 = CARTESIAN_POINT ( 'NONE',  ( 5.412658773652739619, 3.124999999999988898, -92.81698729810783277 ) ) ;
#29037 = CARTESIAN_POINT ( 'NONE',  ( 11.27382486540526685, -2.499999999999904521, -1.035533905932749299 ) ) ;
#29038 = CARTESIAN_POINT ( 'NONE',  ( 112.8124999999998579, 1.035533905932779275, -2.499999999999904521 ) ) ;
#29039 = LINE ( 'NONE', #28327, #2813 ) ;
#29040 = DIRECTION ( 'NONE',  ( 5.551115123125785167E-17, -1.000000000000000000, -8.881784197001256268E-16 ) ) ;
#29041 = CARTESIAN_POINT ( 'NONE',  ( 9.937500000000083489, 2.000000000000151879, -0.8284271247463557142 ) ) ;
#29042 = ORIENTED_EDGE ( 'NONE', *, *, #7345, .F. ) ;
#29043 = CARTESIAN_POINT ( 'NONE',  ( -5.196152422706573404, -3.000000000000002665, -138.7113248654052029 ) ) ;
#29044 = CARTESIAN_POINT ( 'NONE',  ( -3.175426480542816510, -5.500000000000057732, -56.37500000000004263 ) ) ;
#29045 = CARTESIAN_POINT ( 'NONE',  ( 158.9136751345948539, 0.000000000000000000, -5.500000000000005329 ) ) ;
#29046 = CARTESIAN_POINT ( 'NONE',  ( -5.999999999999963585, 8.134310703387671600E-14, -116.3363248654052313 ) ) ;
#29047 =( NAMED_UNIT ( * ) SI_UNIT ( $, .STERADIAN. ) SOLID_ANGLE_UNIT ( ) );
#29048 = CARTESIAN_POINT ( 'NONE',  ( -3.608439182435052128, -6.250000000000110134, -79.30801270189226670 ) ) ;
#29049 = DIRECTION ( 'NONE',  ( -7.147005652999508048E-36, 5.642372883946980038E-36, 1.000000000000000000 ) ) ;
#29050 = CARTESIAN_POINT ( 'NONE',  ( 155.9851497308104058, -3.535533905932725318, 3.535533905932725318 ) ) ;
#29051 = DIRECTION ( 'NONE',  ( -1.000000000000000000, 0.000000000000000000, 0.000000000000000000 ) ) ;
#29052 = CARTESIAN_POINT ( 'NONE',  ( 5.196152422706629359, 3.000000000000002665, -80.03867513459483973 ) ) ;
#29053 = FILL_AREA_STYLE_COLOUR ( '', #19210 ) ;
#29054 = AXIS2_PLACEMENT_3D ( 'NONE', #6856, #6390, #9020 ) ;
#29055 = CARTESIAN_POINT ( 'NONE',  ( -2.775557561562891351E-14, -5.500000000000115463, -134.2500000000000284 ) ) ;
#29056 = LINE ( 'NONE', #12827, #25079 ) ;
#29057 = CARTESIAN_POINT ( 'NONE',  ( -5.999999999999962697, 3.323446944526963891E-14, -152.3363248654052313 ) ) ;
#29058 = CARTESIAN_POINT ( 'NONE',  ( 146.9925748654052313, 2.278174593052027408, 5.499999999999996447 ) ) ;
#29059 = CARTESIAN_POINT ( 'NONE',  ( 6.350852961086080661, -9.614813431917819062E-14, -73.87500000000000000 ) ) ;
#29060 = CARTESIAN_POINT ( 'NONE',  ( 0.000000000000000000, 5.499999999999991118, -60.00000000000005684 ) ) ;
#29061 = EDGE_CURVE ( 'NONE', #22693, #4573, #10616, .T. ) ;
#29062 = CARTESIAN_POINT ( 'NONE',  ( 116.0000000000000142, 0.000000000000000000, 0.000000000000000000 ) ) ;
#29063 = ORIENTED_EDGE ( 'NONE', *, *, #14744, .T. ) ;
#29064 = CARTESIAN_POINT ( 'NONE',  ( 155.0625000000000284, -4.242640687119298093, 4.242640687119298093 ) ) ;
#29065 = CARTESIAN_POINT ( 'NONE',  ( 135.5000000000000000, -54.99999999999993605, 7.500000000000007105 ) ) ;
#29066 = CARTESIAN_POINT ( 'NONE',  ( 14.37500000000016520, -1.414213562373034527, 1.414213562372979016 ) ) ;
#29067 = CARTESIAN_POINT ( 'NONE',  ( 114.7738248654050182, 2.000000000000061728, 0.8284271247462955401 ) ) ;
#29068 = MECHANICAL_DESIGN_GEOMETRIC_PRESENTATION_REPRESENTATION (  '', ( #4555 ), #19765 ) ;
#29069 = ORIENTED_EDGE ( 'NONE', *, *, #7947, .T. ) ;
#29070 = CARTESIAN_POINT ( 'NONE',  ( 145.0312500000000568, -2.485281374238555774, -6.000000000000005329 ) ) ;
#29071 = DIRECTION ( 'NONE',  ( -1.000000000000000000, -1.665334536937736783E-16, -2.220446049250315546E-16 ) ) ;
#29072 = CARTESIAN_POINT ( 'NONE',  ( -6.000000000000007105, -1.607695154586655129, -102.7693375672974270 ) ) ;
#29073 = CARTESIAN_POINT ( 'NONE',  ( 4.763139720814407951, -2.749999999999988454, -179.0000000000000568 ) ) ;
#29074 = CARTESIAN_POINT ( 'NONE',  ( 16.81250000000007816, 0.8284271247462955401, -2.000000000000091926 ) ) ;
#29075 = ORIENTED_EDGE ( 'NONE', *, *, #1434, .T. ) ;
#29076 = CARTESIAN_POINT ( 'NONE',  ( 2.775557561562891351E-14, -6.250000000000061284, -145.8169872981078186 ) ) ;
#29077 = CARTESIAN_POINT ( 'NONE',  ( -6.350852961085760029, -1.281975124255709124E-13, -80.62500000000004263 ) ) ;
#29078 = CARTESIAN_POINT ( 'NONE',  ( 14.87500000000011013, -2.649519052838111843, 0.000000000000000000 ) ) ;
#29079 = CARTESIAN_POINT ( 'NONE',  ( -5.412658773652739619, 3.124999999999975131, -94.68301270189222407 ) ) ;
#29080 = CARTESIAN_POINT ( 'NONE',  ( 6.000000000000000888, -1.859271017917181981E-14, -105.6636751345948397 ) ) ;
#29081 = EDGE_CURVE ( 'NONE', #1732, #21964, #17278, .T. ) ;
#29082 = CARTESIAN_POINT ( 'NONE',  ( 0.000000000000000000, -5.999999999999991118, -151.0386751345948539 ) ) ;
#29083 = CARTESIAN_POINT ( 'NONE',  ( 140.0000000000000284, -11.48545691804907420, -4.867024281885878878 ) ) ;
#29084 = CARTESIAN_POINT ( 'NONE',  ( 134.5875105163469811, -7.951309655804374543, 8.000000000000007105 ) ) ;
#29085 = CARTESIAN_POINT ( 'NONE',  ( 6.350852961086080661, -9.614813431917819062E-14, -163.8750000000000568 ) ) ;
#29086 = CARTESIAN_POINT ( 'NONE',  ( 118.0863248654050039, -1.414213562373034527, 1.414213562373256572 ) ) ;
#29087 = CARTESIAN_POINT ( 'NONE',  ( -3.175426480542816510, 5.499999999999865885, -146.8750000000000284 ) ) ;
#29088 = LINE ( 'NONE', #8049, #19395 ) ;
#29089 = CARTESIAN_POINT ( 'NONE',  ( 3.175426480543072749, 5.499999999999865885, -93.12500000000002842 ) ) ;
#29090 = DIRECTION ( 'NONE',  ( -1.000000000000000000, 0.000000000000000000, 0.000000000000000000 ) ) ;
#29091 = CARTESIAN_POINT ( 'NONE',  ( -4.763139720814407951, 2.749999999999946709, -80.74999999999998579 ) ) ;
#29092 = ADVANCED_FACE ( 'NONE', ( #13251 ), #10934, .T. ) ;
#29093 = CARTESIAN_POINT ( 'NONE',  ( 154.0461002691896795, -2.071067811865468400, 4.999999999999989342 ) ) ;
#29094 = CARTESIAN_POINT ( 'NONE',  ( 5.999999999999949374, 1.607695154586804565, -65.09668783648702117 ) ) ;
#29095 = CARTESIAN_POINT ( 'NONE',  ( 139.9669392956159300, -9.668196137844805804, -7.713418679898259356 ) ) ;
#29096 = CARTESIAN_POINT ( 'NONE',  ( 18.46132486540535922, 1.665334536937734811E-13, -2.500000000000113243 ) ) ;
#29097 = CARTESIAN_POINT ( 'NONE',  ( 0.000000000000000000, 5.999999999999977796, -124.7886751345948539 ) ) ;
#29098 = DIRECTION ( 'NONE',  ( -1.000000000000000000, -1.665334536937736783E-16, -2.220446049250315546E-16 ) ) ;
#29099 = CARTESIAN_POINT ( 'NONE',  ( -5.999999999999919176, 1.607695154586804565, -74.98066243270262987 ) ) ;
#29100 =( BOUNDED_CURVE ( )  B_SPLINE_CURVE ( 2, ( #16192, #2174, #9232, #16641, #18781, #25818, #25962, #7078, #23678 ),
 .UNSPECIFIED., .F., .T. ) 
 B_SPLINE_CURVE_WITH_KNOTS ( ( 3, 2, 2, 2, 3 ),
 ( 0.2916666666666666297, 0.2925925925925925708, 0.2944444444444444531, 0.2962962962962962798, 0.2972222222222222210 ),
 .UNSPECIFIED. ) 
 CURVE ( )  GEOMETRIC_REPRESENTATION_ITEM ( )  RATIONAL_B_SPLINE_CURVE ( ( 0.9330127018922194093, 0.9330127018922174109, 1.000000000000000000, 0.8660254037844388186, 1.000000000000000000, 0.8660254037844388186, 1.000000000000000000, 0.9330127018922194093, 0.9330127018922194093 ) ) 
 REPRESENTATION_ITEM ( '' )  );
#29101 = ORIENTED_EDGE ( 'NONE', *, *, #12403, .F. ) ;
#29102 = CARTESIAN_POINT ( 'NONE',  ( 6.000000000000000888, 1.743066579297358182E-13, -91.58632486540523132 ) ) ;
#29103 = DIRECTION ( 'NONE',  ( -8.326672684688675286E-17, -2.081668171172168821E-17, 1.000000000000000000 ) ) ;
#29104 = CARTESIAN_POINT ( 'NONE',  ( 5.196152422706629359, 3.000000000000002665, -83.03867513459483973 ) ) ;
#29105 = CARTESIAN_POINT ( 'NONE',  ( 120.2502832217622739, 1.308140751793612777, -1.308140751793418488 ) ) ;
#29106 = ORIENTED_EDGE ( 'NONE', *, *, #12207, .F. ) ;
#29107 = CLOSED_SHELL ( 'NONE', ( #2752, #4215, #13283, #12573, #13809, #25927, #6717, #21709, #8881, #19116, #27956, #11114, #29557, #24150, #10609, #30307, #11551, #16018, #1225, #10335, #19149, #3501, #5578, #24127, #16166, #17592, #14524, #28032, #16228, #19419, #2256, #14717, #22075, #21644, #26600, #14264, #17780, #22780, #6118, #17287 ) ) ;
#29108 = ORIENTED_EDGE ( 'NONE', *, *, #14651, .F. ) ;
#29109 = CARTESIAN_POINT ( 'NONE',  ( -3.175426480542816510, 5.499999999999865885, -104.8750000000000142 ) ) ;
#29110 = CARTESIAN_POINT ( 'NONE',  ( 16.75000000000015277, -1.873492889144789952, 1.873492889144956486 ) ) ;
#29111 = CARTESIAN_POINT ( 'NONE',  ( -3.608439182435052128, -6.250000000000110134, -116.8080127018922383 ) ) ;
#29112 = ORIENTED_EDGE ( 'NONE', *, *, #17222, .F. ) ;
#29113 = CARTESIAN_POINT ( 'NONE',  ( -5.999999999999919176, 1.607695154586804565, -110.9806624327025872 ) ) ;
#29114 = CARTESIAN_POINT ( 'NONE',  ( 2.775557561562891351E-14, 6.250000000000033751, -157.0669872981078754 ) ) ;
#29115 = CARTESIAN_POINT ( 'NONE',  ( 104.6874999999998579, -1.035533905932689347, -2.499999999999724221 ) ) ;
#29116 = CARTESIAN_POINT ( 'NONE',  ( 21.41367513459496763, 1.767766952966487448, 1.767766952966376426 ) ) ;
#29117 = EDGE_CURVE ( 'NONE', #29147, #4124, #5377, .T. ) ;
#29118 = CARTESIAN_POINT ( 'NONE',  ( 2.775557561562891351E-14, -6.250000000000061284, -52.18301270189223828 ) ) ;
#29119 = ORIENTED_EDGE ( 'NONE', *, *, #20033, .F. ) ;
#29120 = LINE ( 'NONE', #5773, #17188 ) ;
#29121 = DIRECTION ( 'NONE',  ( -7.147005652999508048E-36, 5.642372883946980038E-36, 1.000000000000000000 ) ) ;
#29122 = CARTESIAN_POINT ( 'NONE',  ( -19.99999999999998224, -54.99999999999990763, 7.500000000000007105 ) ) ;
#29123 = DIRECTION ( 'NONE',  ( 1.000000000000000000, -5.551115123125773458E-17, -1.260129944081490338E-35 ) ) ;
#29124 = CARTESIAN_POINT ( 'NONE',  ( -3.175426480542816510, 5.499999999999865885, -173.8750000000000000 ) ) ;
#29125 = CARTESIAN_POINT ( 'NONE',  ( 120.6874999999997584, -1.035533905932719101, -2.499999999999844569 ) ) ;
#29126 = CARTESIAN_POINT ( 'NONE',  ( 152.5238248654052313, 3.889087296526011706, -3.889087296526011706 ) ) ;
#29127 = CARTESIAN_POINT ( 'NONE',  ( -5.412658773652739619, 3.124999999999975131, -165.1830127018922383 ) ) ;
#29128 = CARTESIAN_POINT ( 'NONE',  ( 6.000000000000000888, 1.743066579297358182E-13, -48.66367513459482552 ) ) ;
#29129 = CARTESIAN_POINT ( 'NONE',  ( 24.18750000000015277, 0.8284271247463557142, 2.000000000000031530 ) ) ;
#29130 = CARTESIAN_POINT ( 'NONE',  ( -6.350852961085760029, -1.281975124255709124E-13, -116.6250000000000000 ) ) ;
#29131 =( LENGTH_UNIT ( ) NAMED_UNIT ( * ) SI_UNIT ( .MILLI., .METRE. ) );
#29132 = EDGE_CURVE ( 'NONE', #7780, #9966, #8531, .T. ) ;
#29133 = CARTESIAN_POINT ( 'NONE',  ( 4.763139720814407951, -2.749999999999988454, -105.5000000000000426 ) ) ;
#29134 = CARTESIAN_POINT ( 'NONE',  ( 135.0000000000000284, -8.936766734253373201, 7.963374800949050147 ) ) ;
#29135 = ORIENTED_EDGE ( 'NONE', *, *, #1328, .T. ) ;
#29136 = CARTESIAN_POINT ( 'NONE',  ( 16.06250000000006040, -2.649519052838238409, 1.097466725451379244 ) ) ;
#29137 = FACE_OUTER_BOUND ( 'NONE', #27437, .T. ) ;
#29138 = LINE ( 'NONE', #7955, #11560 ) ;
#29139 = CARTESIAN_POINT ( 'NONE',  ( 6.000000000000000000, 2.951592740943527306E-14, -150.0863248654052029 ) ) ;
#29140 = ORIENTED_EDGE ( 'NONE', *, *, #3740, .T. ) ;
#29141 = CARTESIAN_POINT ( 'NONE',  ( -3.175426480542816510, -5.500000000000057732, -159.8750000000000284 ) ) ;
#29142 = CARTESIAN_POINT ( 'NONE',  ( 138.8363248654052029, 0.000000000000000000, -5.500000000000005329 ) ) ;
#29143 = CARTESIAN_POINT ( 'NONE',  ( -5.412658773652739619, 3.124999999999975131, -83.31698729810781856 ) ) ;
#29144 = DIRECTION ( 'NONE',  ( -1.000000000000000000, -0.000000000000000000, -0.000000000000000000 ) ) ;
#29145 = ORIENTED_EDGE ( 'NONE', *, *, #1467, .T. ) ;
#29146 = CARTESIAN_POINT ( 'NONE',  ( 115.8363248654051176, 1.414213562373117794, 1.414213562373034527 ) ) ;
#29147 = VERTEX_POINT ( 'NONE', #19814 ) ;
#29148 = CARTESIAN_POINT ( 'NONE',  ( 160.9687500000000000, -2.485281374238585972, 6.000000000000005329 ) ) ;
#29149 = CARTESIAN_POINT ( 'NONE',  ( -7.216878364870328078, 0.000000000000000000, -138.0580127018922099 ) ) ;
#29150 = VERTEX_POINT ( 'NONE', #1683 ) ;
#29151 = CARTESIAN_POINT ( 'NONE',  ( 7.216878364870455975, -6.409875621278545621E-14, -130.4419872981078470 ) ) ;
#29152 = DIRECTION ( 'NONE',  ( 1.734723475976824844E-16, -1.000000000000000000, 0.000000000000000000 ) ) ;
#29153 = LINE ( 'NONE', #5975, #10854 ) ;
#29154 = EDGE_CURVE ( 'NONE', #7308, #27374, #28519, .T. ) ;
#29155 = ORIENTED_EDGE ( 'NONE', *, *, #14160, .F. ) ;
#29156 = CARTESIAN_POINT ( 'NONE',  ( 13.87500000000011013, 1.414213562373312083, -1.414213562373145550 ) ) ;
#29157 = CARTESIAN_POINT ( 'NONE',  ( 6.000000000000000888, 1.607695154586715303, -135.5966878364870354 ) ) ;
#29158 = CARTESIAN_POINT ( 'NONE',  ( 3.464101615137852974, 5.999999999999884537, -148.3363248654051461 ) ) ;
#29159 = CARTESIAN_POINT ( 'NONE',  ( -5.999999999999919176, 1.607695154586804565, -56.40331216351302857 ) ) ;
#29160 = CARTESIAN_POINT ( 'NONE',  ( -6.000000000000007105, -1.607695154586655129, -107.8466878364870354 ) ) ;
#29161 = CARTESIAN_POINT ( 'NONE',  ( 0.9999999929836370649, -15.13506141816058914, -8.789165735397107326 ) ) ;
#29162 = CARTESIAN_POINT ( 'NONE',  ( -3.608439182435052128, -6.250000000000110134, -69.44198729810781856 ) ) ;
#29163 = FILL_AREA_STYLE_COLOUR ( '', #23404 ) ;
#29164 = CARTESIAN_POINT ( 'NONE',  ( -5.999999999999963585, 1.780251999655701777E-13, -64.41367513459483973 ) ) ;
#29165 = CARTESIAN_POINT ( 'NONE',  ( 0.000000000000000000, 5.999999999999977796, -103.2113248654052455 ) ) ;
#29166 = CARTESIAN_POINT ( 'NONE',  ( 6.000000000000000888, 1.743066579297358182E-13, -98.16367513459481131 ) ) ;
#29167 = EDGE_CURVE ( 'NONE', #30104, #30382, #12944, .T. ) ;
#29168 = CARTESIAN_POINT ( 'NONE',  ( -3.175426480542816510, 5.499999999999865885, -127.3750000000000000 ) ) ;
#29169 = ADVANCED_FACE ( 'NONE', ( #24724 ), #13100, .T. ) ;
#29170 = VECTOR ( 'NONE', #20982, 1000.000000000000000 ) ;
#29171 = CARTESIAN_POINT ( 'NONE',  ( 108.5863248654051034, 1.414213562373173305, -1.414213562373145550 ) ) ;
#29172 = CARTESIAN_POINT ( 'NONE',  ( 104.7401757384972996, -0.9317532982612999337, -1.616718326172621456 ) ) ;
#29173 = ORIENTED_EDGE ( 'NONE', *, *, #16847, .F. ) ;
#29174 = CARTESIAN_POINT ( 'NONE',  ( 139.5000000000000284, -9.165151389911669000, -8.500000000000007105 ) ) ;
#29175 = CARTESIAN_POINT ( 'NONE',  ( 1.110223024625164183E-16, -2.000000000000012879, -1.776356839400262692E-15 ) ) ;
#29176 = CARTESIAN_POINT ( 'NONE',  ( 141.0000000000000284, -19.99999999999998934, 5.000000000000004441 ) ) ;
#29177 = CARTESIAN_POINT ( 'NONE',  ( 112.4761751345946692, 0.8284271247462654530, 2.000000000000151879 ) ) ;
#29178 = CARTESIAN_POINT ( 'NONE',  ( 6.000000000000000888, 1.743066579297358182E-13, -102.0863248654051887 ) ) ;
#29179 = ORIENTED_EDGE ( 'NONE', *, *, #5791, .T. ) ;
#29180 = CARTESIAN_POINT ( 'NONE',  ( 112.1247167782376124, -1.849990392679579099, 1.110223024625156540E-13 ) ) ;
#29181 = CYLINDRICAL_SURFACE ( 'NONE', #746, 5.500000000000000000 ) ;
#29182 = CARTESIAN_POINT ( 'NONE',  ( 2.775557561562891351E-14, -6.250000000000061284, -99.31698729810783277 ) ) ;
#29183 = CARTESIAN_POINT ( 'NONE',  ( 155.9136751345948539, 0.000000000000000000, -5.500000000000005329 ) ) ;
#29184 = CARTESIAN_POINT ( 'NONE',  ( 114.3749999999998010, -1.767766952966154381, 1.767766952966653982 ) ) ;
#29185 = CARTESIAN_POINT ( 'NONE',  ( 140.9019117484303933, -11.80382349685853427, 4.000000000000003553 ) ) ;
#29186 =( BOUNDED_CURVE ( )  B_SPLINE_CURVE ( 2, ( #24595, #29664, #15900, #3545, #24760, #3700, #27353, #27049, #22926 ),
 .UNSPECIFIED., .F., .F. ) 
 B_SPLINE_CURVE_WITH_KNOTS ( ( 3, 2, 2, 2, 3 ),
 ( 0.8861111111111111827, 0.8870370370370370683, 0.8888888888888888395, 0.8907407407407407218, 0.8916666666666666075 ),
 .UNSPECIFIED. ) 
 CURVE ( )  GEOMETRIC_REPRESENTATION_ITEM ( )  RATIONAL_B_SPLINE_CURVE ( ( 0.9330127018922194093, 0.9330127018922234061, 1.000000000000000000, 0.8660254037844388186, 1.000000000000000000, 0.8660254037844388186, 1.000000000000000000, 0.9330127018922234061, 0.9330127018922194093 ) ) 
 REPRESENTATION_ITEM ( '' )  );
#29187 = ORIENTED_EDGE ( 'NONE', *, *, #16469, .T. ) ;
#29188 = CARTESIAN_POINT ( 'NONE',  ( 9.875000000000023093, 1.414213562373201061, -1.414213562373090038 ) ) ;
#29189 = CARTESIAN_POINT ( 'NONE',  ( 0.000000000000000000, -5.999999999999991118, -82.96132486540518869 ) ) ;
#29190 = CARTESIAN_POINT ( 'NONE',  ( -3.175426480542816510, 5.499999999999865885, -52.37500000000002842 ) ) ;
#29191 = ADVANCED_FACE ( 'NONE', ( #20742 ), #4490, .T. ) ;
#29192 = CARTESIAN_POINT ( 'NONE',  ( 140.8199251345947687, -2.278174593052058938, -5.499999999999964473 ) ) ;
#29193 = DIRECTION ( 'NONE',  ( 1.000000000000000000, -5.551115123125773458E-17, -1.260129944081490338E-35 ) ) ;
#29194 = CARTESIAN_POINT ( 'NONE',  ( 5.412658773652739619, 3.124999999999988898, -77.18301270189220986 ) ) ;
#29195 = DIRECTION ( 'NONE',  ( 1.000000000000000000, -5.551115123125773458E-17, -1.260129944081490338E-35 ) ) ;
#29196 = CARTESIAN_POINT ( 'NONE',  ( 149.2351497308104342, 3.535533905932725318, -3.535533905932725318 ) ) ;
#29197 = CARTESIAN_POINT ( 'NONE',  ( 154.4136751345948539, 0.000000000000000000, -5.500000000000005329 ) ) ;
#29198 =( LENGTH_UNIT ( ) NAMED_UNIT ( * ) SI_UNIT ( .MILLI., .METRE. ) );
#29199 = LINE ( 'NONE', #8160, #27518 ) ;
#29200 = CARTESIAN_POINT ( 'NONE',  ( 0.000000000000000000, 0.000000000000000000, 0.000000000000000000 ) ) ;
#29201 = ADVANCED_FACE ( 'NONE', ( #27615 ), #142, .T. ) ;
#29202 = CARTESIAN_POINT ( 'NONE',  ( -3.175426480542816066, 5.499999999999865885, -128.8750000000000284 ) ) ;
#29203 = TOROIDAL_SURFACE ( 'NONE', #11102, 1.000000000000000000, 0.5000000000000000000 ) ;
#29204 = CARTESIAN_POINT ( 'NONE',  ( -3.464101615137725076, 5.999999999999979572, -101.5863248654052029 ) ) ;
#29205 = AXIS2_PLACEMENT_3D ( 'NONE', #2260, #18557, #8868 ) ;
#29206 = CARTESIAN_POINT ( 'NONE',  ( -6.350852961085760029, -1.281975124255709124E-13, -61.12500000000000000 ) ) ;
#29207 = DIRECTION ( 'NONE',  ( 1.000000000000000000, 0.000000000000000000, 0.000000000000000000 ) ) ;
#29208 = CARTESIAN_POINT ( 'NONE',  ( 4.763139720814407951, -2.749999999999988454, -59.00000000000004974 ) ) ;
#29209 = ORIENTED_EDGE ( 'NONE', *, *, #18783, .T. ) ;
#29210 = CARTESIAN_POINT ( 'NONE',  ( 145.8750000000000284, 0.000000000000000000, 6.000000000000005329 ) ) ;
#29211 = CARTESIAN_POINT ( 'NONE',  ( 159.0000000000000284, -19.99999999999998934, 3.000000000000002665 ) ) ;
#29212 = CARTESIAN_POINT ( 'NONE',  ( 16.31250000000011369, -0.8284271247460552878, 1.999999999999971800 ) ) ;
#29213 = VECTOR ( 'NONE', #15915, 1000.000000000000000 ) ;
#29214 = CARTESIAN_POINT ( 'NONE',  ( 114.8363248654050324, 1.414213562373090038, 1.414213562373034527 ) ) ;
#29215 = CARTESIAN_POINT ( 'NONE',  ( 111.6872167782374135, 1.849990392679562001, 0.7662911109079489913 ) ) ;
#29216 = ORIENTED_EDGE ( 'NONE', *, *, #16516, .F. ) ;
#29217 = CARTESIAN_POINT ( 'NONE',  ( 144.0937500000000000, 6.000000000000005329, 2.485281374238585972 ) ) ;
#29218 = CARTESIAN_POINT ( 'NONE',  ( 161.1201765630156615, -0.6312603797374088943, 5.593606079993166169 ) ) ;
#29219 = B_SPLINE_CURVE_WITH_KNOTS ( 'NONE', 3,
 ( #23739, #21435, #10215, #17137, #16990, #26314, #367, #9756, #5270, #2967 ),
 .UNSPECIFIED., .F., .F.,
 ( 4, 2, 2, 2, 4 ),
 ( -1.043662239764700441E-05, 0.0005703011627235046472, 0.001151038947844656339, 0.001731776732965803478, 0.002312514518086950834 ),
 .UNSPECIFIED. ) ;
#29220 = EDGE_LOOP ( 'NONE', ( #23421, #24666, #24239, #16458 ) ) ;
#29221 = CARTESIAN_POINT ( 'NONE',  ( -6.350852961085760029, -1.281975124255709124E-13, -148.1250000000000284 ) ) ;
#29222 = CARTESIAN_POINT ( 'NONE',  ( 16.37500000000008527, -1.414213562373090038, 1.414213562373034527 ) ) ;
#29223 = ORIENTED_EDGE ( 'NONE', *, *, #26734, .T. ) ;
#29224 = CARTESIAN_POINT ( 'NONE',  ( -3.608439182435052128, -6.250000000000110134, -147.4419872981078470 ) ) ;
#29225 = CARTESIAN_POINT ( 'NONE',  ( -4.763139720814407951, -2.750000000000016431, -73.00000000000001421 ) ) ;
#29226 = ADVANCED_FACE ( 'NONE', ( #6591 ), #30092, .F. ) ;
#29227 = CARTESIAN_POINT ( 'NONE',  ( 13.25000000000015099, 1.873492889145123019, -1.873492889144956486 ) ) ;
#29228 = EDGE_CURVE ( 'NONE', #4337, #2765, #1250, .T. ) ;
#29229 = CARTESIAN_POINT ( 'NONE',  ( -7.216878364870328078, 0.000000000000000000, -91.55801270189225249 ) ) ;
#29230 = CARTESIAN_POINT ( 'NONE',  ( 0.000000000000000000, 0.000000000000000000, 0.000000000000000000 ) ) ;
#29231 = CARTESIAN_POINT ( 'NONE',  ( 147.9300748654052313, 2.278174593051764951, -5.500000000000262013 ) ) ;
#29232 = CARTESIAN_POINT ( 'NONE',  ( -3.464101615137725076, 5.999999999999979572, -98.58632486540518869 ) ) ;
#29233 = DIRECTION ( 'NONE',  ( 1.000000000000000000, -5.551115123125773458E-17, -1.260129944081490338E-35 ) ) ;
#29234 = CARTESIAN_POINT ( 'NONE',  ( -6.350852961085760029, -1.281975124255709124E-13, -158.6250000000000284 ) ) ;
#29235 = CARTESIAN_POINT ( 'NONE',  ( 17.46132486540527395, 5.551115123125782702E-14, -2.500000000000002220 ) ) ;
#29236 = CARTESIAN_POINT ( 'NONE',  ( -4.763139720814407951, 2.749999999999946709, -146.7500000000000568 ) ) ;
#29237 = CARTESIAN_POINT ( 'NONE',  ( 3.464101615137852974, 5.999999999999884537, -76.91367513459478289 ) ) ;
#29238 = FILL_AREA_STYLE ('',( #30139 ) ) ;
#29239 = CARTESIAN_POINT ( 'NONE',  ( 4.763139720814407951, -2.749999999999988454, -86.00000000000001421 ) ) ;
#29240 = STYLED_ITEM ( 'NONE', ( #22639 ), #4002 ) ;
#29241 = CARTESIAN_POINT ( 'NONE',  ( 19.46132486540541606, 1.665334536937734811E-13, -2.500000000000002220 ) ) ;
#29242 = CARTESIAN_POINT ( 'NONE',  ( -4.763139720814407951, 2.749999999999946709, -85.25000000000004263 ) ) ;
#29243 = CARTESIAN_POINT ( 'NONE',  ( 151.1398502691896510, -3.535533905932752852, 3.535533905932725318 ) ) ;
#29244 = LINE ( 'NONE', #22366, #28897 ) ;
#29245 = CARTESIAN_POINT ( 'NONE',  ( -3.464101615137757051, -5.999999999999979572, -108.5863248654051887 ) ) ;
#29246 = MECHANICAL_DESIGN_GEOMETRIC_PRESENTATION_REPRESENTATION (  '', ( #25839 ), #18515 ) ;
#29248 = CARTESIAN_POINT ( 'NONE',  ( -3.464101615137757051, -5.999999999999979572, -149.6636751345947971 ) ) ;
#29247 = AXIS2_PLACEMENT_3D ( 'NONE', #28711, #3072, #23981 ) ;
#29249 = CARTESIAN_POINT ( 'NONE',  ( 21.31250000000010658, -0.8284271247460552878, 1.999999999999971800 ) ) ;
#29250 = CARTESIAN_POINT ( 'NONE',  ( 111.8363248654050039, 1.414213562373201061, 1.414213562373367594 ) ) ;
#29251 = FACE_OUTER_BOUND ( 'NONE', #10843, .T. ) ;
#29252 = CARTESIAN_POINT ( 'NONE',  ( -5.196152422706601826, 2.999999999999975131, -138.9613248654052313 ) ) ;
#29253 = ORIENTED_EDGE ( 'NONE', *, *, #8455, .T. ) ;
#29254 = DIRECTION ( 'NONE',  ( 1.000000000000000000, 0.000000000000000000, -0.000000000000000000 ) ) ;
#29255 =( NAMED_UNIT ( * ) PLANE_ANGLE_UNIT ( ) SI_UNIT ( $, .RADIAN. ) );
#29256 = CARTESIAN_POINT ( 'NONE',  ( 110.0386751345947971, 0.000000000000000000, -1.999999999999779732 ) ) ;
#29257 = PRESENTATION_LAYER_ASSIGNMENT (  '', '', ( #28299 ) ) ;
#29258 = CARTESIAN_POINT ( 'NONE',  ( 119.3752832217622313, 1.849990392679523588, 0.000000000000000000 ) ) ;
#29259 = CARTESIAN_POINT ( 'NONE',  ( -5.196152422706573404, -3.000000000000002665, -116.2113248654052029 ) ) ;
#29260 = ORIENTED_EDGE ( 'NONE', *, *, #2719, .T. ) ;
#29261 = CIRCLE ( 'NONE', #11156, 14.99999999999998579 ) ;
#29262 = ORIENTED_EDGE ( 'NONE', *, *, #10133, .F. ) ;
#29263 = CARTESIAN_POINT ( 'NONE',  ( -4.763139720814407951, 2.749999999999946709, -104.7500000000000142 ) ) ;
#29264 = CYLINDRICAL_SURFACE ( 'NONE', #1835, 2.000000000000012879 ) ;
#29265 = ADVANCED_FACE ( 'NONE', ( #13707 ), #20203, .T. ) ;
#29266 = CARTESIAN_POINT ( 'NONE',  ( -5.412658773652684552, -3.125000000000099920, -116.9330127018922667 ) ) ;
#29267 = VERTEX_POINT ( 'NONE', #14169 ) ;
#29268 = LINE ( 'NONE', #24829, #14705 ) ;
#29269 = CARTESIAN_POINT ( 'NONE',  ( 105.3749999999999005, -1.767766952966320915, 1.767766952966431937 ) ) ;
#29270 = CARTESIAN_POINT ( 'NONE',  ( 0.000000000000000000, 10.00000000000000888, -5.000000000000004441 ) ) ;
#29271 = CARTESIAN_POINT ( 'NONE',  ( 7.216878364870455975, -6.409875621278545621E-14, -54.80801270189220986 ) ) ;
#29272 = EDGE_LOOP ( 'NONE', ( #29739, #18091, #7669, #7175, #17961, #13338, #10377, #24362, #6495, #7775, #23985, #17254, #17972, #13855, #30193, #2435, #19794, #5924, #14506, #5275, #29135, #2442, #4929, #3818, #9050, #16220, #23779, #5283, #13977, #11380, #7270, #14832, #12099, #20105, #22252, #26696, #25923, #3157, #6416, #20407, #5355, #13918, #24785, #29546, #3510, #21749, #13227, #10067, #4719, #28851, #4489, #19260, #24966, #21784, #2489, #12583, #6281, #1504, #26425, #27839, #1274, #21141, #5205, #9653, #13163, #19555, #27560, #15375, #26293, #11465, #20372, #22432, #19446, #2543, #17028, #26216, #4193, #18100, #29075, #12283, #11346, #13536, #23016, #25136, #425, #3308, #1849, #9312, #12888, #25075, #28440, #607, #18329, #18242, #26327, #21480, #27565, #19980, #30216, #4769, #29658, #27590, #25499, #580, #24882, #3676, #6196, #24926, #2687, #3343, #18623, #10481, #16965, #11252, #19633, #24322, #24736, #29511, #25189, #21986, #24960, #16162, #11220, #30037, #6090, #23032, #5232, #21145, #6455, #27073, #18297, #30067, #14450, #8790, #28050, #27795, #6082, #13202, #28801, #19047, #22461, #3044, #9802, #17454, #6707, #2395, #6120, #5054, #30313, #26247, #27406, #23067, #23663, #10451, #27123, #5961, #1110, #19756, #4542, #16862, #10599, #22941, #22112, #19878, #21450, #11061, #21372, #13439, #10848, #8967, #23277, #1308, #11714, #23943, #7924, #19076, #28401, #13239, #14230, #30342, #14332, #8815 ) ) ;
#29273 = CARTESIAN_POINT ( 'NONE',  ( 0.000000000000000000, 5.999999999999977796, -167.7113248654051745 ) ) ;
#29274 = CARTESIAN_POINT ( 'NONE',  ( -3.464101615137757051, -5.999999999999979572, -119.6636751345947829 ) ) ;
#29275 = CARTESIAN_POINT ( 'NONE',  ( 0.000000000000000000, 0.000000000000000000, 0.000000000000000000 ) ) ;
#29276 = CARTESIAN_POINT ( 'NONE',  ( 155.7113248654052313, 5.500000000000005329, 0.000000000000000000 ) ) ;
#29277 = CARTESIAN_POINT ( 'NONE',  ( -2.775557561562891351E-14, -5.500000000000115463, -173.2500000000000284 ) ) ;
#29278 = CARTESIAN_POINT ( 'NONE',  ( 120.0624999999998721, 2.500000000000114575, 1.035533905932869425 ) ) ;
#29279 = CARTESIAN_POINT ( 'NONE',  ( -0.08386379889025598333, -15.14278526281355219, 7.883982414521697457 ) ) ;
#29280 = CARTESIAN_POINT ( 'NONE',  ( 2.775557561562891351E-14, -6.250000000000061284, -170.6830127018922383 ) ) ;
#29281 = CARTESIAN_POINT ( 'NONE',  ( -0.9345383689551277628, -9.130923262089552850, 4.000000000000004441 ) ) ;
#29282 = CARTESIAN_POINT ( 'NONE',  ( 3.175426480543072749, -5.500000000000105693, -114.6250000000000000 ) ) ;
#29283 = CARTESIAN_POINT ( 'NONE',  ( 105.9613248654051461, 5.551115123125782702E-14, 2.000000000000001776 ) ) ;
#29284 = CARTESIAN_POINT ( 'NONE',  ( 3.175426480543072749, -5.500000000000105693, -104.1250000000000142 ) ) ;
#29285 =( BOUNDED_CURVE ( )  B_SPLINE_CURVE ( 2, ( #28103, #14044, #9082, #6773, #26110, #166, #2329, #23382, #14485 ),
 .UNSPECIFIED., .F., .F. ) 
 B_SPLINE_CURVE_WITH_KNOTS ( ( 3, 2, 2, 2, 3 ),
 ( 0.6718750000000000000, 0.6796875000000000000, 0.6875000000000000000, 0.6953125000000000000, 0.7031250000000000000 ),
 .UNSPECIFIED. ) 
 CURVE ( )  GEOMETRIC_REPRESENTATION_ITEM ( )  RATIONAL_B_SPLINE_CURVE ( ( 1.000000000000000000, 0.9238795325112867385, 1.000000000000000000, 0.9238795325112867385, 1.000000000000000000, 0.9238795325112867385, 1.000000000000000000, 0.9238795325112867385, 1.000000000000000000 ) ) 
 REPRESENTATION_ITEM ( '' )  );
#29286 = CYLINDRICAL_SURFACE ( 'NONE', #6770, 2.000000000000012879 ) ;
#29287 = CARTESIAN_POINT ( 'NONE',  ( 5.196152422706629359, -2.999999999999988898, -87.21132486540523132 ) ) ;
#29288 = LINE ( 'NONE', #27582, #19585 ) ;
#29289 = CARTESIAN_POINT ( 'NONE',  ( 135.0000000000000284, -8.656969940506323624, 7.548343266826465836 ) ) ;
#29290 = EDGE_LOOP ( 'NONE', ( #17752, #1201, #8393, #25620 ) ) ;
#29291 = CARTESIAN_POINT ( 'NONE',  ( 13.37500000000013678, 1.665334536937734811E-13, -2.649519052838444910 ) ) ;
#29292 = CARTESIAN_POINT ( 'NONE',  ( 159.0000000000000284, -59.99999999999980105, -3.000000000000002665 ) ) ;
#29293 = CARTESIAN_POINT ( 'NONE',  ( 161.4375000000000284, -4.242640687119298093, -4.242640687119298093 ) ) ;
#29294 = MECHANICAL_DESIGN_GEOMETRIC_PRESENTATION_REPRESENTATION (  '', ( #21485 ), #7265 ) ;
#29295 = CARTESIAN_POINT ( 'NONE',  ( 111.3127832217622171, 1.849990392679501827, -0.7662911109077087390 ) ) ;
#29296 = VERTEX_POINT ( 'NONE', #14016 ) ;
#29297 = CARTESIAN_POINT ( 'NONE',  ( 4.763139720814407951, -2.749999999999988454, -161.0000000000000284 ) ) ;
#29298 = CARTESIAN_POINT ( 'NONE',  ( 149.9136751345948539, 0.000000000000000000, -5.500000000000005329 ) ) ;
#29299 = CARTESIAN_POINT ( 'NONE',  ( 109.8122167782375840, 0.7662911109078588412, 1.849990392679772278 ) ) ;
#29300 = EDGE_CURVE ( 'NONE', #17631, #956, #4401, .T. ) ;
#29301 = CARTESIAN_POINT ( 'NONE',  ( 5.412658773652712085, -3.125000000000086153, -81.06698729810779014 ) ) ;
#29302 = LINE ( 'NONE', #10915, #17085 ) ;
#29303 = ORIENTED_EDGE ( 'NONE', *, *, #6855, .F. ) ;
#29304 = CARTESIAN_POINT ( 'NONE',  ( 24.57756289884257939, 1.057017408232165723, -2.193898053493716471 ) ) ;
#29305 = VECTOR ( 'NONE', #5827, 1000.000000000000000 ) ;
#29306 = ORIENTED_EDGE ( 'NONE', *, *, #10950, .T. ) ;
#29307 = ORIENTED_EDGE ( 'NONE', *, *, #30327, .F. ) ;
#29308 = CARTESIAN_POINT ( 'NONE',  ( 156.4687500000000284, -2.485281374238585972, 6.000000000000005329 ) ) ;
#29309 = EDGE_CURVE ( 'NONE', #17836, #19610, #23652, .T. ) ;
#29310 = VERTEX_POINT ( 'NONE', #21048 ) ;
#29311 = CARTESIAN_POINT ( 'NONE',  ( 5.412658773652739619, 3.124999999999988898, -122.8169872981078612 ) ) ;
#29312 = CARTESIAN_POINT ( 'NONE',  ( -4.763139720814407951, 2.749999999999946709, -169.2500000000000000 ) ) ;
#29313 = CARTESIAN_POINT ( 'NONE',  ( 6.000000000000000888, -1.607695154586752384, -167.2306624327026157 ) ) ;
#29314 = FILL_AREA_STYLE ('',( #24867 ) ) ;
#29315 = EDGE_LOOP ( 'NONE', ( #13418, #4147, #28241, #24678 ) ) ;
#29316 = CARTESIAN_POINT ( 'NONE',  ( 8.673617379884035472E-16, -15.46117127753089449, -5.976030864474088489 ) ) ;
#29317 = CARTESIAN_POINT ( 'NONE',  ( 0.000000000000000000, 5.999999999999977796, -163.7886751345948255 ) ) ;
#29318 = CARTESIAN_POINT ( 'NONE',  ( 0.000000000000000000, 5.999999999999977796, -56.71132486540520290 ) ) ;
#29319 = DIRECTION ( 'NONE',  ( -1.000000000000000000, -1.665334536937723717E-16, 0.000000000000000000 ) ) ;
#29320 = CARTESIAN_POINT ( 'NONE',  ( 3.464101615137757051, -5.999999999999979572, -54.91367513459480421 ) ) ;
#29321 = CARTESIAN_POINT ( 'NONE',  ( 8.673617379884035472E-16, -14.27031434886951544, -8.428912904374499249 ) ) ;
#29322 = CARTESIAN_POINT ( 'NONE',  ( 115.3752832217622881, 1.849990392679579099, 0.000000000000000000 ) ) ;
#29323 = CARTESIAN_POINT ( 'NONE',  ( -3.608439182435115633, 6.249999999999965361, -65.44198729810786119 ) ) ;
#29324 = CARTESIAN_POINT ( 'NONE',  ( -3.608439182435052128, -6.250000000000110134, -57.44198729810781856 ) ) ;
#29325 = CARTESIAN_POINT ( 'NONE',  ( 5.196152422706629359, -2.999999999999988898, -120.7886751345948539 ) ) ;
#29326 = CARTESIAN_POINT ( 'NONE',  ( 135.0000000000001137, 4.403472173772889242, 3.650336322691055013 ) ) ;
#29327 = CARTESIAN_POINT ( 'NONE',  ( 148.0386751345948539, -5.500000000000005329, 0.000000000000000000 ) ) ;
#29328 = CARTESIAN_POINT ( 'NONE',  ( 6.000000000000000888, -1.859271017917181981E-14, -120.6636751345948255 ) ) ;
#29329 = CARTESIAN_POINT ( 'NONE',  ( -6.350852961085760029, -1.281975124255709124E-13, -131.6250000000000284 ) ) ;
#29331 = CARTESIAN_POINT ( 'NONE',  ( -5.999999999999963585, -1.487416814333745711E-14, -166.4136751345948539 ) ) ;
#29330 = COLOUR_RGB ( '', 0.40784314, 0.44705882, 0.49803922) ;
#29332 = VERTEX_POINT ( 'NONE', #13550 ) ;
#29333 = CARTESIAN_POINT ( 'NONE',  ( 23.68750000000009948, 2.649519052838538613, 1.097466725451559322 ) ) ;
#29334 = CARTESIAN_POINT ( 'NONE',  ( -5.999999999999963585, 0.000000000000000000, -179.9136751345948255 ) ) ;
#29335 = CARTESIAN_POINT ( 'NONE',  ( 6.000000000000000000, 2.951592740943527306E-14, -155.1636751345948539 ) ) ;
#29336 = CARTESIAN_POINT ( 'NONE',  ( 124.9999999999999432, -71.00000000000001421, 4.000000000000003553 ) ) ;
#29337 = ORIENTED_EDGE ( 'NONE', *, *, #23927, .F. ) ;
#29338 = CARTESIAN_POINT ( 'NONE',  ( 114.4997167782375413, 1.308140751793696044, -1.308140751793640533 ) ) ;
#29339 = PRESENTATION_STYLE_ASSIGNMENT (( #15728 ) ) ;
#29340 = ADVANCED_FACE ( 'NONE', ( #11553 ), #21195, .T. ) ;
#29341 = CARTESIAN_POINT ( 'NONE',  ( 2.775557561562891351E-14, 6.250000000000033751, -118.0669872981078328 ) ) ;
#29342 = CARTESIAN_POINT ( 'NONE',  ( 6.000000000000000888, -1.607695154586752384, -173.2306624327026441 ) ) ;
#29343 = CARTESIAN_POINT ( 'NONE',  ( 155.7261751345948539, -3.889087296526011706, -3.889087296526011706 ) ) ;
#29344 = CARTESIAN_POINT ( 'NONE',  ( 116.1874999999999005, 1.035533905932839227, 2.500000000000205169 ) ) ;
#29345 = CARTESIAN_POINT ( 'NONE',  ( 140.8038234968598488, -11.90191174842882660, 4.000000000000003553 ) ) ;
#29346 = CARTESIAN_POINT ( 'NONE',  ( 144.4687500000000568, -2.485281374238585972, 6.000000000000005329 ) ) ;
#29347 = EDGE_CURVE ( 'NONE', #8327, #17555, #26554, .T. ) ;
#29348 = ADVANCED_FACE ( 'NONE', ( #18303 ), #23204, .F. ) ;
#29349 = CARTESIAN_POINT ( 'NONE',  ( 159.9871598483856587, -11.17259796798583515, 4.379265499705882192 ) ) ;
#29350 = CARTESIAN_POINT ( 'NONE',  ( 4.763139720814407951, 2.750000000000002665, -49.75000000000001421 ) ) ;
#29351 = CARTESIAN_POINT ( 'NONE',  ( 140.4449251345948539, -5.500000000000012434, 2.278174593052012309 ) ) ;
#29352 = CARTESIAN_POINT ( 'NONE',  ( 0.000000000000000000, -5.999999999999991118, -59.53867513459481842 ) ) ;
#29353 = DIRECTION ( 'NONE',  ( -7.147005652999508048E-36, 5.642372883946980038E-36, 1.000000000000000000 ) ) ;
#29354 = CARTESIAN_POINT ( 'NONE',  ( 3.608439182435180470, 6.249999999999982236, -75.55801270189225249 ) ) ;
#29355 = CARTESIAN_POINT ( 'NONE',  ( 136.0000000000000284, -8.798545334315230448, -8.160000000000007248 ) ) ;
#29356 = CARTESIAN_POINT ( 'NONE',  ( 151.2038997308104058, 2.071067811865468400, 4.999999999999989342 ) ) ;
#29357 = DIRECTION ( 'NONE',  ( 1.000000000000000000, -5.551115123125773458E-17, -1.260129944081490338E-35 ) ) ;
#29358 = CARTESIAN_POINT ( 'NONE',  ( 104.1872167782373708, -1.849990392679351725, -0.7662911109074682647 ) ) ;
#29359 =( NAMED_UNIT ( * ) PLANE_ANGLE_UNIT ( ) SI_UNIT ( $, .RADIAN. ) );
#29360 = CARTESIAN_POINT ( 'NONE',  ( -5.196152422706601826, 2.999999999999975131, -104.4613248654052171 ) ) ;
#29361 = CARTESIAN_POINT ( 'NONE',  ( 3.175426480543072749, 5.499999999999865885, -132.1250000000000284 ) ) ;
#29362 = DIRECTION ( 'NONE',  ( -1.000000000000000000, -1.665334536937731113E-16, 1.526556658859586792E-16 ) ) ;
#29363 = CARTESIAN_POINT ( 'NONE',  ( -1.000000000000000888, -10.00000000000000888, -4.000000000000003553 ) ) ;
#29364 = EDGE_LOOP ( 'NONE', ( #13393, #26181, #13079, #3312, #9955 ) ) ;
#29365 = CARTESIAN_POINT ( 'NONE',  ( 4.763139720814407951, -2.749999999999988454, -65.00000000000000000 ) ) ;
#29366 = CARTESIAN_POINT ( 'NONE',  ( -4.763139720814407951, -2.750000000000016431, -58.00000000000004974 ) ) ;
#29367 = FACE_OUTER_BOUND ( 'NONE', #22502, .T. ) ;
#29368 = ORIENTED_EDGE ( 'NONE', *, *, #2547, .F. ) ;
#29369 = CARTESIAN_POINT ( 'NONE',  ( 107.8749999999999858, 1.767766952966431937, -1.767766952966209892 ) ) ;
#29370 = CARTESIAN_POINT ( 'NONE',  ( 143.9062500000000284, 6.000000000000005329, -2.485281374238556218 ) ) ;
#29371 = DIRECTION ( 'NONE',  ( 5.551115123125785167E-17, -1.000000000000000000, -8.881784197001256268E-16 ) ) ;
#29372 = CARTESIAN_POINT ( 'NONE',  ( 15.06250000000016165, 2.000000000000151879, 0.8284271247461152399 ) ) ;
#29373 = EDGE_CURVE ( 'NONE', #22801, #25470, #3995, .T. ) ;
#29374 = DIRECTION ( 'NONE',  ( -7.147005652999508048E-36, 5.642372883946980038E-36, 1.000000000000000000 ) ) ;
#29375 =( BOUNDED_SURFACE ( )  B_SPLINE_SURFACE ( 1, 2, ( 
 ( #3188, #20102, #7954, #21806, #17824, #6112, #5491, #3046, #12464, #14896, #12612, #752, #10592, #17365, #26680, #21954, #888, #10139, #5643, #19507, #28838, #15047, #24393, #3337, #22106, #10437, #19790, #8096, #17513, #26825, #22254, #5789, #24538, #3488, #19943, #20396, #16140, #6404, #18578, #25285, #4257, #23179, #20555, #27898, #8731, #27742, #13677, #2123, #23018, #15525, #18118, #20715, #15839, #22865, #18421, #3795, #3939, #29906, #13525, #15985, #1803, #11526, #9182, #4103, #25445, #24846, #4409, #25138, #1964, #6260, #20867, #27287, #30063, #13834, #11051, #30218, #13225, #22565, #9033, #1655, #11368, #1495, #11208, #13369, #8886, #17974, #10907, #20262, #29608, #15681, #8569, #18273, #24989, #27586, #6564, #30371, #28503, #2858, #18729, #28052, #4568, #23771, #23485, #116, #9339, #21023, #7470, #25768, #12279, #16884, #21623, #555, #19170, #12131, #26203, #18881, #5154, #2423, #16442, #5006, #9644, #14146, #6872, #14569, #11837, #23917, #28202, #9945, #16737, #26061, #19321, #11988, #16295, #21173, #25615, #14438, #13994, #2704, #23333, #7179, #21475, #16591, #14289, #9791, #2276, #4713, #21319, #4861, #7329, #23630, #11680, #7024, #25913, #2565, #402, #261, #19036, #28354, #28643, #28797, #7759, #1424, #711, #18055, #24921, #12424, #3871, #26352, #29682, #27370, #8333, #10833, #25070, #15451, #17171, #24777, #1264, #5302, #3003, #21767, #11129, #7614, #15608, #14715, #3147, #6192, #20022, #3723, #13152, #17024, #22641, #24058, #26493, #5449, #20186, #10097, #15763, #13299, #19468, #1580, #12571, #8654, #4027, #17743, #29538, #13446, #22491, #21916, #8495, #10675, #29369, #27067, #6032, #17901, #27218, #10986, #20331, #22794, #1734, #11457, #16221, #25533, #29838, #14074, #9111, #23410, #23555, #9420, #18506, #9264, #11291, #7102, #1886, #4641, #2355, #16073, #18808, #14217, #28133, #11758, #6654, #30299, #20477, #27829, #18357, #2054, #22947, #18201, #18657, #27976, #20646, #16522, #25374, #27519, #21103, #25691, #13603, #32, #25844, #29992, #8968, #6496, #6950, #13759, #23106 ),
 ( #16368, #6797, #20801, #8816, #15919, #4791, #20949, #4496, #13919, #2493, #25220, #23262, #27674, #2203, #11608, #4188, #24276, #3082, #24137, #28578, #16814, #17103, #28878, #12505, #26580, #7259, #11918, #7546, #21844, #26284, #792, #19249, #26429, #14507, #14367, #19546, #12213, #14645, #23992, #14938, #17256, #16956, #7407, #21247, #2935, #188, #9571, #12352, #18965, #2785, #21703, #28282, #7695, #5233, #10176, #5385, #7842, #19401, #639, #12058, #4936, #5532, #16668, #25991, #23705, #2639, #21401, #334, #10022, #26136, #28429, #19104, #14792, #28724, #9727, #480, #5082, #23847, #21553, #9874, #8140, #20302, #10799, #17405, #8299, #29498, #19987, #8463, #3840, #6158, #22456, #17709, #10483, #19691, #5680, #12803, #20150, #22298, #29338, #17870, #10637, #27187, #22609, #27339, #13119, #29648, #15727, #10952, #3223, #1544, #29033, #15575, #15092, #15251, #7999, #8614, #27033, #18022, #13268, #5998, #15418, #12650, #21992, #3377, #24743, #926, #22144, #10325, #24582, #3684, #24430, #1390, #1229, #17557, #1087, #19833, #29180, #26874, #5836, #3530, #12961, #14036, #11253, #22908, #13569, #27634, #20763, #7069, #16335, #6913, #11418, #29951, #30261, #11721, #25656, #9380, #20443, #25035, #30109, #4607, #9073, #23374, #2009, #9226, #6613, #27479, #2320, #25332, #27788, #6764, #28094, #30413, #18466, #20604, #16185, #21064, #25492, #1850, #4457, #16035, #22759, #29802, #8780, #3990, #13412, #11568, #11097, #8931, #2168, #4307, #13883, #23223, #1700, #18616, #13726, #27938, #18167, #18774, #23068, #20913, #15883, #6456, #25182, #4148, #18321, #21117, #23865, #19270, #2805, #28450, #11776, #4952, #25552, #2509, #23428, #7118, #6967, #23279, #23720, #14387, #4658, #12231, #52, #2221, #7423, #349, #18674, #16831, #21569, #16386, #2373, #11625, #12079, #9441, #18824, #28150, #9280, #26152, #21417, #20969, #14240, #4811, #501, #5100, #9742, #14526, #16538, #9895, #25864, #23573, #28593, #28301, #11937, #4514, #13937, #21265, #30319, #204, #9590, #18979, #7281, #16685, #26007, #29358, #21865 ) ),
 .UNSPECIFIED., .F., .F., .T. ) 
 B_SPLINE_SURFACE_WITH_KNOTS ( ( 2, 2 ),
 ( 3, 2, 2, 2, 2, 2, 2, 2, 2, 2, 2, 2, 2, 2, 2, 2, 2, 2, 2, 2, 2, 2, 2, 2, 2, 2, 2, 2, 2, 2, 2, 2, 2, 2, 2, 2, 2, 2, 2, 2, 2, 2, 2, 2, 2, 2, 2, 2, 2, 2, 2, 2, 2, 2, 2, 2, 2, 2, 2, 2, 2, 2, 2, 2, 2, 2, 2, 2, 2, 2, 2, 2, 2, 2, 2, 2, 2, 2, 2, 2, 2, 2, 2, 2, 2, 2, 2, 2, 2, 2, 2, 2, 2, 2, 2, 2, 2, 2, 2, 2, 2, 2, 2, 2, 2, 2, 2, 2, 2, 2, 2, 2, 2, 2, 2, 2, 2, 2, 2, 2, 2, 2, 2, 2, 2, 2, 2, 2, 2, 2, 2, 2, 3 ),
 ( 0.000000000000000000, 1.000000000000000000 ),
 ( 0.000000000000000000, 0.007352941176470588133, 0.01470588235294117627, 0.02205882352941176613, 0.02941176470588235253, 0.03676470588235294240, 0.04411764705882353227, 0.05147058823529411520, 0.05882352941176470507, 0.06617647058823529493, 0.07352941176470588480, 0.08088235294117647467, 0.08823529411764706454, 0.09558823529411764053, 0.1029411764705882304, 0.1102941176470588203, 0.1176470588235294101, 0.1250000000000000000, 0.1323529411764705899, 0.1397058823529411797, 0.1470588235294117696, 0.1544117647058823595, 0.1617647058823529493, 0.1691176470588235392, 0.1764705882352941291, 0.1838235294117647189, 0.1911764705882352811, 0.1985294117647058709, 0.2058823529411764608, 0.2132352941176470507, 0.2205882352941176405, 0.2279411764705882304, 0.2352941176470588203, 0.2426470588235294101, 0.2500000000000000000, 0.2573529411764705621, 0.2647058823529411797, 0.2720588235294117418, 0.2794117647058823595, 0.2867647058823529216, 0.2941176470588235392, 0.3014705882352941013, 0.3088235294117647189, 0.3161764705882352811, 0.3235294117647058987, 0.3308823529411764608, 0.3382352941176470784, 0.3455882352941176405, 0.3529411764705882582, 0.3602941176470588203, 0.3676470588235294379, 0.3750000000000000000, 0.3823529411764705621, 0.3897058823529411797, 0.3970588235294117418, 0.4044117647058823595, 0.4117647058823529216, 0.4191176470588235392, 0.4264705882352941013, 0.4338235294117647189, 0.4411764705882352811, 0.4485294117647058987, 0.4558823529411764608, 0.4632352941176470784, 0.4705882352941176405, 0.4779411764705882582, 0.4852941176470588203, 0.4926470588235294379, 0.5000000000000000000, 0.5073529411764705621, 0.5147058823529411242, 0.5220588235294117974, 0.5294117647058823595, 0.5367647058823529216, 0.5441176470588234837, 0.5514705882352941568, 0.5588235294117647189, 0.5661764705882352811, 0.5735294117647058432, 0.5808823529411765163, 0.5882352941176470784, 0.5955882352941176405, 0.6029411764705882026, 0.6102941176470588758, 0.6176470588235294379, 0.6250000000000000000, 0.6323529411764705621, 0.6397058823529411242, 0.6470588235294117974, 0.6544117647058823595, 0.6617647058823529216, 0.6691176470588234837, 0.6764705882352941568, 0.6838235294117647189, 0.6911764705882352811, 0.6985294117647058432, 0.7058823529411765163, 0.7132352941176470784, 0.7205882352941176405, 0.7279411764705882026, 0.7352941176470588758, 0.7426470588235294379, 0.7500000000000000000, 0.7573529411764705621, 0.7647058823529411242, 0.7720588235294117974, 0.7794117647058823595, 0.7867647058823529216, 0.7941176470588234837, 0.8014705882352941568, 0.8088235294117647189, 0.8161764705882352811, 0.8235294117647058432, 0.8308823529411765163, 0.8382352941176470784, 0.8455882352941176405, 0.8529411764705882026, 0.8602941176470588758, 0.8676470588235294379, 0.8750000000000000000, 0.8823529411764705621, 0.8897058823529411242, 0.8970588235294117974, 0.9044117647058823595, 0.9117647058823529216, 0.9191176470588234837, 0.9264705882352941568, 0.9338235294117647189, 0.9411764705882352811, 0.9485294117647058432, 0.9558823529411765163, 0.9632352941176470784, 0.9705882352941176405 ),
 .UNSPECIFIED. ) 
 GEOMETRIC_REPRESENTATION_ITEM ( )  RATIONAL_B_SPLINE_SURFACE ( (
 ( 1.000000000000000000, 0.9238795325112867385, 1.000000000000000000, 0.9238795325112867385, 1.000000000000000000, 0.9238795325112867385, 1.000000000000000000, 0.9238795325112867385, 1.000000000000000000, 0.9238795325112867385, 1.000000000000000000, 0.9238795325112867385, 1.000000000000000000, 0.9238795325112867385, 1.000000000000000000, 0.9238795325112867385, 1.000000000000000000, 0.9238795325112867385, 1.000000000000000000, 0.9238795325112867385, 1.000000000000000000, 0.9238795325112867385, 1.000000000000000000, 0.9238795325112867385, 1.000000000000000000, 0.9238795325112867385, 1.000000000000000000, 0.9238795325112867385, 1.000000000000000000, 0.9238795325112867385, 1.000000000000000000, 0.9238795325112867385, 1.000000000000000000, 0.9238795325112867385, 1.000000000000000000, 0.9238795325112867385, 1.000000000000000000, 0.9238795325112867385, 1.000000000000000000, 0.9238795325112867385, 1.000000000000000000, 0.9238795325112867385, 1.000000000000000000, 0.9238795325112867385, 1.000000000000000000, 0.9238795325112867385, 1.000000000000000000, 0.9238795325112867385, 1.000000000000000000, 0.9238795325112867385, 1.000000000000000000, 0.9238795325112867385, 1.000000000000000000, 0.9238795325112867385, 1.000000000000000000, 0.9238795325112867385, 1.000000000000000000, 0.9238795325112867385, 1.000000000000000000, 0.9238795325112867385, 1.000000000000000000, 0.9238795325112867385, 1.000000000000000000, 0.9238795325112867385, 1.000000000000000000, 0.9238795325112867385, 1.000000000000000000, 0.9238795325112867385, 1.000000000000000000, 0.9238795325112867385, 1.000000000000000000, 0.9238795325112867385, 1.000000000000000000, 0.9238795325112867385, 1.000000000000000000, 0.9238795325112867385, 1.000000000000000000, 0.9238795325112867385, 1.000000000000000000, 0.9238795325112867385, 1.000000000000000000, 0.9238795325112867385, 1.000000000000000000, 0.9238795325112867385, 1.000000000000000000, 0.9238795325112867385, 1.000000000000000000, 0.9238795325112867385, 1.000000000000000000, 0.9238795325112867385, 1.000000000000000000, 0.9238795325112867385, 1.000000000000000000, 0.9238795325112867385, 1.000000000000000000, 0.9238795325112867385, 1.000000000000000000, 0.9238795325112867385, 1.000000000000000000, 0.9238795325112867385, 1.000000000000000000, 0.9238795325112867385, 1.000000000000000000, 0.9238795325112867385, 1.000000000000000000, 0.9238795325112867385, 1.000000000000000000, 0.9238795325112867385, 1.000000000000000000, 0.9238795325112867385, 1.000000000000000000, 0.9238795325112867385, 1.000000000000000000, 0.9238795325112867385, 1.000000000000000000, 0.9238795325112867385, 1.000000000000000000, 0.9238795325112867385, 1.000000000000000000, 0.9238795325112867385, 1.000000000000000000, 0.9238795325112867385, 1.000000000000000000, 0.9238795325112867385, 1.000000000000000000, 0.9238795325112867385, 1.000000000000000000, 0.9238795325112867385, 1.000000000000000000, 0.9238795325112867385, 1.000000000000000000, 0.9238795325112867385, 1.000000000000000000, 0.9238795325112867385, 1.000000000000000000, 0.9238795325112867385, 1.000000000000000000, 0.9238795325112867385, 1.000000000000000000, 0.9238795325112867385, 1.000000000000000000, 0.9238795325112867385, 1.000000000000000000, 0.9238795325112867385, 1.000000000000000000, 0.9238795325112867385, 1.000000000000000000, 0.9238795325112867385, 1.000000000000000000, 0.9238795325112867385, 1.000000000000000000, 0.9238795325112867385, 1.000000000000000000, 0.9238795325112867385, 1.000000000000000000, 0.9238795325112867385, 1.000000000000000000, 0.9238795325112867385, 1.000000000000000000, 0.9238795325112867385, 1.000000000000000000, 0.9238795325112867385, 1.000000000000000000, 0.9238795325112867385, 1.000000000000000000, 0.9238795325112867385, 1.000000000000000000, 0.9238795325112867385, 1.000000000000000000, 0.9238795325112867385, 1.000000000000000000, 0.9238795325112867385, 1.000000000000000000, 0.9238795325112867385, 1.000000000000000000, 0.9238795325112867385, 1.000000000000000000, 0.9238795325112867385, 1.000000000000000000, 0.9238795325112867385, 1.000000000000000000, 0.9238795325112867385, 1.000000000000000000, 0.9238795325112867385, 1.000000000000000000, 0.9238795325112867385, 1.000000000000000000, 0.9238795325112867385, 1.000000000000000000, 0.9238795325112867385, 1.000000000000000000, 0.9238795325112867385, 1.000000000000000000, 0.9238795325112867385, 1.000000000000000000, 0.9238795325112867385, 1.000000000000000000, 0.9238795325112867385, 1.000000000000000000, 0.9238795325112867385, 1.000000000000000000, 0.9238795325112867385, 1.000000000000000000, 0.9238795325112867385, 1.000000000000000000, 0.9238795325112867385, 1.000000000000000000, 0.9238795325112867385, 1.000000000000000000, 0.9238795325112867385, 1.000000000000000000, 0.9238795325112867385, 1.000000000000000000, 0.9238795325112867385, 1.000000000000000000, 0.9238795325112867385, 1.000000000000000000, 0.9238795325112867385, 1.000000000000000000, 0.9238795325112867385, 1.000000000000000000, 0.9238795325112867385, 1.000000000000000000, 0.9238795325112867385, 1.000000000000000000, 0.9238795325112867385, 1.000000000000000000, 0.9238795325112867385, 1.000000000000000000, 0.9238795325112867385, 1.000000000000000000, 0.9238795325112867385, 1.000000000000000000, 0.9238795325112867385, 1.000000000000000000, 0.9238795325112867385, 1.000000000000000000, 0.9238795325112867385, 1.000000000000000000, 0.9238795325112867385, 1.000000000000000000, 0.9238795325112867385, 1.000000000000000000, 0.9238795325112867385, 1.000000000000000000, 0.9238795325112867385, 1.000000000000000000, 0.9238795325112867385, 1.000000000000000000, 0.9238795325112867385, 1.000000000000000000, 0.9238795325112867385, 1.000000000000000000, 0.9238795325112867385, 1.000000000000000000, 0.9238795325112867385, 1.000000000000000000, 0.9238795325112867385, 1.000000000000000000, 0.9238795325112867385, 1.000000000000000000, 0.9238795325112867385, 1.000000000000000000, 0.9238795325112867385, 1.000000000000000000),
 ( 1.000000000000000000, 0.9238795325112867385, 1.000000000000000000, 0.9238795325112867385, 1.000000000000000000, 0.9238795325112867385, 1.000000000000000000, 0.9238795325112867385, 1.000000000000000000, 0.9238795325112867385, 1.000000000000000000, 0.9238795325112867385, 1.000000000000000000, 0.9238795325112867385, 1.000000000000000000, 0.9238795325112867385, 1.000000000000000000, 0.9238795325112867385, 1.000000000000000000, 0.9238795325112867385, 1.000000000000000000, 0.9238795325112867385, 1.000000000000000000, 0.9238795325112867385, 1.000000000000000000, 0.9238795325112867385, 1.000000000000000000, 0.9238795325112867385, 1.000000000000000000, 0.9238795325112867385, 1.000000000000000000, 0.9238795325112867385, 1.000000000000000000, 0.9238795325112867385, 1.000000000000000000, 0.9238795325112867385, 1.000000000000000000, 0.9238795325112867385, 1.000000000000000000, 0.9238795325112867385, 1.000000000000000000, 0.9238795325112867385, 1.000000000000000000, 0.9238795325112867385, 1.000000000000000000, 0.9238795325112867385, 1.000000000000000000, 0.9238795325112867385, 1.000000000000000000, 0.9238795325112867385, 1.000000000000000000, 0.9238795325112867385, 1.000000000000000000, 0.9238795325112867385, 1.000000000000000000, 0.9238795325112867385, 1.000000000000000000, 0.9238795325112867385, 1.000000000000000000, 0.9238795325112867385, 1.000000000000000000, 0.9238795325112867385, 1.000000000000000000, 0.9238795325112867385, 1.000000000000000000, 0.9238795325112867385, 1.000000000000000000, 0.9238795325112867385, 1.000000000000000000, 0.9238795325112867385, 1.000000000000000000, 0.9238795325112867385, 1.000000000000000000, 0.9238795325112867385, 1.000000000000000000, 0.9238795325112867385, 1.000000000000000000, 0.9238795325112867385, 1.000000000000000000, 0.9238795325112867385, 1.000000000000000000, 0.9238795325112867385, 1.000000000000000000, 0.9238795325112867385, 1.000000000000000000, 0.9238795325112867385, 1.000000000000000000, 0.9238795325112867385, 1.000000000000000000, 0.9238795325112867385, 1.000000000000000000, 0.9238795325112867385, 1.000000000000000000, 0.9238795325112867385, 1.000000000000000000, 0.9238795325112867385, 1.000000000000000000, 0.9238795325112867385, 1.000000000000000000, 0.9238795325112867385, 1.000000000000000000, 0.9238795325112867385, 1.000000000000000000, 0.9238795325112867385, 1.000000000000000000, 0.9238795325112867385, 1.000000000000000000, 0.9238795325112867385, 1.000000000000000000, 0.9238795325112867385, 1.000000000000000000, 0.9238795325112867385, 1.000000000000000000, 0.9238795325112867385, 1.000000000000000000, 0.9238795325112867385, 1.000000000000000000, 0.9238795325112867385, 1.000000000000000000, 0.9238795325112867385, 1.000000000000000000, 0.9238795325112867385, 1.000000000000000000, 0.9238795325112867385, 1.000000000000000000, 0.9238795325112867385, 1.000000000000000000, 0.9238795325112867385, 1.000000000000000000, 0.9238795325112867385, 1.000000000000000000, 0.9238795325112867385, 1.000000000000000000, 0.9238795325112867385, 1.000000000000000000, 0.9238795325112867385, 1.000000000000000000, 0.9238795325112867385, 1.000000000000000000, 0.9238795325112867385, 1.000000000000000000, 0.9238795325112867385, 1.000000000000000000, 0.9238795325112867385, 1.000000000000000000, 0.9238795325112867385, 1.000000000000000000, 0.9238795325112867385, 1.000000000000000000, 0.9238795325112867385, 1.000000000000000000, 0.9238795325112867385, 1.000000000000000000, 0.9238795325112867385, 1.000000000000000000, 0.9238795325112867385, 1.000000000000000000, 0.9238795325112867385, 1.000000000000000000, 0.9238795325112867385, 1.000000000000000000, 0.9238795325112867385, 1.000000000000000000, 0.9238795325112867385, 1.000000000000000000, 0.9238795325112867385, 1.000000000000000000, 0.9238795325112867385, 1.000000000000000000, 0.9238795325112867385, 1.000000000000000000, 0.9238795325112867385, 1.000000000000000000, 0.9238795325112867385, 1.000000000000000000, 0.9238795325112867385, 1.000000000000000000, 0.9238795325112867385, 1.000000000000000000, 0.9238795325112867385, 1.000000000000000000, 0.9238795325112867385, 1.000000000000000000, 0.9238795325112867385, 1.000000000000000000, 0.9238795325112867385, 1.000000000000000000, 0.9238795325112867385, 1.000000000000000000, 0.9238795325112867385, 1.000000000000000000, 0.9238795325112867385, 1.000000000000000000, 0.9238795325112867385, 1.000000000000000000, 0.9238795325112867385, 1.000000000000000000, 0.9238795325112867385, 1.000000000000000000, 0.9238795325112867385, 1.000000000000000000, 0.9238795325112867385, 1.000000000000000000, 0.9238795325112867385, 1.000000000000000000, 0.9238795325112867385, 1.000000000000000000, 0.9238795325112867385, 1.000000000000000000, 0.9238795325112867385, 1.000000000000000000, 0.9238795325112867385, 1.000000000000000000, 0.9238795325112867385, 1.000000000000000000, 0.9238795325112867385, 1.000000000000000000, 0.9238795325112867385, 1.000000000000000000, 0.9238795325112867385, 1.000000000000000000, 0.9238795325112867385, 1.000000000000000000, 0.9238795325112867385, 1.000000000000000000, 0.9238795325112867385, 1.000000000000000000, 0.9238795325112867385, 1.000000000000000000, 0.9238795325112867385, 1.000000000000000000, 0.9238795325112867385, 1.000000000000000000, 0.9238795325112867385, 1.000000000000000000, 0.9238795325112867385, 1.000000000000000000, 0.9238795325112867385, 1.000000000000000000, 0.9238795325112867385, 1.000000000000000000, 0.9238795325112867385, 1.000000000000000000, 0.9238795325112867385, 1.000000000000000000, 0.9238795325112867385, 1.000000000000000000, 0.9238795325112867385, 1.000000000000000000, 0.9238795325112867385, 1.000000000000000000, 0.9238795325112867385, 1.000000000000000000, 0.9238795325112867385, 1.000000000000000000, 0.9238795325112867385, 1.000000000000000000, 0.9238795325112867385, 1.000000000000000000, 0.9238795325112867385, 1.000000000000000000, 0.9238795325112867385, 1.000000000000000000, 0.9238795325112867385, 1.000000000000000000) ) ) 
 REPRESENTATION_ITEM ( '' )  SURFACE ( )  );
#29376 = VERTEX_POINT ( 'NONE', #10273 ) ;
#29377 = CARTESIAN_POINT ( 'NONE',  ( -5.999999999999956479, -1.607695154586745057, -122.2693375672974128 ) ) ;
#29378 = EDGE_LOOP ( 'NONE', ( #27597, #14366, #14728, #14259 ) ) ;
#29379 = ADVANCED_FACE ( 'NONE', ( #17049 ), #28376, .F. ) ;
#29380 = CARTESIAN_POINT ( 'NONE',  ( 0.000000000000000000, 5.499999999999991118, -148.5000000000000284 ) ) ;
#29381 =( GEOMETRIC_REPRESENTATION_CONTEXT ( 3 ) GLOBAL_UNCERTAINTY_ASSIGNED_CONTEXT ( ( #6065 ) ) GLOBAL_UNIT_ASSIGNED_CONTEXT ( ( #12500, #11090, #20755 ) ) REPRESENTATION_CONTEXT ( 'NONE', 'WORKASPACE' ) );
#29382 = CARTESIAN_POINT ( 'NONE',  ( 7.216878364870455975, -6.409875621278545621E-14, -47.94198729810783277 ) ) ;
#29383 = CARTESIAN_POINT ( 'NONE',  ( 17.37500000000011369, -1.414213562372979016, 1.414213562373034527 ) ) ;
#29384 = ORIENTED_EDGE ( 'NONE', *, *, #6922, .F. ) ;
#29385 = CARTESIAN_POINT ( 'NONE',  ( 2.775557561562891351E-14, -6.250000000000061284, -150.3169872981078186 ) ) ;
#29386 = CARTESIAN_POINT ( 'NONE',  ( -3.175426480542816510, 5.499999999999865885, -73.37500000000000000 ) ) ;
#29387 = CARTESIAN_POINT ( 'NONE',  ( 5.412658773652739619, 3.124999999999988898, -96.68301270189222407 ) ) ;
#29388 = CARTESIAN_POINT ( 'NONE',  ( -4.763139720814407951, -2.750000000000016431, -152.5000000000000284 ) ) ;
#29389 = CARTESIAN_POINT ( 'NONE',  ( -5.196552517144552574, -9.698180938751621127, -21.97571210926416541 ) ) ;
#29390 = DIRECTION ( 'NONE',  ( -7.147005652999508048E-36, 5.642372883946980038E-36, 1.000000000000000000 ) ) ;
#29391 = FACE_OUTER_BOUND ( 'NONE', #6696, .T. ) ;
#29392 = CARTESIAN_POINT ( 'NONE',  ( -6.000000000000007105, -1.607695154586655129, -91.34668783648704959 ) ) ;
#29393 = CYLINDRICAL_SURFACE ( 'NONE', #1946, 6.000000000000000888 ) ;
#29394 = CARTESIAN_POINT ( 'NONE',  ( -4.763139720814407951, 2.749999999999946709, -158.7500000000000568 ) ) ;
#29395 = CARTESIAN_POINT ( 'NONE',  ( -3.175426480542816510, 5.499999999999865885, -145.3750000000000000 ) ) ;
#29396 = CARTESIAN_POINT ( 'NONE',  ( 19.46132486540541606, 1.665334536937734811E-13, -2.500000000000002220 ) ) ;
#29397 = UNCERTAINTY_MEASURE_WITH_UNIT (LENGTH_MEASURE( 1.000000000000000082E-05 ), #18830, 'distance_accuracy_value', 'NONE');
#29398 = TOROIDAL_SURFACE ( 'NONE', #960, 12.50000000000000178, 0.5000000000000000000 ) ;
#29399 = CARTESIAN_POINT ( 'NONE',  ( -4.763139720814407951, -2.750000000000016431, -89.50000000000002842 ) ) ;
#29400 = CARTESIAN_POINT ( 'NONE',  ( 24.49999999999999289, 0.6095397824026904665, 2.424553825690067388 ) ) ;
#29401 = CARTESIAN_POINT ( 'NONE',  ( 3.175426480543072749, 5.499999999999865885, -81.12500000000002842 ) ) ;
#29402 = CIRCLE ( 'NONE', #7808, 0.5000000000000004441 ) ;
#29403 = DIRECTION ( 'NONE',  ( 0.000000000000000000, 0.000000000000000000, -1.000000000000000000 ) ) ;
#29404 = CARTESIAN_POINT ( 'NONE',  ( 161.3006082692931500, -4.487120878302232718, -3.700106666589778825 ) ) ;
#29405 = CARTESIAN_POINT ( 'NONE',  ( 114.3363248654051176, -1.414213562373256572, -1.414213562372923505 ) ) ;
#29406 = CARTESIAN_POINT ( 'NONE',  ( 6.000000000000000888, -1.859271017917181981E-14, -125.1636751345948397 ) ) ;
#29407 = EDGE_CURVE ( 'NONE', #21222, #24216, #10720, .T. ) ;
#29408 = CARTESIAN_POINT ( 'NONE',  ( 120.5622167782374419, 1.849990392679652151, -0.7662911109075283278 ) ) ;
#29409 = CARTESIAN_POINT ( 'NONE',  ( 6.000000000000000888, -3.330669073875464691E-16, -7.560779664488942560E-35 ) ) ;
#29410 = ADVANCED_FACE ( 'NONE', ( #12156 ), #428, .T. ) ;
#29411 = ORIENTED_EDGE ( 'NONE', *, *, #22351, .T. ) ;
#29412 = CARTESIAN_POINT ( 'NONE',  ( 5.999999999999949374, 1.607695154586804565, -91.51933756729745539 ) ) ;
#29413 = CARTESIAN_POINT ( 'NONE',  ( 5.999999999999949374, 1.607695154586804565, -73.51933756729744118 ) ) ;
#29414 = CARTESIAN_POINT ( 'NONE',  ( 145.5074251345947971, 2.278174593051996322, -5.500000000000026645 ) ) ;
#29415 = CARTESIAN_POINT ( 'NONE',  ( 118.6877832217621460, -0.7662911109076785410, 1.849990392679712103 ) ) ;
#29416 = CARTESIAN_POINT ( 'NONE',  ( 25.00000000000013500, 2.000000000000279332, -5.551115123125782702E-14 ) ) ;
#29417 = VERTEX_POINT ( 'NONE', #7784 ) ;
#29418 = ORIENTED_EDGE ( 'NONE', *, *, #22757, .T. ) ;
#29419 = CARTESIAN_POINT ( 'NONE',  ( 3.175426480543072749, -5.500000000000105693, -95.12500000000002842 ) ) ;
#29420 = AXIS2_PLACEMENT_3D ( 'NONE', #12591, #865, #28968 ) ;
#29421 = CARTESIAN_POINT ( 'NONE',  ( 5.412658773652739619, 3.124999999999988898, -111.6830127018922383 ) ) ;
#29422 = VERTEX_POINT ( 'NONE', #16904 ) ;
#29423 = CYLINDRICAL_SURFACE ( 'NONE', #27908, 6.000000000000000888 ) ;
#29424 = VECTOR ( 'NONE', #7596, 1000.000000000000000 ) ;
#29425 = CARTESIAN_POINT ( 'NONE',  ( 135.0000000000000284, -9.047800747817552391, 7.500000000000007105 ) ) ;
#29426 = CARTESIAN_POINT ( 'NONE',  ( 21.35117513459487171, 2.500000000000024425, 1.035533905932629173 ) ) ;
#29427 = CARTESIAN_POINT ( 'NONE',  ( -3.608439182435052128, -6.250000000000110134, -52.30801270189225249 ) ) ;
#29428 = EDGE_LOOP ( 'NONE', ( #26953, #6698, #12766, #26983 ) ) ;
#29429 = CARTESIAN_POINT ( 'NONE',  ( 135.5000000000000000, -24.99999999999999289, -8.000000000000007105 ) ) ;
#29430 = CARTESIAN_POINT ( 'NONE',  ( 6.000000000000000888, -1.859271017917181981E-14, -136.5863248654051745 ) ) ;
#29431 = CARTESIAN_POINT ( 'NONE',  ( 119.2113248654050466, -1.999999999999946265, 2.220446049250313081E-13 ) ) ;
#29432 = CARTESIAN_POINT ( 'NONE',  ( -4.763139720814407951, -2.750000000000016431, -173.5000000000000000 ) ) ;
#29433 = CARTESIAN_POINT ( 'NONE',  ( 117.4374999999997584, -2.499999999999844569, 1.035533905932929599 ) ) ;
#29434 = CARTESIAN_POINT ( 'NONE',  ( 10.08632486540522777, -1.767766952966209892, 1.767766952966431937 ) ) ;
#29435 = CARTESIAN_POINT ( 'NONE',  ( -7.216878364870328078, 0.000000000000000000, -159.0580127018922383 ) ) ;
#29436 = CARTESIAN_POINT ( 'NONE',  ( -3.464101615137725076, 5.999999999999979572, -48.16367513459483973 ) ) ;
#29437 = CARTESIAN_POINT ( 'NONE',  ( -4.763139720814407951, 2.749999999999946709, -106.2500000000000142 ) ) ;
#29438 = CARTESIAN_POINT ( 'NONE',  ( 13.53867513459486283, 1.110223024625156540E-13, 2.499999999999946709 ) ) ;
#29439 = CARTESIAN_POINT ( 'NONE',  ( -4.763139720814407951, 2.749999999999946709, -107.7500000000000142 ) ) ;
#29440 = CARTESIAN_POINT ( 'NONE',  ( 5.196152422706629359, 3.000000000000002665, -152.0386751345948539 ) ) ;
#29441 = CARTESIAN_POINT ( 'NONE',  ( 140.9136751345948539, 0.000000000000000000, -5.500000000000005329 ) ) ;
#29442 = CARTESIAN_POINT ( 'NONE',  ( 5.196152422706629359, 3.000000000000002665, -145.4613248654052029 ) ) ;
#29443 = CARTESIAN_POINT ( 'NONE',  ( 16.12500000000019540, -2.649519052838111843, -5.551115123125782702E-14 ) ) ;
#29444 = CARTESIAN_POINT ( 'NONE',  ( 3.464101615137757051, -5.999999999999979572, -90.33632486540521711 ) ) ;
#29445 = AXIS2_PLACEMENT_3D ( 'NONE', #24902, #3849, #5846 ) ;
#29446 = CARTESIAN_POINT ( 'NONE',  ( 110.9377832217620323, -1.849990392679411677, -0.7662911109076485650 ) ) ;
#29447 = ADVANCED_FACE ( 'NONE', ( #7204 ), #14460, .T. ) ;
#29448 = ORIENTED_EDGE ( 'NONE', *, *, #3740, .F. ) ;
#29449 = CARTESIAN_POINT ( 'NONE',  ( 0.000000000000000000, 5.499999999999991118, -160.5000000000000284 ) ) ;
#29450 = CARTESIAN_POINT ( 'NONE',  ( 0.000000000000000000, 5.999999999999977796, -65.71132486540520290 ) ) ;
#29451 = CARTESIAN_POINT ( 'NONE',  ( 108.3747167782376124, -1.665334536937734811E-13, -1.849990392679523588 ) ) ;
#29452 = CARTESIAN_POINT ( 'NONE',  ( 2.775557561562891351E-14, -6.250000000000061284, -82.81698729810781856 ) ) ;
#29453 = CARTESIAN_POINT ( 'NONE',  ( 149.8050748654052313, 5.500000000000012434, 2.278174593052012309 ) ) ;
#29454 = ORIENTED_EDGE ( 'NONE', *, *, #6227, .T. ) ;
#29455 = CARTESIAN_POINT ( 'NONE',  ( 6.000000000000000888, -1.859271017917181981E-14, -125.1636751345948397 ) ) ;
#29456 = CIRCLE ( 'NONE', #17727, 6.000000000000009770 ) ;
#29457 = EDGE_LOOP ( 'NONE', ( #1898, #25699, #9426, #15226 ) ) ;
#29458 = ORIENTED_EDGE ( 'NONE', *, *, #8341, .T. ) ;
#29459 = CARTESIAN_POINT ( 'NONE',  ( 159.2812500000000568, 2.485281374238585972, 6.000000000000005329 ) ) ;
#29460 = CARTESIAN_POINT ( 'NONE',  ( 3.175426480543072749, -5.500000000000105693, -122.1250000000000284 ) ) ;
#29461 =( BOUNDED_CURVE ( )  B_SPLINE_CURVE ( 2, ( #15771, #16227, #4192, #30153, #22954, #1892, #11298, #7268, #28434, #5239, #21108, #21253, #16820, #9578, #2361, #7413, #14224, #26436, #28287, #2940, #14653, #14800, #5086, #11765, #2645, #2792, #39, #28584, #26141, #23997, #7551, #10029, #9880, #23852, #11923, #25849, #7700, #12357, #21707, #645, #17109, #19405, #14512, #28730, #21407, #12219, #18971, #9425, #16528, #16673, #19256, #12064, #14373, #21558, #338, #16961, #486, #5391, #4797, #23561, #4943, #29344, #15422, #27038, #12967, #8145, #931, #10180, #17262, #3231, #10642, #12809, #19838, #1234, #1094, #19992, #13122, #17875, #3536, #20156, #27192, #24283, #10805, #10331, #21851, #17715, #8306, #26881, #3383, #6004, #29184, #5538, #796, #24750, #19696, #17410, #26584, #7849, #3690, #22303, #19551, #15098, #17563, #24142, #22460, #22151, #8004, #5688, #28884, #1396, #29504, #26724, #24434, #8468, #6167, #29038, #21996, #12656, #14943, #10489, #3085, #5842, #15257, #12511, #24587, #7092, #22, #6640, #27963, #18797, #9249, #28123, #14208, #25835, #11746, #6940, #30136, #8955, #16062, #2037, #9409, #18642, #16509, #30289, #4785, #11906, #16658, #2346, #18954, #25981, #182, #4925, #21239, #18347, #23546, #4330, #4484, #6786, #25360, #23250, #16209, #20633, #2486, #9098, #25520, #13749, #23094, #9562, #21091, #29976, #11596, #2189, #28271, #7250, #22936, #1875, #20788, #27661, #16359, #11279, #11443, #13908, #18495, #27815, #20938, #25680, #4628, #14061, #23400, #26706, #5519, #26569, #628, #19239, #19535, #914, #14928, #29020, #9714, #14356, #10012, #28565, #21692, #17244, #2630, #2776, #28713, #12203, #23695, #19389, #26128, #7984, #9865, #24263, #7828, #12050, #7685, #3213, #21392, #14501, #23841, #10163, #17094, #12636, #28869, #21981, #21835, #5372, #21544, #7400, #19678, #10312, #17391, #324, #19095, #23982, #28420, #5074, #26421, #2923, #7534, #16807, #12340, #470, #14780, #16945, #26274, #783, #5224 ),
 .UNSPECIFIED., .F., .T. ) 
 B_SPLINE_CURVE_WITH_KNOTS ( ( 3, 2, 2, 2, 2, 2, 2, 2, 2, 2, 2, 2, 2, 2, 2, 2, 2, 2, 2, 2, 2, 2, 2, 2, 2, 2, 2, 2, 2, 2, 2, 2, 2, 2, 2, 2, 2, 2, 2, 2, 2, 2, 2, 2, 2, 2, 2, 2, 2, 2, 2, 2, 2, 2, 2, 2, 2, 2, 2, 2, 2, 2, 2, 2, 2, 2, 2, 2, 2, 2, 2, 2, 2, 2, 2, 2, 2, 2, 2, 2, 2, 2, 2, 2, 2, 2, 2, 2, 2, 2, 2, 2, 2, 2, 2, 2, 2, 2, 2, 2, 2, 2, 2, 2, 2, 2, 2, 2, 2, 2, 2, 2, 2, 2, 2, 2, 2, 2, 2, 2, 2, 2, 2, 2, 3 ),
 ( 0.05882352941176714062, 0.06617647058823770967, 0.07352941176470828566, 0.08088235294117884777, 0.08823529411764942376, 0.09558823529411997200, 0.1029411764705905480, 0.1102941176470611240, 0.1176470588235316861, 0.1250000000000022482, 0.1323529411764728381, 0.1397058823529434002, 0.1470588235294139623, 0.1544117647058845244, 0.1617647058823551143, 0.1691176470588256764, 0.1764705882352962663, 0.1838235294117668006, 0.1911764705882373350, 0.1985294117647079526, 0.2058823529411784869, 0.2132352941176490768, 0.2205882352941196389, 0.2279411764705902288, 0.2352941176470607632, 0.2426470588235313530, 0.2500000000000018874, 0.2573529411764724495, 0.2647058823529430671, 0.2720588235294135737, 0.2794117647058841913, 0.2867647058823546979, 0.2941176470588253711, 0.3014705882352958777, 0.3088235294117664953, 0.3161764705882370019, 0.3235294117647076195, 0.3308823529411781816, 0.3382352941176487993, 0.3455882352941193059, 0.3529411764705899235, 0.3602941176470604301, 0.3676470588235310477, 0.3750000000000015543, 0.3823529411764721719, 0.3897058823529427340, 0.3970588235294132962, 0.4044117647058838583, 0.4117647058823544204, 0.4191176470588250380, 0.4264705882352955446, 0.4338235294117661622, 0.4411764705882366688, 0.4485294117647072865, 0.4558823529411778486, 0.4632352941176484662, 0.4705882352941189728, 0.4779411764705895904, 0.4852941176470600970, 0.4926470588235307146, 0.5000000000000012212, 0.5073529411764717834, 0.5147058823529422344, 0.5220588235294129076, 0.5294117647058835807, 0.5367647058823540318, 0.5441176470588245939, 0.5514705882352952671, 0.5588235294117658292, 0.5661764705882363913, 0.5735294117647068424, 0.5808823529411775155, 0.5882352941176480776, 0.5955882352941186397, 0.6029411764705892018, 0.6102941176470598750, 0.6176470588235304371, 0.6250000000000008882, 0.6323529411764714503, 0.6397058823529420124, 0.6470588235294126855, 0.6544117647058831366, 0.6617647058823536987, 0.6691176470588242609, 0.6764705882352949340, 0.6838235294117654961, 0.6911764705882359472, 0.6985294117647066203, 0.7058823529411772935, 0.7132352941176478556, 0.7205882352941183067, 0.7279411764705888688, 0.7352941176470595419, 0.7426470588235301040, 0.7500000000000005551, 0.7573529411764711172, 0.7647058823529416793, 0.7720588235294123525, 0.7794117647058829146, 0.7867647058823533657, 0.7941176470588239278, 0.8014705882352946009, 0.8088235294117651630, 0.8161764705882356141, 0.8235294117647061762, 0.8308823529411768494, 0.8382352941176474115, 0.8455882352941180846, 0.8529411764705885357, 0.8602941176470592088, 0.8676470588235297710, 0.8750000000000003331, 0.8823529411764707842, 0.8897058823529413463, 0.8970588235294120194, 0.9044117647058825815, 0.9117647058823530326, 0.9191176470588235947, 0.9264705882352942679, 0.9338235294117648300, 0.9411764705882352811, 0.9485294117647058432, 0.9558823529411765163, 0.9632352941176470784, 0.9705882352941176405 ),
 .UNSPECIFIED. ) 
 CURVE ( )  GEOMETRIC_REPRESENTATION_ITEM ( )  RATIONAL_B_SPLINE_CURVE ( ( 0.9999999999999747979, 0.9238795325113119405, 1.000000000000000000, 0.9238795325112867385, 1.000000000000000000, 0.9238795325112867385, 1.000000000000000000, 0.9238795325112867385, 1.000000000000000000, 0.9238795325112867385, 1.000000000000000000, 0.9238795325112867385, 1.000000000000000000, 0.9238795325112867385, 1.000000000000000000, 0.9238795325112867385, 1.000000000000000000, 0.9238795325112867385, 1.000000000000000000, 0.9238795325112867385, 1.000000000000000000, 0.9238795325112867385, 1.000000000000000000, 0.9238795325112867385, 1.000000000000000000, 0.9238795325112867385, 1.000000000000000000, 0.9238795325112867385, 1.000000000000000000, 0.9238795325112867385, 1.000000000000000000, 0.9238795325112867385, 1.000000000000000000, 0.9238795325112867385, 1.000000000000000000, 0.9238795325112867385, 1.000000000000000000, 0.9238795325112867385, 1.000000000000000000, 0.9238795325112867385, 1.000000000000000000, 0.9238795325112867385, 1.000000000000000000, 0.9238795325112867385, 1.000000000000000000, 0.9238795325112867385, 1.000000000000000000, 0.9238795325112867385, 1.000000000000000000, 0.9238795325112867385, 1.000000000000000000, 0.9238795325112867385, 1.000000000000000000, 0.9238795325112867385, 1.000000000000000000, 0.9238795325112867385, 1.000000000000000000, 0.9238795325112867385, 1.000000000000000000, 0.9238795325112867385, 1.000000000000000000, 0.9238795325112867385, 1.000000000000000000, 0.9238795325112867385, 1.000000000000000000, 0.9238795325112867385, 1.000000000000000000, 0.9238795325112867385, 1.000000000000000000, 0.9238795325112867385, 1.000000000000000000, 0.9238795325112867385, 1.000000000000000000, 0.9238795325112867385, 1.000000000000000000, 0.9238795325112867385, 1.000000000000000000, 0.9238795325112867385, 1.000000000000000000, 0.9238795325112867385, 1.000000000000000000, 0.9238795325112867385, 1.000000000000000000, 0.9238795325112867385, 1.000000000000000000, 0.9238795325112867385, 1.000000000000000000, 0.9238795325112867385, 1.000000000000000000, 0.9238795325112867385, 1.000000000000000000, 0.9238795325112867385, 1.000000000000000000, 0.9238795325112867385, 1.000000000000000000, 0.9238795325112867385, 1.000000000000000000, 0.9238795325112867385, 1.000000000000000000, 0.9238795325112867385, 1.000000000000000000, 0.9238795325112867385, 1.000000000000000000, 0.9238795325112867385, 1.000000000000000000, 0.9238795325112867385, 1.000000000000000000, 0.9238795325112867385, 1.000000000000000000, 0.9238795325112867385, 1.000000000000000000, 0.9238795325112867385, 1.000000000000000000, 0.9238795325112867385, 1.000000000000000000, 0.9238795325112867385, 1.000000000000000000, 0.9238795325112867385, 1.000000000000000000, 0.9238795325112867385, 1.000000000000000000, 0.9238795325112867385, 1.000000000000000000, 0.9238795325112867385, 1.000000000000000000, 0.9238795325112867385, 1.000000000000000000, 0.9238795325112867385, 1.000000000000000000, 0.9238795325112867385, 1.000000000000000000, 0.9238795325112867385, 1.000000000000000000, 0.9238795325112867385, 1.000000000000000000, 0.9238795325112867385, 1.000000000000000000, 0.9238795325112867385, 1.000000000000000000, 0.9238795325112867385, 1.000000000000000000, 0.9238795325112867385, 1.000000000000000000, 0.9238795325112867385, 1.000000000000000000, 0.9238795325112867385, 1.000000000000000000, 0.9238795325112867385, 1.000000000000000000, 0.9238795325112867385, 1.000000000000000000, 0.9238795325112867385, 1.000000000000000000, 0.9238795325112867385, 1.000000000000000000, 0.9238795325112867385, 1.000000000000000000, 0.9238795325112867385, 1.000000000000000000, 0.9238795325112867385, 1.000000000000000000, 0.9238795325112867385, 1.000000000000000000, 0.9238795325112867385, 1.000000000000000000, 0.9238795325112867385, 1.000000000000000000, 0.9238795325112867385, 1.000000000000000000, 0.9238795325112867385, 1.000000000000000000, 0.9238795325112867385, 1.000000000000000000, 0.9238795325112867385, 1.000000000000000000, 0.9238795325112867385, 1.000000000000000000, 0.9238795325112867385, 1.000000000000000000, 0.9238795325112867385, 1.000000000000000000, 0.9238795325112867385, 1.000000000000000000, 0.9238795325112867385, 1.000000000000000000, 0.9238795325112867385, 1.000000000000000000, 0.9238795325112867385, 1.000000000000000000, 0.9238795325112867385, 1.000000000000000000, 0.9238795325112867385, 1.000000000000000000, 0.9238795325112867385, 1.000000000000000000, 0.9238795325112867385, 1.000000000000000000, 0.9238795325112867385, 1.000000000000000000, 0.9238795325112867385, 1.000000000000000000, 0.9238795325112867385, 1.000000000000000000, 0.9238795325112867385, 1.000000000000000000, 0.9238795325112867385, 1.000000000000000000, 0.9238795325112867385, 1.000000000000000000, 0.9238795325112867385, 1.000000000000000000, 0.9238795325112867385, 1.000000000000000000, 0.9238795325112867385, 1.000000000000000000, 0.9238795325112867385, 1.000000000000000000, 0.9238795325112867385, 1.000000000000000000, 0.9238795325112867385, 1.000000000000000000, 0.9238795325112867385, 1.000000000000000000, 0.9238795325112867385, 1.000000000000000000, 0.9238795325112867385, 1.000000000000000000, 0.9238795325112867385, 1.000000000000000000, 0.9238795325112867385, 1.000000000000000000, 0.9238795325112867385, 1.000000000000000000, 0.9238795325112867385, 1.000000000000000000, 0.9238795325112867385, 1.000000000000000000, 0.9238795325112867385, 1.000000000000000000, 0.9238795325112867385, 1.000000000000000000, 0.9238795325112867385, 1.000000000000000000, 0.9238795325112867385, 1.000000000000000000, 0.9238795325112867385, 1.000000000000000000, 0.9238795325112867385, 1.000000000000000000 ) ) 
 REPRESENTATION_ITEM ( '' )  );
#29462 = CARTESIAN_POINT ( 'NONE',  ( 5.412658773652739619, 3.124999999999988898, -135.6830127018922667 ) ) ;
#29463 = ORIENTED_EDGE ( 'NONE', *, *, #28171, .T. ) ;
#29464 = CARTESIAN_POINT ( 'NONE',  ( 150.8511751345948255, -3.889087296526011706, 3.889087296526011706 ) ) ;
#29465 = CARTESIAN_POINT ( 'NONE',  ( 5.412658773652712085, -3.125000000000086153, -120.0669872981078328 ) ) ;
#29466 = CARTESIAN_POINT ( 'NONE',  ( 3.175426480543072749, -5.500000000000105693, -174.6250000000000284 ) ) ;
#29467 = CARTESIAN_POINT ( 'NONE',  ( 153.6636751345948255, 0.000000000000000000, 5.500000000000005329 ) ) ;
#29468 =( REPRESENTATION_RELATIONSHIP ('NONE','NONE', #103, #13689 ) REPRESENTATION_RELATIONSHIP_WITH_TRANSFORMATION ( #6353 )SHAPE_REPRESENTATION_RELATIONSHIP( ) );
#29469 = CARTESIAN_POINT ( 'NONE',  ( -5.196152422706601826, 2.999999999999975131, -47.46132486540521711 ) ) ;
#29470 = AXIS2_PLACEMENT_3D ( 'NONE', #12526, #21568, #10196 ) ;
#29471 = EDGE_LOOP ( 'NONE', ( #26624, #165, #5763, #4255 ) ) ;
#29472 = CARTESIAN_POINT ( 'NONE',  ( 15.62500000000013856, -1.414213562372979016, -1.414213562373145550 ) ) ;
#29473 = FACE_OUTER_BOUND ( 'NONE', #10408, .T. ) ;
#29474 =( BOUNDED_CURVE ( )  B_SPLINE_CURVE ( 2, ( #26942, #15329, #12276, #552, #12721, #26489, #22060, #21619, #9942 ),
 .UNSPECIFIED., .F., .T. ) 
 B_SPLINE_CURVE_WITH_KNOTS ( ( 3, 2, 2, 2, 3 ),
 ( 0.8625000000000012657, 0.8687500000000010214, 0.8750000000000008882, 0.8812500000000006439, 0.8875000000000003997 ),
 .UNSPECIFIED. ) 
 CURVE ( )  GEOMETRIC_REPRESENTATION_ITEM ( )  RATIONAL_B_SPLINE_CURVE ( ( 0.9999999999999851230, 0.9238795325113016155, 1.000000000000000000, 0.9238795325112867385, 1.000000000000000000, 0.9238795325112867385, 1.000000000000000000, 0.9238795325112812984, 1.000000000000005329 ) ) 
 REPRESENTATION_ITEM ( '' )  );
#29475 = CARTESIAN_POINT ( 'NONE',  ( 159.7582345317023567, -12.26499483057044415, -3.655200626169436084 ) ) ;
#29476 = CARTESIAN_POINT ( 'NONE',  ( 5.196152422706629359, -2.999999999999988898, -54.78867513459484684 ) ) ;
#29477 = CIRCLE ( 'NONE', #28488, 6.500000000000016875 ) ;
#29478 = CARTESIAN_POINT ( 'NONE',  ( -5.196152422706573404, -3.000000000000002665, -47.21132486540524553 ) ) ;
#29479 = CARTESIAN_POINT ( 'NONE',  ( 113.8127832217621034, -1.849990392679441875, 0.7662911109079489913 ) ) ;
#29480 = CARTESIAN_POINT ( 'NONE',  ( -3.608439182435052128, -6.250000000000110134, -66.44198729810784698 ) ) ;
#29481 = CARTESIAN_POINT ( 'NONE',  ( -5.412658773652739619, 3.124999999999975131, -56.31698729810785409 ) ) ;
#29482 = EDGE_CURVE ( 'NONE', #24216, #17631, #2590, .T. ) ;
#29483 = CARTESIAN_POINT ( 'NONE',  ( 119.3988248654050039, -0.8284271247460852639, -1.999999999999791278 ) ) ;
#29484 = CARTESIAN_POINT ( 'NONE',  ( -6.000000000000007105, -1.607695154586655129, -64.34668783648703538 ) ) ;
#29485 = DIRECTION ( 'NONE',  ( 1.000000000000000000, 0.000000000000000000, -0.000000000000000000 ) ) ;
#29486 = DIRECTION ( 'NONE',  ( 1.000000000000000000, 0.000000000000000000, 0.000000000000000000 ) ) ;
#29487 = CARTESIAN_POINT ( 'NONE',  ( -4.763139720814407951, 2.749999999999946709, -125.7500000000000284 ) ) ;
#29488 = VECTOR ( 'NONE', #27251, 1000.000000000000000 ) ;
#29489 = AXIS2_PLACEMENT_3D ( 'NONE', #3400, #8482, #27209 ) ;
#29490 = ORIENTED_EDGE ( 'NONE', *, *, #15461, .F. ) ;
#29491 = CARTESIAN_POINT ( 'NONE',  ( -5.999999999999963585, 8.134310703387671600E-14, -119.3363248654052455 ) ) ;
#29492 = CARTESIAN_POINT ( 'NONE',  ( 17.91367513459496408, -1.767766952966209892, -1.767766952966542959 ) ) ;
#29493 = CARTESIAN_POINT ( 'NONE',  ( 0.000000000000000000, 5.999999999999977796, -97.21132486540517448 ) ) ;
#29494 = CARTESIAN_POINT ( 'NONE',  ( 15.91367513459493388, -1.767766952966320915, -1.767766952966542959 ) ) ;
#29495 = CARTESIAN_POINT ( 'NONE',  ( 139.7023502691896510, 0.000000000000000000, -5.000000000000004441 ) ) ;
#29496 = ADVANCED_FACE ( 'NONE', ( #26524 ), #3175, .F. ) ;
#29497 = ORIENTED_EDGE ( 'NONE', *, *, #30127, .T. ) ;
#29498 = CARTESIAN_POINT ( 'NONE',  ( 115.3122167782374845, -0.7662911109077388261, -1.849990392679291551 ) ) ;
#29499 = DIRECTION ( 'NONE',  ( 1.000000000000000000, -5.551115123125773458E-17, -1.260129944081490338E-35 ) ) ;
#29500 = LINE ( 'NONE', #23339, #9225 ) ;
#29501 = CARTESIAN_POINT ( 'NONE',  ( 5.412658773652712085, -3.125000000000086153, -112.5669872981078186 ) ) ;
#29502 = TOROIDAL_SURFACE ( 'NONE', #9414, 14.49999999999999822, 0.5000000000000000000 ) ;
#29503 = CARTESIAN_POINT ( 'NONE',  ( 140.0707155294794006, -11.09459640813432557, -4.575173035329879845 ) ) ;
#29504 = CARTESIAN_POINT ( 'NONE',  ( 113.1249999999998295, 1.767766952966376426, 1.767766952966320915 ) ) ;
#29505 = AXIS2_PLACEMENT_3D ( 'NONE', #5951, #24097, #12917 ) ;
#29506 = ORIENTED_EDGE ( 'NONE', *, *, #7474, .T. ) ;
#29507 = VERTEX_POINT ( 'NONE', #12305 ) ;
#29508 = CARTESIAN_POINT ( 'NONE',  ( 21.71132486540530593, 2.500000000000002220, -1.665334536937734811E-13 ) ) ;
#29509 = CARTESIAN_POINT ( 'NONE',  ( 144.7500000000000568, -6.000000000000005329, 0.000000000000000000 ) ) ;
#29510 = VERTEX_POINT ( 'NONE', #21646 ) ;
#29511 = ORIENTED_EDGE ( 'NONE', *, *, #20597, .T. ) ;
#29512 = DIRECTION ( 'NONE',  ( 1.000000000000000000, 0.000000000000000000, 0.000000000000000000 ) ) ;
#29513 = CARTESIAN_POINT ( 'NONE',  ( 3.175426480543072749, -5.500000000000105693, -50.12500000000001421 ) ) ;
#29514 = DIRECTION ( 'NONE',  ( -0.000000000000000000, -0.000000000000000000, -1.000000000000000000 ) ) ;
#29515 = CARTESIAN_POINT ( 'NONE',  ( 136.4136751345948539, 0.000000000000000000, -5.500000000000005329 ) ) ;
#29516 = CARTESIAN_POINT ( 'NONE',  ( -7.216878364870328078, 0.000000000000000000, -76.55801270189223828 ) ) ;
#29517 = LINE ( 'NONE', #22006, #19226 ) ;
#29518 = CARTESIAN_POINT ( 'NONE',  ( 147.8288997308104342, 4.999999999999989342, -2.071067811865468400 ) ) ;
#29519 = VECTOR ( 'NONE', #22670, 1000.000000000000000 ) ;
#29520 = CARTESIAN_POINT ( 'NONE',  ( 0.000000000000000000, 5.999999999999977796, -177.2886751345948539 ) ) ;
#29521 = CYLINDRICAL_SURFACE ( 'NONE', #23123, 1.000000000000000000 ) ;
#29522 =( BOUNDED_CURVE ( )  B_SPLINE_CURVE ( 2, ( #29431, #15188, #22552, #1485, #26666, #1168, #10576, #1330, #10423 ),
 .UNSPECIFIED., .F., .F. ) 
 B_SPLINE_CURVE_WITH_KNOTS ( ( 3, 2, 2, 2, 3 ),
 ( 0.08823529411764706454, 0.09558823529411764053, 0.1029411764705882304, 0.1102941176470588203, 0.1176470588235294101 ),
 .UNSPECIFIED. ) 
 CURVE ( )  GEOMETRIC_REPRESENTATION_ITEM ( )  RATIONAL_B_SPLINE_CURVE ( ( 1.000000000000000000, 0.9238795325112867385, 1.000000000000000000, 0.9238795325112867385, 1.000000000000000000, 0.9238795325112867385, 1.000000000000000000, 0.9238795325112867385, 1.000000000000000000 ) ) 
 REPRESENTATION_ITEM ( '' )  );
#29523 = EDGE_CURVE ( 'NONE', #17248, #7661, #23273, .T. ) ;
#29524 = FACE_OUTER_BOUND ( 'NONE', #9120, .T. ) ;
#29525 = SURFACE_SIDE_STYLE ('',( #12984 ) ) ;
#29526 = LINE ( 'NONE', #2038, #10866 ) ;
#29527 = CARTESIAN_POINT ( 'NONE',  ( -4.763139720814407951, 2.749999999999946709, -130.2500000000000284 ) ) ;
#29528 = CARTESIAN_POINT ( 'NONE',  ( -5.196152422706601826, 2.999999999999975131, -68.46132486540523132 ) ) ;
#29529 = CARTESIAN_POINT ( 'NONE',  ( 2.775557561562891351E-14, -6.250000000000061284, -146.6830127018922099 ) ) ;
#29530 = DIRECTION ( 'NONE',  ( -7.147005652999508048E-36, 5.642372883946980038E-36, 1.000000000000000000 ) ) ;
#29531 = CARTESIAN_POINT ( 'NONE',  ( 5.196152422706629359, 3.000000000000002665, -178.4613248654052313 ) ) ;
#29532 = ORIENTED_EDGE ( 'NONE', *, *, #1059, .T. ) ;
#29533 =( BOUNDED_CURVE ( )  B_SPLINE_CURVE ( 2, ( #21049, #9364, #6285, #15708, #25018, #18451, #13397, #6437, #6749 ),
 .UNSPECIFIED., .F., .F. ) 
 B_SPLINE_CURVE_WITH_KNOTS ( ( 3, 2, 2, 2, 3 ),
 ( 0.07812500000000000000, 0.08593750000000000000, 0.09375000000000000000, 0.1015625000000000000, 0.1093750000000000000 ),
 .UNSPECIFIED. ) 
 CURVE ( )  GEOMETRIC_REPRESENTATION_ITEM ( )  RATIONAL_B_SPLINE_CURVE ( ( 1.000000000000000000, 0.9238795325112867385, 1.000000000000000000, 0.9238795325112867385, 1.000000000000000000, 0.9238795325112867385, 1.000000000000000000, 0.9238795325112867385, 1.000000000000000000 ) ) 
 REPRESENTATION_ITEM ( '' )  );
#29534 = CARTESIAN_POINT ( 'NONE',  ( -4.763139720814407951, -2.750000000000016431, -64.00000000000000000 ) ) ;
#29535 = EDGE_CURVE ( 'NONE', #14644, #12881, #24135, .T. ) ;
#29536 = DIRECTION ( 'NONE',  ( -0.000000000000000000, -0.000000000000000000, -1.000000000000000000 ) ) ;
#29537 = ORIENTED_EDGE ( 'NONE', *, *, #13407, .F. ) ;
#29538 = CARTESIAN_POINT ( 'NONE',  ( 108.2499999999998863, 5.551115123125782702E-14, 2.499999999999946709 ) ) ;
#29539 = CARTESIAN_POINT ( 'NONE',  ( 145.7812500000000284, 2.485281374238585972, 6.000000000000005329 ) ) ;
#29540 = CARTESIAN_POINT ( 'NONE',  ( 141.6636751345948255, 0.000000000000000000, 5.500000000000005329 ) ) ;
#29541 = CARTESIAN_POINT ( 'NONE',  ( 14.81250000000010658, 0.8284271247463557142, -2.000000000000031530 ) ) ;
#29542 = CARTESIAN_POINT ( 'NONE',  ( 3.464101615137757051, -5.999999999999979572, -48.91367513459484684 ) ) ;
#29543 = ORIENTED_EDGE ( 'NONE', *, *, #6216, .T. ) ;
#29544 = CARTESIAN_POINT ( 'NONE',  ( 138.4687500000000284, -2.485281374238585972, 6.000000000000005329 ) ) ;
#29545 = CARTESIAN_POINT ( 'NONE',  ( 161.2143795948215370, -3.807535749796857605, 4.272797826763722995 ) ) ;
#29546 = ORIENTED_EDGE ( 'NONE', *, *, #4895, .T. ) ;
#29547 = B_SPLINE_CURVE_WITH_KNOTS ( 'NONE', 3,
 ( #13503, #22843, #20537, #8867, #18860, #22004, #7860, #21860, #2951, #16569, #9163, #5548, #9318, #24005, #24153, #28034, #16278, #92, #12367, #18556, #28740, #19560, #7004, #25596, #26297, #27881, #7712, #21717, #805, #11815, #23466, #12523, #28895, #25745, #16423, #4692, #21153, #5252 ),
 .UNSPECIFIED., .F., .F.,
 ( 4, 2, 2, 2, 2, 2, 2, 2, 2, 2, 2, 2, 2, 2, 2, 2, 2, 2, 4 ),
 ( 0.01915730813553682965, 0.01975454893833632555, 0.02035178974113582145, 0.02154627134673480979, 0.02274075295233380159, 0.02393523455793278992, 0.02512971616353178173, 0.02632419776913077353, 0.02751867937472976533, 0.02871316098032875713, 0.02990764258592774893, 0.03110212419152673727, 0.03229660579712572560, 0.03349108740272471740, 0.03468556900832370227, 0.03528280981112319470, 0.03588005061392269407, 0.03707453221952168587, 0.03826901382512067074 ),
 .UNSPECIFIED. ) ;
#29548 = CARTESIAN_POINT ( 'NONE',  ( -2.775557561562891351E-14, -5.500000000000115463, -141.7500000000000568 ) ) ;
#29549 = CARTESIAN_POINT ( 'NONE',  ( 3.608439182435180470, 6.249999999999982236, -47.69198729810783277 ) ) ;
#29550 = CARTESIAN_POINT ( 'NONE',  ( 17.75000000000015632, 1.110223024625156540E-13, -2.000000000000001776 ) ) ;
#29551 = ORIENTED_EDGE ( 'NONE', *, *, #11975, .F. ) ;
#29552 = CARTESIAN_POINT ( 'NONE',  ( -3.175426480542816510, -5.500000000000057732, -75.87500000000001421 ) ) ;
#29553 = CARTESIAN_POINT ( 'NONE',  ( 15.18750000000004086, 1.097466725451679892, -2.649519052838238409 ) ) ;
#29554 = CARTESIAN_POINT ( 'NONE',  ( -5.412658773652739619, 3.124999999999975131, -96.18301270189222407 ) ) ;
#29555 = ORIENTED_EDGE ( 'NONE', *, *, #17909, .F. ) ;
#29556 = CARTESIAN_POINT ( 'NONE',  ( -2.687256737965178832, -10.66819377212465447, -30.36813770228164699 ) ) ;
#29557 = ADVANCED_FACE ( 'NONE', ( #24522 ), #15032, .T. ) ;
#29558 = CARTESIAN_POINT ( 'NONE',  ( 5.999999999999999112, 2.951592740943527306E-14, -150.6636751345948539 ) ) ;
#29559 = CARTESIAN_POINT ( 'NONE',  ( 110.4136751345947260, 1.414213562373117794, 1.414213562373034527 ) ) ;
#29560 = APPLICATION_PROTOCOL_DEFINITION ( 'draft international standard', 'automotive_design', 1998, #7328 ) ;
#29561 = CARTESIAN_POINT ( 'NONE',  ( -2.775557561562891351E-14, -5.500000000000115463, -158.2500000000000000 ) ) ;
#29562 = DIRECTION ( 'NONE',  ( 1.000000000000000000, -5.551115123125773458E-17, -1.260129944081490338E-35 ) ) ;
#29563 = CARTESIAN_POINT ( 'NONE',  ( -3.106370373191974732, 4.832402510093865899, -180.0000000000000853 ) ) ;
#29564 = CARTESIAN_POINT ( 'NONE',  ( 3.175426480543072749, 5.499999999999865885, -85.62500000000000000 ) ) ;
#29565 = CARTESIAN_POINT ( 'NONE',  ( 104.5622167782374561, 1.849990392679501827, -0.7662911109076485650 ) ) ;
#29566 = ADVANCED_FACE ( 'NONE', ( #13059 ), #12750, .T. ) ;
#29567 = CARTESIAN_POINT ( 'NONE',  ( 4.763139720814407951, -2.749999999999988454, -74.00000000000001421 ) ) ;
#29568 =( BOUNDED_CURVE ( )  B_SPLINE_CURVE ( 2, ( #19350, #17354, #21650, #5185, #12600, #17203, #2886, #21504, #26669 ),
 .UNSPECIFIED., .F., .T. ) 
 B_SPLINE_CURVE_WITH_KNOTS ( ( 3, 2, 2, 2, 3 ),
 ( 0.3972222222222222543, 0.3981481481481481399, 0.4000000000000000222, 0.4018518518518519045, 0.4027777777777777901 ),
 .UNSPECIFIED. ) 
 CURVE ( )  GEOMETRIC_REPRESENTATION_ITEM ( )  RATIONAL_B_SPLINE_CURVE ( ( 0.9330127018922194093, 0.9330127018922234061, 1.000000000000000000, 0.8660254037844388186, 1.000000000000000000, 0.8660254037844388186, 1.000000000000000000, 0.9330127018922194093, 0.9330127018922194093 ) ) 
 REPRESENTATION_ITEM ( '' )  );
#29569 = VECTOR ( 'NONE', #18389, 1000.000000000000000 ) ;
#29570 = EDGE_CURVE ( 'NONE', #16234, #26967, #3470, .T. ) ;
#29571 = CYLINDRICAL_SURFACE ( 'NONE', #21694, 6.000000000000000888 ) ;
#29572 = CARTESIAN_POINT ( 'NONE',  ( 153.8586002691896510, 2.071067811865468400, 4.999999999999989342 ) ) ;
#29573 = CARTESIAN_POINT ( 'NONE',  ( 6.000000000000000888, 1.743066579297358182E-13, -106.5863248654052313 ) ) ;
#29574 = CARTESIAN_POINT ( 'NONE',  ( 135.4761751345948539, 3.889087296526011706, 3.889087296526011706 ) ) ;
#29575 = CARTESIAN_POINT ( 'NONE',  ( 3.464101615137852974, 5.999999999999884537, -124.9136751345948113 ) ) ;
#29576 = CARTESIAN_POINT ( 'NONE',  ( 150.3675748654052313, -5.500000000000012434, 2.278174593052012309 ) ) ;
#29577 = DIRECTION ( 'NONE',  ( -1.000000000000000000, 0.000000000000000000, 0.000000000000000000 ) ) ;
#29578 = ORIENTED_EDGE ( 'NONE', *, *, #27893, .F. ) ;
#29579 = CARTESIAN_POINT ( 'NONE',  ( 157.7812500000000568, 2.485281374238585972, 6.000000000000005329 ) ) ;
#29580 = DIRECTION ( 'NONE',  ( -7.147005652999508048E-36, 5.642372883946980038E-36, 1.000000000000000000 ) ) ;
#29581 = CARTESIAN_POINT ( 'NONE',  ( 6.000000000000000888, -1.607695154586752384, -171.7306624327026157 ) ) ;
#29582 = CARTESIAN_POINT ( 'NONE',  ( 116.9377832217621460, -1.849990392679441875, -0.7662911109077087390 ) ) ;
#29583 = FACE_OUTER_BOUND ( 'NONE', #14377, .T. ) ;
#29584 = VERTEX_POINT ( 'NONE', #26970 ) ;
#29585 = CARTESIAN_POINT ( 'NONE',  ( 0.000000000000000000, 5.499999999999991118, -96.00000000000002842 ) ) ;
#29586 = CARTESIAN_POINT ( 'NONE',  ( 16.25000000000009948, 1.873492889145123019, -1.873492889145011997 ) ) ;
#29587 = CARTESIAN_POINT ( 'NONE',  ( 6.000000000000000888, -3.330669073875464691E-16, -7.560779664488942560E-35 ) ) ;
#29588 = CARTESIAN_POINT ( 'NONE',  ( 2.775557561562891351E-14, -6.250000000000061284, -118.1830127018922383 ) ) ;
#29589 = ORIENTED_EDGE ( 'NONE', *, *, #14910, .F. ) ;
#29590 = CARTESIAN_POINT ( 'NONE',  ( 5.196152422706629359, 3.000000000000002665, -94.46132486540520290 ) ) ;
#29591 = FILL_AREA_STYLE_COLOUR ( '', #15767 ) ;
#29592 = CARTESIAN_POINT ( 'NONE',  ( 0.7509638210179210294, -15.55246597669451170, 8.023235780102909942 ) ) ;
#29593 = EDGE_CURVE ( 'NONE', #29422, #765, #23152, .T. ) ;
#29594 = CARTESIAN_POINT ( 'NONE',  ( 2.775557561562891351E-14, -6.250000000000061284, -53.68301270189223828 ) ) ;
#29595 = VERTEX_POINT ( 'NONE', #20088 ) ;
#29596 = DIRECTION ( 'NONE',  ( 1.000000000000000000, 0.000000000000000000, 0.000000000000000000 ) ) ;
#29597 = EDGE_CURVE ( 'NONE', #4074, #7068, #3322, .T. ) ;
#29598 = CARTESIAN_POINT ( 'NONE',  ( 6.350852961086080661, -9.614813431917819062E-14, -162.3750000000000284 ) ) ;
#29599 = CARTESIAN_POINT ( 'NONE',  ( 117.0624999999998579, 2.500000000000234479, 1.035533905932989551 ) ) ;
#29600 = CARTESIAN_POINT ( 'NONE',  ( 6.000000000000052403, -1.607695154586662678, -157.6533121635129362 ) ) ;
#29601 = CARTESIAN_POINT ( 'NONE',  ( 6.350852961086080661, -9.614813431917819062E-14, -111.3750000000000426 ) ) ;
#29602 = FACE_OUTER_BOUND ( 'NONE', #3775, .T. ) ;
#29603 = CARTESIAN_POINT ( 'NONE',  ( -2.775557561562891351E-14, -5.500000000000115463, -104.2500000000000142 ) ) ;
#29604 = SURFACE_SIDE_STYLE ('',( #22560 ) ) ;
#29605 = CARTESIAN_POINT ( 'NONE',  ( 5.196152422706629359, 3.000000000000002665, -118.4613248654052313 ) ) ;
#29606 = EDGE_LOOP ( 'NONE', ( #23963, #23704 ) ) ;
#29607 = CARTESIAN_POINT ( 'NONE',  ( 14.31249999999993072, -1.097466725451559322, -2.649519052838358757 ) ) ;
#29608 = CARTESIAN_POINT ( 'NONE',  ( 115.4999999999998153, -2.499999999999891198, 0.000000000000000000 ) ) ;
#29609 = CARTESIAN_POINT ( 'NONE',  ( 108.9377832217621886, -1.849990392679411677, -0.7662911109076485650 ) ) ;
#29610 = CARTESIAN_POINT ( 'NONE',  ( -5.196152422706573404, -3.000000000000002665, -134.2113248654052029 ) ) ;
#29611 = CARTESIAN_POINT ( 'NONE',  ( -3.175426480542816510, 5.499999999999865885, -158.8750000000000000 ) ) ;
#29612 = FILL_AREA_STYLE ('',( #6727 ) ) ;
#29613 = AXIS2_PLACEMENT_3D ( 'NONE', #7993, #1224, #10321 ) ;
#29614 = CARTESIAN_POINT ( 'NONE',  ( 2.775557561562891351E-14, -6.250000000000061284, -88.81698729810783277 ) ) ;
#29615 = ORIENTED_EDGE ( 'NONE', *, *, #16341, .F. ) ;
#29616 = CARTESIAN_POINT ( 'NONE',  ( 0.000000000000000000, 0.000000000000000000, 0.000000000000000000 ) ) ;
#29617 = ORIENTED_EDGE ( 'NONE', *, *, #24664, .F. ) ;
#29618 = CARTESIAN_POINT ( 'NONE',  ( 153.8437500000000284, -6.000000000000005329, -2.485281374238555774 ) ) ;
#29619 = CARTESIAN_POINT ( 'NONE',  ( -2.775557561562891351E-14, -5.500000000000115463, -119.2500000000000284 ) ) ;
#29620 = CARTESIAN_POINT ( 'NONE',  ( -3.608439182435052128, -6.250000000000110134, -142.3080127018922667 ) ) ;
#29621 = ORIENTED_EDGE ( 'NONE', *, *, #1092, .F. ) ;
#29622 = CARTESIAN_POINT ( 'NONE',  ( 151.2261751345948539, -3.889087296526011706, -3.889087296526011706 ) ) ;
#29623 = CARTESIAN_POINT ( 'NONE',  ( 2.775557561562891351E-14, -6.250000000000061284, -124.8169872981078612 ) ) ;
#29624 = CARTESIAN_POINT ( 'NONE',  ( 2.775557561562891351E-14, -6.250000000000061284, -177.3169872981078470 ) ) ;
#29625 = CARTESIAN_POINT ( 'NONE',  ( 4.763139720814407951, -2.749999999999988454, -174.5000000000000000 ) ) ;
#29626 = SURFACE_SIDE_STYLE ('',( #6742 ) ) ;
#29627 = ADVANCED_FACE ( 'NONE', ( #15511 ), #27130, .T. ) ;
#29628 = ORIENTED_EDGE ( 'NONE', *, *, #27125, .F. ) ;
#29629 = CARTESIAN_POINT ( 'NONE',  ( 12.31250000000004974, -0.8284271247461753029, 2.000000000000091926 ) ) ;
#29630 = DIRECTION ( 'NONE',  ( 1.000000000000000000, -5.551115123125773458E-17, -1.260129944081490338E-35 ) ) ;
#29631 = EDGE_CURVE ( 'NONE', #29267, #12068, #29522, .T. ) ;
#29632 = CARTESIAN_POINT ( 'NONE',  ( -5.999999999999963585, -1.487416814333745711E-14, -170.9136751345948255 ) ) ;
#29633 = CARTESIAN_POINT ( 'NONE',  ( 113.0627832217621886, -0.7662911109076184779, -1.849990392679291551 ) ) ;
#29634 = CARTESIAN_POINT ( 'NONE',  ( -3.608439182435115633, 6.249999999999965361, -71.44198729810781856 ) ) ;
#29635 = CARTESIAN_POINT ( 'NONE',  ( -5.412658773652739619, 3.124999999999975131, -57.81698729810780435 ) ) ;
#29636 = CARTESIAN_POINT ( 'NONE',  ( 0.000000000000000000, 0.000000000000000000, 0.000000000000000000 ) ) ;
#29637 = CARTESIAN_POINT ( 'NONE',  ( -4.763139720814407951, -2.750000000000016431, -49.00000000000004263 ) ) ;
#29638 = DIRECTION ( 'NONE',  ( 0.000000000000000000, -0.9393939393939397808, 0.3428396514843859988 ) ) ;
#29639 = CARTESIAN_POINT ( 'NONE',  ( -38.99999999999998579, -59.99999999999980105, -4.000000000000003553 ) ) ;
#29640 = CARTESIAN_POINT ( 'NONE',  ( 3.175426480543072749, 5.499999999999865885, -132.1250000000000284 ) ) ;
#29641 = CARTESIAN_POINT ( 'NONE',  ( -5.999999999999963585, 1.780251999655701777E-13, -85.41367513459483973 ) ) ;
#29642 = ORIENTED_EDGE ( 'NONE', *, *, #1174, .T. ) ;
#29643 = CARTESIAN_POINT ( 'NONE',  ( 23.18750000000004619, -2.649519052838238409, -1.097466725451559322 ) ) ;
#29644 = CARTESIAN_POINT ( 'NONE',  ( 160.3050748654052029, 5.500000000000012434, 2.278174593052012309 ) ) ;
#29645 = CARTESIAN_POINT ( 'NONE',  ( -5.999999999999963585, -1.487416814333745711E-14, -50.91367513459483973 ) ) ;
#29646 = CARTESIAN_POINT ( 'NONE',  ( 142.2336002691896226, -4.999999999999989342, 2.071067811865468400 ) ) ;
#29647 = ORIENTED_EDGE ( 'NONE', *, *, #28303, .F. ) ;
#29648 = CARTESIAN_POINT ( 'NONE',  ( 114.0622167782374845, -1.849990392679501827, 0.7662911109078287542 ) ) ;
#29649 = CARTESIAN_POINT ( 'NONE',  ( 9.562500000000090594, -1.999999999999851674, -0.8284271247462354770 ) ) ;
#29650 = CARTESIAN_POINT ( 'NONE',  ( 5.412658773652739619, 3.124999999999988898, -113.8169872981078470 ) ) ;
#29651 = CARTESIAN_POINT ( 'NONE',  ( 140.0256844536733922, -11.04862469602451291, -4.684420475249996052 ) ) ;
#29652 =( BOUNDED_CURVE ( )  B_SPLINE_CURVE ( 2, ( #23628, #401, #21915, #28502, #2856, #2561, #11985, #26058, #9943 ),
 .UNSPECIFIED., .F., .T. ) 
 B_SPLINE_CURVE_WITH_KNOTS ( ( 3, 2, 2, 2, 3 ),
 ( 0.1176470588235294379, 0.1250000000000000000, 0.1323529411764705621, 0.1397058823529411242, 0.1470588235294117974 ),
 .UNSPECIFIED. ) 
 CURVE ( )  GEOMETRIC_REPRESENTATION_ITEM ( )  RATIONAL_B_SPLINE_CURVE ( ( 1.000000000000000000, 0.9238795325112867385, 1.000000000000000000, 0.9238795325112867385, 1.000000000000000000, 0.9238795325112867385, 1.000000000000000000, 0.9238795325112867385, 1.000000000000000000 ) ) 
 REPRESENTATION_ITEM ( '' )  );
#29653 = CARTESIAN_POINT ( 'NONE',  ( 6.000000000000000888, -3.330669073875464691E-16, -7.560779664488942560E-35 ) ) ;
#29654 = ORIENTED_EDGE ( 'NONE', *, *, #4037, .T. ) ;
#29655 = CARTESIAN_POINT ( 'NONE',  ( 159.6405936598872586, -12.17689969114422688, 3.778228146401014342 ) ) ;
#29656 = CARTESIAN_POINT ( 'NONE',  ( 139.7812500000000284, 2.485281374238585972, 6.000000000000005329 ) ) ;
#29657 =( BOUNDED_CURVE ( )  B_SPLINE_CURVE ( 2, ( #4939, #23265, #9730, #14370, #19107, #28432, #16671, #9575, #23708 ),
 .UNSPECIFIED., .F., .T. ) 
 B_SPLINE_CURVE_WITH_KNOTS ( ( 3, 2, 2, 2, 3 ),
 ( 0.7625000000000011768, 0.7687500000000010436, 0.7750000000000007994, 0.7812500000000004441, 0.7875000000000001998 ),
 .UNSPECIFIED. ) 
 CURVE ( )  GEOMETRIC_REPRESENTATION_ITEM ( )  RATIONAL_B_SPLINE_CURVE ( ( 0.9999999999999851230, 0.9238795325113016155, 1.000000000000000000, 0.9238795325112867385, 1.000000000000000000, 0.9238795325112867385, 1.000000000000000000, 0.9238795325112840739, 1.000000000000002665 ) ) 
 REPRESENTATION_ITEM ( '' )  );
#29658 = ORIENTED_EDGE ( 'NONE', *, *, #21742, .T. ) ;
#29659 = ORIENTED_EDGE ( 'NONE', *, *, #2900, .T. ) ;
#29660 = SURFACE_STYLE_USAGE ( .BOTH. , #20312 ) ;
#29661 = CARTESIAN_POINT ( 'NONE',  ( 3.175426480543072749, 5.499999999999865885, -49.62500000000001421 ) ) ;
#29662 = CARTESIAN_POINT ( 'NONE',  ( 23.68750000000013500, -0.8284271247461152399, -1.999999999999911626 ) ) ;
#29663 = CARTESIAN_POINT ( 'NONE',  ( 6.000000000000000888, -1.859271017917181981E-14, -141.6636751345948255 ) ) ;
#29664 = CARTESIAN_POINT ( 'NONE',  ( 5.999999999999949374, 1.607695154586804565, -62.09668783648702117 ) ) ;
#29665 = CARTESIAN_POINT ( 'NONE',  ( -3.608439182435052128, -6.250000000000110134, -70.30801270189220986 ) ) ;
#29666 = EDGE_CURVE ( 'NONE', #19330, #3655, #450, .T. ) ;
#29667 = FACE_OUTER_BOUND ( 'NONE', #16782, .T. ) ;
#29668 = CARTESIAN_POINT ( 'NONE',  ( 149.1413997308104058, 2.071067811865468400, -4.999999999999989342 ) ) ;
#29669 = CARTESIAN_POINT ( 'NONE',  ( 23.96132486540522422, 5.551115123125782702E-14, 2.500000000000002220 ) ) ;
#29670 = DIRECTION ( 'NONE',  ( -7.147005652999508048E-36, 5.642372883946980038E-36, 1.000000000000000000 ) ) ;
#29671 = CIRCLE ( 'NONE', #16970, 1.000000000000000222 ) ;
#29672 = DIRECTION ( 'NONE',  ( -1.000000000000000000, -1.665334536937731113E-16, 1.526556658859586792E-16 ) ) ;
#29673 = CARTESIAN_POINT ( 'NONE',  ( 5.196152422706629359, 3.000000000000002665, -115.4613248654052171 ) ) ;
#29674 = CARTESIAN_POINT ( 'NONE',  ( -4.763139720814407951, 2.749999999999946709, -134.7500000000000284 ) ) ;
#29675 = CARTESIAN_POINT ( 'NONE',  ( 16.10117513459491789, 1.035533905932869425, -2.499999999999904521 ) ) ;
#29676 = EDGE_LOOP ( 'NONE', ( #14121, #762, #7354, #2167, #15809 ) ) ;
#29677 = CARTESIAN_POINT ( 'NONE',  ( 3.175426480543072749, -5.500000000000105693, -63.62500000000001421 ) ) ;
#29678 = DIRECTION ( 'NONE',  ( -7.147005652999508048E-36, 5.642372883946980038E-36, 1.000000000000000000 ) ) ;
#29679 = CARTESIAN_POINT ( 'NONE',  ( 6.000000000000000888, -1.859271017917181981E-14, -172.5863248654052029 ) ) ;
#29680 = CARTESIAN_POINT ( 'NONE',  ( -5.999999999999964473, 9.063946212346262433E-15, -174.8363248654052313 ) ) ;
#29681 = ORIENTED_EDGE ( 'NONE', *, *, #26599, .F. ) ;
#29682 = CARTESIAN_POINT ( 'NONE',  ( 110.4999999999999432, -2.499999999999891198, 3.330669073875469621E-13 ) ) ;
#29683 = CARTESIAN_POINT ( 'NONE',  ( 145.0312500000000568, -2.485281374238556218, -6.000000000000005329 ) ) ;
#29684 = FACE_OUTER_BOUND ( 'NONE', #12438, .T. ) ;
#29685 = CARTESIAN_POINT ( 'NONE',  ( 141.0000000000000284, -12.00000000000001066, -4.000000000000003553 ) ) ;
#29686 = CARTESIAN_POINT ( 'NONE',  ( 139.7812500000000284, 2.485281374238585972, 6.000000000000005329 ) ) ;
#29687 = CARTESIAN_POINT ( 'NONE',  ( 22.03867513459498184, 1.110223024625156540E-13, -2.500000000000057732 ) ) ;
#29688 = EDGE_CURVE ( 'NONE', #6944, #15581, #16519, .T. ) ;
#29689 = ORIENTED_EDGE ( 'NONE', *, *, #21297, .T. ) ;
#29690 = VECTOR ( 'NONE', #18391, 1000.000000000000114 ) ;
#29691 = EDGE_CURVE ( 'NONE', #23494, #18429, #3026, .T. ) ;
#29692 = CARTESIAN_POINT ( 'NONE',  ( -4.763139720814407951, 2.749999999999946709, -148.2500000000000000 ) ) ;
#29693 = ORIENTED_EDGE ( 'NONE', *, *, #14719, .F. ) ;
#29694 = CARTESIAN_POINT ( 'NONE',  ( 14.31250000000002309, -0.8284271247461153509, 2.000000000000151879 ) ) ;
#29695 = ORIENTED_EDGE ( 'NONE', *, *, #19184, .T. ) ;
#29696 = CARTESIAN_POINT ( 'NONE',  ( -6.350852961085760029, -1.281975124255709124E-13, -71.62500000000005684 ) ) ;
#29697 = CARTESIAN_POINT ( 'NONE',  ( 18.47617513459497474, 1.035533905932929599, 2.499999999999844569 ) ) ;
#29698 = CARTESIAN_POINT ( 'NONE',  ( -5.412658773652684552, -3.125000000000099920, -89.93301270189223828 ) ) ;
#29699 = EDGE_CURVE ( 'NONE', #24857, #8961, #2976, .T. ) ;
#29700 = VERTEX_POINT ( 'NONE', #684 ) ;
#29701 = AXIS2_PLACEMENT_3D ( 'NONE', #12448, #21791, #7355 ) ;
#29702 = CARTESIAN_POINT ( 'NONE',  ( 105.2886751345946550, 2.000000000000057288, 0.000000000000000000 ) ) ;
#29703 = CARTESIAN_POINT ( 'NONE',  ( 0.000000000000000000, 5.999999999999977796, -46.78867513459483973 ) ) ;
#29704 = CARTESIAN_POINT ( 'NONE',  ( 135.3537946693345759, -8.430374945247399054, -8.227582779367073940 ) ) ;
#29705 = CARTESIAN_POINT ( 'NONE',  ( 121.2502832217622171, 1.308140751793640533, -1.308140751793418488 ) ) ;
#29706 = ITEM_DEFINED_TRANSFORMATION ( 'NONE', 'NONE', #2139,  #18805 ) ;
#29707 = CARTESIAN_POINT ( 'NONE',  ( 6.350852961086080661, -9.614813431917819062E-14, -157.8750000000000284 ) ) ;
#29708 = CARTESIAN_POINT ( 'NONE',  ( -6.000000000000000888, 1.067854986875958443E-15, 7.560779664488942560E-35 ) ) ;
#29709 = CARTESIAN_POINT ( 'NONE',  ( -5.196152422706601826, 2.999999999999975131, -48.96132486540521711 ) ) ;
#29710 = CIRCLE ( 'NONE', #27245, 0.5000000000000004441 ) ;
#29711 = CARTESIAN_POINT ( 'NONE',  ( 3.175426480543072749, 5.499999999999865885, -90.12500000000001421 ) ) ;
#29712 = CARTESIAN_POINT ( 'NONE',  ( 4.763139720814407951, 2.750000000000002665, -70.75000000000002842 ) ) ;
#29713 = DIRECTION ( 'NONE',  ( -7.147005652999508048E-36, 5.642372883946980038E-36, 1.000000000000000000 ) ) ;
#29714 = CARTESIAN_POINT ( 'NONE',  ( 0.000000000000000000, 0.000000000000000000, 0.000000000000000000 ) ) ;
#29715 = CARTESIAN_POINT ( 'NONE',  ( -19.99999999999998224, -25.00000000000010658, -5.000000000000004441 ) ) ;
#29716 = CARTESIAN_POINT ( 'NONE',  ( 3.464101615137852974, 5.999999999999884537, -118.9136751345948397 ) ) ;
#29717 = DIRECTION ( 'NONE',  ( 1.000000000000000000, -0.000000000000000000, -0.000000000000000000 ) ) ;
#29718 = LINE ( 'NONE', #15490, #4653 ) ;
#29719 = ORIENTED_EDGE ( 'NONE', *, *, #9858, .T. ) ;
#29720 = CARTESIAN_POINT ( 'NONE',  ( 157.0312500000000853, -2.485281374238555774, -6.000000000000005329 ) ) ;
#29721 = CARTESIAN_POINT ( 'NONE',  ( 116.3752832217622597, 1.849990392679523588, 0.000000000000000000 ) ) ;
#29722 = CIRCLE ( 'NONE', #29205, 1.000000000000000444 ) ;
#29723 = EDGE_CURVE ( 'NONE', #20406, #21808, #15003, .T. ) ;
#29724 = FACE_OUTER_BOUND ( 'NONE', #30379, .T. ) ;
#29725 = ORIENTED_EDGE ( 'NONE', *, *, #27299, .F. ) ;
#29726 = VECTOR ( 'NONE', #15314, 1000.000000000000000 ) ;
#29727 = ORIENTED_EDGE ( 'NONE', *, *, #20566, .T. ) ;
#29728 = CARTESIAN_POINT ( 'NONE',  ( 0.000000000000000000, 5.499999999999991118, -94.50000000000002842 ) ) ;
#29729 = CARTESIAN_POINT ( 'NONE',  ( 3.464101615137852974, 5.999999999999884537, -96.41367513459479710 ) ) ;
#29730 = EDGE_CURVE ( 'NONE', #28093, #15499, #26034, .T. ) ;
#29731 = CARTESIAN_POINT ( 'NONE',  ( 2.775557561562891351E-14, 6.250000000000033751, -112.9330127018922667 ) ) ;
#29732 = EDGE_CURVE ( 'NONE', #6232, #8188, #19584, .T. ) ;
#29733 = ORIENTED_EDGE ( 'NONE', *, *, #8956, .F. ) ;
#29734 = FACE_OUTER_BOUND ( 'NONE', #5165, .T. ) ;
#29735 = CARTESIAN_POINT ( 'NONE',  ( 140.3265217274359600, -9.159198771249785764, -7.753921182607669493 ) ) ;
#29736 = MECHANICAL_DESIGN_GEOMETRIC_PRESENTATION_REPRESENTATION (  '', ( #18016 ), #22900 ) ;
#29737 = DIRECTION ( 'NONE',  ( -1.000000000000000000, -1.665334536937736783E-16, -2.220446049250315546E-16 ) ) ;
#29738 = CARTESIAN_POINT ( 'NONE',  ( 2.775557561562891351E-14, -6.250000000000061284, -49.18301270189223828 ) ) ;
#29739 = ORIENTED_EDGE ( 'NONE', *, *, #22885, .T. ) ;
#29740 = DIRECTION ( 'NONE',  ( 0.000000000000000000, 0.000000000000000000, -1.000000000000000000 ) ) ;
#29741 =( BOUNDED_CURVE ( )  B_SPLINE_CURVE ( 2, ( #5112, #26160, #5411, #10208, #28460, #359, #21428, #14532, #5266 ),
 .UNSPECIFIED., .F., .T. ) 
 B_SPLINE_CURVE_WITH_KNOTS ( ( 3, 2, 2, 2, 3 ),
 ( 0.5374999999999999778, 0.5437500000000001776, 0.5500000000000004885, 0.5562500000000007994, 0.5625000000000009992 ),
 .UNSPECIFIED. ) 
 CURVE ( )  GEOMETRIC_REPRESENTATION_ITEM ( )  RATIONAL_B_SPLINE_CURVE ( ( 1.000000000000000000, 0.9238795325112867385, 1.000000000000000000, 0.9238795325112867385, 1.000000000000000000, 0.9238795325112867385, 1.000000000000000000, 0.9238795325112745260, 1.000000000000012212 ) ) 
 REPRESENTATION_ITEM ( '' )  );
#29742 = CARTESIAN_POINT ( 'NONE',  ( -5.999999999999866773, 1.607695154586893826, -135.9033121635129930 ) ) ;
#29743 = CARTESIAN_POINT ( 'NONE',  ( 4.763139720814407951, -2.749999999999988454, -164.0000000000000284 ) ) ;
#29744 = CARTESIAN_POINT ( 'NONE',  ( 116.1874999999999005, 1.035533905932839449, 2.500000000000205169 ) ) ;
#29745 = FILL_AREA_STYLE ('',( #25128 ) ) ;
#29746 = CARTESIAN_POINT ( 'NONE',  ( 3.175426480543072749, 5.499999999999865885, -108.1250000000000284 ) ) ;
#29747 = CARTESIAN_POINT ( 'NONE',  ( 106.0238248654050182, -0.8284271247461453269, 2.000000000000332179 ) ) ;
#29748 = CARTESIAN_POINT ( 'NONE',  ( -5.999999999999956479, -1.607695154586745057, -122.8466878364870496 ) ) ;
#29749 = CARTESIAN_POINT ( 'NONE',  ( 6.350852961086080661, -9.614813431917819062E-14, -99.37499999999998579 ) ) ;
#29750 = CARTESIAN_POINT ( 'NONE',  ( -3.464101615137757051, -5.999999999999979572, -112.1636751345948113 ) ) ;
#29751 = CARTESIAN_POINT ( 'NONE',  ( -6.000000000000007105, -1.607695154586655129, -82.34668783648702117 ) ) ;
#29752 = ORIENTED_EDGE ( 'NONE', *, *, #27785, .T. ) ;
#29753 = CARTESIAN_POINT ( 'NONE',  ( 14.12500000000002665, -2.649519052838222866, 0.000000000000000000 ) ) ;
#29754 = CARTESIAN_POINT ( 'NONE',  ( 112.3752832217621176, 1.849990392679551343, 0.000000000000000000 ) ) ;
#29755 = CARTESIAN_POINT ( 'NONE',  ( 0.000000000000000000, 0.000000000000000000, 0.000000000000000000 ) ) ;
#29756 = ORIENTED_EDGE ( 'NONE', *, *, #22820, .F. ) ;
#29757 = DIRECTION ( 'NONE',  ( 0.000000000000000000, -5.551115123125768527E-17, 1.000000000000000000 ) ) ;
#29758 = CARTESIAN_POINT ( 'NONE',  ( 109.4997167782374845, 1.308140751793696044, -1.308140751793640533 ) ) ;
#29759 = CARTESIAN_POINT ( 'NONE',  ( 2.775557561562891351E-14, -6.250000000000061284, -87.31698729810783277 ) ) ;
#29760 = ADVANCED_FACE ( 'NONE', ( #14413 ), #969, .T. ) ;
#29761 = DIRECTION ( 'NONE',  ( 1.000000000000000000, 0.000000000000000000, 0.000000000000000000 ) ) ;
#29762 = ORIENTED_EDGE ( 'NONE', *, *, #3301, .T. ) ;
#29763 = AXIS2_PLACEMENT_3D ( 'NONE', #18058, #25378, #17905 ) ;
#29764 = VECTOR ( 'NONE', #28844, 1000.000000000000000 ) ;
#29765 = CARTESIAN_POINT ( 'NONE',  ( 125.0000000000000568, -55.00000000000000711, -7.500000000000007105 ) ) ;
#29766 =( GEOMETRIC_REPRESENTATION_CONTEXT ( 3 ) GLOBAL_UNCERTAINTY_ASSIGNED_CONTEXT ( ( #7484 ) ) GLOBAL_UNIT_ASSIGNED_CONTEXT ( ( #13423, #11108, #26288 ) ) REPRESENTATION_CONTEXT ( 'NONE', 'WORKASPACE' ) );
#29767 = ORIENTED_EDGE ( 'NONE', *, *, #27092, .F. ) ;
#29768 = VERTEX_POINT ( 'NONE', #26177 ) ;
#29769 = CARTESIAN_POINT ( 'NONE',  ( 156.6562500000000284, -6.000000000000005329, 2.485281374238555774 ) ) ;
#29770 = CARTESIAN_POINT ( 'NONE',  ( 4.763139720814407951, -2.749999999999988454, -119.0000000000000000 ) ) ;
#29771 = EDGE_CURVE ( 'NONE', #9697, #84, #7538, .T. ) ;
#29772 = CARTESIAN_POINT ( 'NONE',  ( -5.412658773652739619, 3.124999999999975131, -139.6830127018922099 ) ) ;
#29773 = ORIENTED_EDGE ( 'NONE', *, *, #4133, .T. ) ;
#29774 = CARTESIAN_POINT ( 'NONE',  ( 2.775557561562891351E-14, 6.250000000000033751, -119.5669872981078328 ) ) ;
#29775 = CARTESIAN_POINT ( 'NONE',  ( -3.608439182435115633, 6.249999999999965361, -176.4419872981078470 ) ) ;
#29776 = AXIS2_PLACEMENT_3D ( 'NONE', #22069, #22685, #24354 ) ;
#29777 = CARTESIAN_POINT ( 'NONE',  ( 0.000000000000000000, 5.499999999999991118, -172.5000000000000000 ) ) ;
#29778 = CARTESIAN_POINT ( 'NONE',  ( -5.999999999999962697, 3.323446944526963891E-14, -151.4136751345948255 ) ) ;
#29779 = CARTESIAN_POINT ( 'NONE',  ( 6.000000000000000888, -1.859271017917181981E-14, -147.6636751345948255 ) ) ;
#29780 = VERTEX_POINT ( 'NONE', #2831 ) ;
#29781 = CARTESIAN_POINT ( 'NONE',  ( -4.999999999999886313, -15.00000000000001421, -7.500000000000007105 ) ) ;
#29782 = CARTESIAN_POINT ( 'NONE',  ( 1.110223024625164183E-16, -2.000000000000012879, -1.776356839400262692E-15 ) ) ;
#29783 = CARTESIAN_POINT ( 'NONE',  ( 159.4504201399719818, -12.08528864193560537, -3.895248697861249276 ) ) ;
#29784 = AXIS2_PLACEMENT_3D ( 'NONE', #26476, #11974, #7597 ) ;
#29785 = CARTESIAN_POINT ( 'NONE',  ( -5.999999999999963585, 1.780251999655701777E-13, -107.9136751345948397 ) ) ;
#29786 = CARTESIAN_POINT ( 'NONE',  ( 6.000000000000052403, -1.607695154586662678, -150.1533121635129646 ) ) ;
#29787 = CARTESIAN_POINT ( 'NONE',  ( 2.775557561562891351E-14, -6.250000000000061284, -75.31698729810781856 ) ) ;
#29788 = CARTESIAN_POINT ( 'NONE',  ( 5.412658773652739619, 3.124999999999988898, -59.81698729810780435 ) ) ;
#29789 = CARTESIAN_POINT ( 'NONE',  ( 0.000000000000000000, 5.999999999999977796, -110.7113248654052455 ) ) ;
#29790 = CARTESIAN_POINT ( 'NONE',  ( 3.175426480543072749, -5.500000000000105693, -51.62500000000001421 ) ) ;
#29791 = CYLINDRICAL_SURFACE ( 'NONE', #22604, 1.000000000000000888 ) ;
#29792 = CIRCLE ( 'NONE', #24364, 0.4999999999999983347 ) ;
#29793 = CARTESIAN_POINT ( 'NONE',  ( -3.175426480542816510, -5.500000000000057732, -122.3749999999999716 ) ) ;
#29794 = ORIENTED_EDGE ( 'NONE', *, *, #22328, .F. ) ;
#29795 = CARTESIAN_POINT ( 'NONE',  ( 5.196152422706629359, 3.000000000000002665, -132.5386751345948255 ) ) ;
#29796 =( BOUNDED_CURVE ( )  B_SPLINE_CURVE ( 2, ( #8711, #13933, #1322, #19922, #10887, #12896, #1632, #6240, #10734 ),
 .UNSPECIFIED., .F., .F. ) 
 B_SPLINE_CURVE_WITH_KNOTS ( ( 3, 2, 2, 2, 3 ),
 ( 0.6972222222222221877, 0.6981481481481481843, 0.6999999999999999556, 0.7018518518518518379, 0.7027777777777777235 ),
 .UNSPECIFIED. ) 
 CURVE ( )  GEOMETRIC_REPRESENTATION_ITEM ( )  RATIONAL_B_SPLINE_CURVE ( ( 0.9330127018922194093, 0.9330127018922154125, 1.000000000000000000, 0.8660254037844388186, 1.000000000000000000, 0.8660254037844388186, 1.000000000000000000, 0.9330127018922234061, 0.9330127018922194093 ) ) 
 REPRESENTATION_ITEM ( '' )  );
#29797 = CARTESIAN_POINT ( 'NONE',  ( 3.464101615137852974, 5.999999999999884537, -105.4136751345947971 ) ) ;
#29798 = DIRECTION ( 'NONE',  ( -7.147005652999508048E-36, 5.642372883946980038E-36, 1.000000000000000000 ) ) ;
#29799 = CARTESIAN_POINT ( 'NONE',  ( 136.9836002691896510, 4.999999999999989342, -2.071067811865468400 ) ) ;
#29800 = VERTEX_POINT ( 'NONE', #12254 ) ;
#29801 = VECTOR ( 'NONE', #8919, 1000.000000000000000 ) ;
#29802 = CARTESIAN_POINT ( 'NONE',  ( 109.3122167782373566, -0.7662911109077388261, -1.849990392679351725 ) ) ;
#29803 = CARTESIAN_POINT ( 'NONE',  ( 5.412658773652739619, 3.124999999999988898, -116.8169872981078612 ) ) ;
#29804 = EDGE_CURVE ( 'NONE', #2708, #8939, #10717, .T. ) ;
#29805 = CARTESIAN_POINT ( 'NONE',  ( 3.464101615137757051, -5.999999999999979572, -109.8363248654051745 ) ) ;
#29806 = EDGE_CURVE ( 'NONE', #8961, #20296, #14067, .T. ) ;
#29807 = CARTESIAN_POINT ( 'NONE',  ( 10.00000000000014744, 1.941674212873021999, 0.8547671284023850014 ) ) ;
#29808 = ORIENTED_EDGE ( 'NONE', *, *, #18463, .F. ) ;
#29809 = VERTEX_POINT ( 'NONE', #29669 ) ;
#29810 = CARTESIAN_POINT ( 'NONE',  ( 105.8511751345945981, -1.999999999999911626, -0.8284271247459350507 ) ) ;
#29811 = CARTESIAN_POINT ( 'NONE',  ( 144.3750000000000284, 0.000000000000000000, 6.000000000000005329 ) ) ;
#29812 = STYLED_ITEM ( 'NONE', ( #14650 ), #4906 ) ;
#29813 = ORIENTED_EDGE ( 'NONE', *, *, #29309, .F. ) ;
#29814 = VERTEX_POINT ( 'NONE', #8799 ) ;
#29815 = CYLINDRICAL_SURFACE ( 'NONE', #15574, 0.5000000000000000000 ) ;
#29816 = CARTESIAN_POINT ( 'NONE',  ( -3.175426480542816510, 5.499999999999865885, -49.37500000000000711 ) ) ;
#29817 = CARTESIAN_POINT ( 'NONE',  ( 22.87500000000000711, 1.414213562373312083, -1.414213562373090038 ) ) ;
#29818 = CYLINDRICAL_SURFACE ( 'NONE', #10815, 0.5000000000000004441 ) ;
#29819 = DIRECTION ( 'NONE',  ( 1.000000000000000000, 0.000000000000000000, 0.000000000000000000 ) ) ;
#29820 = CARTESIAN_POINT ( 'NONE',  ( -3.608439182435052128, -6.250000000000110134, -64.30801270189225249 ) ) ;
#29821 = CARTESIAN_POINT ( 'NONE',  ( 152.0476497308104058, 0.000000000000000000, -5.000000000000004441 ) ) ;
#29822 = CARTESIAN_POINT ( 'NONE',  ( 5.196152422706629359, 3.000000000000002665, -177.5386751345948255 ) ) ;
#29823 = FILL_AREA_STYLE ('',( #17891 ) ) ;
#29824 = CARTESIAN_POINT ( 'NONE',  ( -5.196152422706601826, 2.999999999999975131, -165.0386751345947971 ) ) ;
#29825 = DIRECTION ( 'NONE',  ( 0.000000000000000000, 0.000000000000000000, -1.000000000000000000 ) ) ;
#29826 =( LENGTH_UNIT ( ) NAMED_UNIT ( * ) SI_UNIT ( .MILLI., .METRE. ) );
#29827 = B_SPLINE_CURVE_WITH_KNOTS ( 'NONE', 3,
 ( #786, #23984, #26709, #2928 ),
 .UNSPECIFIED., .F., .F.,
 ( 4, 4 ),
 ( 0.000000000000000000, 0.0007769152796223661528 ),
 .UNSPECIFIED. ) ;
#29828 = CARTESIAN_POINT ( 'NONE',  ( -3.175426480542816066, 5.499999999999865885, -122.8749999999999716 ) ) ;
#29829 = DIRECTION ( 'NONE',  ( -7.147005652999508048E-36, 5.642372883946980038E-36, 1.000000000000000000 ) ) ;
#29830 = CARTESIAN_POINT ( 'NONE',  ( -5.412658773652739619, 3.124999999999975131, -145.6830127018922099 ) ) ;
#29831 = CYLINDRICAL_SURFACE ( 'NONE', #13582, 2.000000000000012879 ) ;
#29832 = ORIENTED_EDGE ( 'NONE', *, *, #26134, .T. ) ;
#29833 = CARTESIAN_POINT ( 'NONE',  ( 3.175426480543072749, 5.499999999999865885, -64.62500000000001421 ) ) ;
#29834 = CYLINDRICAL_SURFACE ( 'NONE', #14925, 2.499999999999999112 ) ;
#29835 = CARTESIAN_POINT ( 'NONE',  ( 3.464101615137852974, 5.999999999999884537, -172.3363248654052029 ) ) ;
#29836 =( BOUNDED_CURVE ( )  B_SPLINE_CURVE ( 2, ( #16734, #7468, #5002, #14437, #5152, #12278, #19318, #28641, #7612 ),
 .UNSPECIFIED., .F., .T. ) 
 B_SPLINE_CURVE_WITH_KNOTS ( ( 3, 2, 2, 2, 3 ),
 ( 0.6470588235294117974, 0.6544117647058823595, 0.6617647058823529216, 0.6691176470588234837, 0.6764705882352941568 ),
 .UNSPECIFIED. ) 
 CURVE ( )  GEOMETRIC_REPRESENTATION_ITEM ( )  RATIONAL_B_SPLINE_CURVE ( ( 1.000000000000000000, 0.9238795325112867385, 1.000000000000000000, 0.9238795325112867385, 1.000000000000000000, 0.9238795325112867385, 1.000000000000000000, 0.9238795325112867385, 1.000000000000000000 ) ) 
 REPRESENTATION_ITEM ( '' )  );
#29837 = VERTEX_POINT ( 'NONE', #13431 ) ;
#29838 = CARTESIAN_POINT ( 'NONE',  ( 107.1249999999998437, 1.767766952966265404, 1.767766952966320915 ) ) ;
#29839 = CARTESIAN_POINT ( 'NONE',  ( 148.0312500000000284, -2.485281374238556218, -6.000000000000005329 ) ) ;
#29840 = CARTESIAN_POINT ( 'NONE',  ( 160.0000000000000284, -11.67610212985246676, -2.769230769230771383 ) ) ;
#29841 = LINE ( 'NONE', #6801, #4266 ) ;
#29842 = EDGE_CURVE ( 'NONE', #15258, #18703, #14834, .T. ) ;
#29843 = CARTESIAN_POINT ( 'NONE',  ( 139.4062500000000284, 6.000000000000005329, -2.485281374238555774 ) ) ;
#29844 = DIRECTION ( 'NONE',  ( -7.147005652999508048E-36, 5.642372883946980038E-36, 1.000000000000000000 ) ) ;
#29845 = ORIENTED_EDGE ( 'NONE', *, *, #15498, .F. ) ;
#29846 = CARTESIAN_POINT ( 'NONE',  ( 3.175426480543072749, 5.499999999999865885, -142.6250000000000000 ) ) ;
#29847 = ORIENTED_EDGE ( 'NONE', *, *, #17380, .F. ) ;
#29848 = CARTESIAN_POINT ( 'NONE',  ( 11.87500000000007994, 1.414213562373312083, -1.414213562373090038 ) ) ;
#29849 = VERTEX_POINT ( 'NONE', #18185 ) ;
#29850 = CARTESIAN_POINT ( 'NONE',  ( -3.175426480542816510, -5.500000000000057732, -74.37500000000000000 ) ) ;
#29851 = CARTESIAN_POINT ( 'NONE',  ( 10.00000000000014744, 1.820735071450596099, -1.172870270573495910 ) ) ;
#29852 = CARTESIAN_POINT ( 'NONE',  ( 2.775557561562891351E-14, 6.250000000000033751, -87.43301270189223828 ) ) ;
#29853 = CARTESIAN_POINT ( 'NONE',  ( 6.000000000000000888, 1.743066579297358182E-13, -111.0863248654051887 ) ) ;
#29854 = CARTESIAN_POINT ( 'NONE',  ( 113.1636751345946692, 1.414213562373145550, -1.414213562372812483 ) ) ;
#29855 = DIRECTION ( 'NONE',  ( 1.000000000000000000, -5.551115123125773458E-17, -1.260129944081490338E-35 ) ) ;
#29856 = CARTESIAN_POINT ( 'NONE',  ( 24.50844993798688165, 0.4074731033292928184, 2.466641088734008669 ) ) ;
#29857 = APPLICATION_PROTOCOL_DEFINITION ( 'draft international standard', 'automotive_design', 1998, #8906 ) ;
#29858 = CARTESIAN_POINT ( 'NONE',  ( 0.000000000000000000, 5.499999999999991118, -153.0000000000000284 ) ) ;
#29859 = LINE ( 'NONE', #18525, #10912 ) ;
#29860 = CARTESIAN_POINT ( 'NONE',  ( 5.196152422706629359, 3.000000000000002665, -49.46132486540521711 ) ) ;
#29861 = ADVANCED_FACE ( 'NONE', ( #15746 ), #8319, .T. ) ;
#29862 = CARTESIAN_POINT ( 'NONE',  ( -3.175426480542816066, -5.500000000000057732, -87.87500000000000000 ) ) ;
#29863 = SURFACE_STYLE_FILL_AREA ( #18381 ) ;
#29864 = CARTESIAN_POINT ( 'NONE',  ( 4.763139720814407951, -2.749999999999988454, -71.00000000000001421 ) ) ;
#29865 = CARTESIAN_POINT ( 'NONE',  ( -5.999999999999963585, 9.296355089585909904E-15, -164.3363248654052313 ) ) ;
#29866 = CARTESIAN_POINT ( 'NONE',  ( 104.8953215971908293, -1.758631583619322480, -0.8464305698015709423 ) ) ;
#29867 = CARTESIAN_POINT ( 'NONE',  ( 161.1562500000000284, -6.000000000000005329, 2.485281374238556218 ) ) ;
#29868 = CARTESIAN_POINT ( 'NONE',  ( 3.464101615137757051, -5.999999999999979572, -149.4136751345947687 ) ) ;
#29869 = CARTESIAN_POINT ( 'NONE',  ( 18.62500000000003197, -1.414213562373034527, -1.414213562373090038 ) ) ;
#29870 = FACE_OUTER_BOUND ( 'NONE', #5645, .T. ) ;
#29871 = AXIS2_PLACEMENT_3D ( 'NONE', #13209, #20965, #15352 ) ;
#29872 = DIRECTION ( 'NONE',  ( -1.000000000000000000, 3.469446951953694061E-16, 0.000000000000000000 ) ) ;
#29873 = CARTESIAN_POINT ( 'NONE',  ( -5.999999999999963585, -1.487416814333745711E-14, -137.3363248654052313 ) ) ;
#29874 = EDGE_CURVE ( 'NONE', #22758, #1710, #13383, .T. ) ;
#29875 = ORIENTED_EDGE ( 'NONE', *, *, #10093, .T. ) ;
#29876 = CARTESIAN_POINT ( 'NONE',  ( 154.4062500000000284, 6.000000000000005329, -2.485281374238555774 ) ) ;
#29877 = CARTESIAN_POINT ( 'NONE',  ( 118.8127832217620465, -1.849990392679381701, 0.7662911109078287542 ) ) ;
#29878 =( BOUNDED_CURVE ( )  B_SPLINE_CURVE ( 2, ( #11936, #16684, #20968, #2372, #11775, #19268, #660, #26597, #15114 ),
 .UNSPECIFIED., .F., .F. ) 
 B_SPLINE_CURVE_WITH_KNOTS ( ( 3, 2, 2, 2, 3 ),
 ( 0.6624999999999992006, 0.6687499999999994005, 0.6749999999999998224, 0.6812500000000000222, 0.6875000000000002220 ),
 .UNSPECIFIED. ) 
 CURVE ( )  GEOMETRIC_REPRESENTATION_ITEM ( )  RATIONAL_B_SPLINE_CURVE ( ( 1.000000000000009548, 0.9238795325112773016, 1.000000000000000000, 0.9238795325112867385, 1.000000000000000000, 0.9238795325112867385, 1.000000000000000000, 0.9238795325112840739, 1.000000000000002665 ) ) 
 REPRESENTATION_ITEM ( '' )  );
#29879 = CARTESIAN_POINT ( 'NONE',  ( 3.464101615137852974, 5.999999999999884537, -157.3363248654051745 ) ) ;
#29880 = VERTEX_POINT ( 'NONE', #10972 ) ;
#29881 = ORIENTED_EDGE ( 'NONE', *, *, #12482, .F. ) ;
#29882 = CARTESIAN_POINT ( 'NONE',  ( 4.763139720814407951, 2.750000000000002665, -100.7500000000000000 ) ) ;
#29883 = CARTESIAN_POINT ( 'NONE',  ( 6.000000000000000888, 1.743066579297358182E-13, -96.66367513459479710 ) ) ;
#29884 = CARTESIAN_POINT ( 'NONE',  ( -7.216878364870328078, 0.000000000000000000, -109.5580127018922099 ) ) ;
#29885 = ORIENTED_EDGE ( 'NONE', *, *, #809, .F. ) ;
#29886 = CARTESIAN_POINT ( 'NONE',  ( -5.999999999999963585, -1.487416814333745711E-14, -50.33632486540523843 ) ) ;
#29887 = CARTESIAN_POINT ( 'NONE',  ( 6.000000000000026645, -1.607695154586707753, -143.2306624327025872 ) ) ;
#29888 = CARTESIAN_POINT ( 'NONE',  ( 5.196152422706629359, -2.999999999999988898, -63.21132486540520290 ) ) ;
#29889 = AXIS2_PLACEMENT_3D ( 'NONE', #11583, #13426, #20316 ) ;
#29890 = ORIENTED_EDGE ( 'NONE', *, *, #22818, .T. ) ;
#29891 = CARTESIAN_POINT ( 'NONE',  ( 3.464101615137852974, 5.999999999999884537, -153.4136751345947971 ) ) ;
#29892 =( GEOMETRIC_REPRESENTATION_CONTEXT ( 3 ) GLOBAL_UNCERTAINTY_ASSIGNED_CONTEXT ( ( #3592 ) ) GLOBAL_UNIT_ASSIGNED_CONTEXT ( ( #15981, #27283, #17658 ) ) REPRESENTATION_CONTEXT ( 'NONE', 'WORKASPACE' ) );
#29893 = CARTESIAN_POINT ( 'NONE',  ( 140.5000000000000284, -9.599999999999997868, 7.200000000000011724 ) ) ;
#29894 = CARTESIAN_POINT ( 'NONE',  ( 0.000000000000000000, 5.499999999999991118, -159.0000000000000284 ) ) ;
#29895 = CARTESIAN_POINT ( 'NONE',  ( 115.3124999999998863, -1.035533905932659149, 2.500000000000205169 ) ) ;
#29896 = SURFACE_STYLE_USAGE ( .BOTH. , #3786 ) ;
#29897 = VECTOR ( 'NONE', #12942, 1000.000000000000000 ) ;
#29898 = ADVANCED_FACE ( 'NONE', ( #26891 ), #10657, .T. ) ;
#29899 = CARTESIAN_POINT ( 'NONE',  ( -4.763139720814407951, 2.749999999999946709, -107.7500000000000142 ) ) ;
#29900 = DIRECTION ( 'NONE',  ( 1.000000000000000000, 0.000000000000000000, -0.000000000000000000 ) ) ;
#29901 = CARTESIAN_POINT ( 'NONE',  ( -4.763139720814407951, -2.750000000000016431, -97.00000000000002842 ) ) ;
#29902 = CARTESIAN_POINT ( 'NONE',  ( 159.2961002691896226, 2.071067811865468400, -4.999999999999989342 ) ) ;
#29903 = CARTESIAN_POINT ( 'NONE',  ( 0.1512544026176828038, -15.31703501317270977, 8.468610511427742793 ) ) ;
#29904 = ORIENTED_EDGE ( 'NONE', *, *, #9118, .F. ) ;
#29905 = CARTESIAN_POINT ( 'NONE',  ( 12.00000000000012079, -1.873492889144789952, 1.873492889144845464 ) ) ;
#29906 = CARTESIAN_POINT ( 'NONE',  ( 117.4374999999997584, -2.499999999999844569, 1.035533905932929599 ) ) ;
#29907 = CARTESIAN_POINT ( 'NONE',  ( 109.6252832217622739, -2.775557561562891351E-14, 1.849990392679523588 ) ) ;
#29908 = ADVANCED_FACE ( 'NONE', ( #25203 ), #22777, .T. ) ;
#29909 = DIRECTION ( 'NONE',  ( 1.000000000000000000, 0.000000000000000000, 0.000000000000000000 ) ) ;
#29910 = EDGE_LOOP ( 'NONE', ( #13968, #2066, #24659 ) ) ;
#29911 = DIRECTION ( 'NONE',  ( -7.147005652999508048E-36, 5.642372883946980038E-36, 1.000000000000000000 ) ) ;
#29912 = CARTESIAN_POINT ( 'NONE',  ( 108.2497167782376266, -1.308140751793585022, -1.308140751793640533 ) ) ;
#29913 = CARTESIAN_POINT ( 'NONE',  ( 7.216878364870455975, -6.409875621278545621E-14, -86.94198729810781856 ) ) ;
#29914 = VECTOR ( 'NONE', #28554, 1000.000000000000000 ) ;
#29915 = ORIENTED_EDGE ( 'NONE', *, *, #11615, .T. ) ;
#29916 = DIRECTION ( 'NONE',  ( -7.147005652999508048E-36, 5.642372883946980038E-36, 1.000000000000000000 ) ) ;
#29917 = AXIS2_PLACEMENT_3D ( 'NONE', #2988, #4437, #28624 ) ;
#29918 = ORIENTED_EDGE ( 'NONE', *, *, #14719, .T. ) ;
#29919 = CARTESIAN_POINT ( 'NONE',  ( 155.2500000000000284, -6.000000000000005329, 0.000000000000000000 ) ) ;
#29920 = CARTESIAN_POINT ( 'NONE',  ( 4.763139720814407951, 2.750000000000002665, -118.7500000000000284 ) ) ;
#29921 = CARTESIAN_POINT ( 'NONE',  ( 23.18750000000007461, 1.097466725451679892, -2.649519052838358757 ) ) ;
#29922 =( BOUNDED_CURVE ( )  B_SPLINE_CURVE ( 2, ( #20707, #2415, #4248, #7168, #4854, #16288, #28046, #2555, #23325 ),
 .UNSPECIFIED., .F., .F. ) 
 B_SPLINE_CURVE_WITH_KNOTS ( ( 3, 2, 2, 2, 3 ),
 ( 0.2031250000000000000, 0.2109375000000000000, 0.2187500000000000000, 0.2265625000000000000, 0.2343750000000000000 ),
 .UNSPECIFIED. ) 
 CURVE ( )  GEOMETRIC_REPRESENTATION_ITEM ( )  RATIONAL_B_SPLINE_CURVE ( ( 1.000000000000000000, 0.9238795325112867385, 1.000000000000000000, 0.9238795325112867385, 1.000000000000000000, 0.9238795325112867385, 1.000000000000000000, 0.9238795325112867385, 1.000000000000000000 ) ) 
 REPRESENTATION_ITEM ( '' )  );
#29923 = CARTESIAN_POINT ( 'NONE',  ( 5.412658773652739619, 3.124999999999988898, -128.1830127018922383 ) ) ;
#29924 = ORIENTED_EDGE ( 'NONE', *, *, #25685, .F. ) ;
#29925 = CARTESIAN_POINT ( 'NONE',  ( -5.196152422706601826, 2.999999999999975131, -160.5386751345948539 ) ) ;
#29926 = CARTESIAN_POINT ( 'NONE',  ( -7.216878364870328078, 0.000000000000000000, -122.1919872981078043 ) ) ;
#29927 = CARTESIAN_POINT ( 'NONE',  ( -3.608439182435052128, -6.250000000000110134, -174.4419872981078754 ) ) ;
#29928 = ORIENTED_EDGE ( 'NONE', *, *, #17345, .T. ) ;
#29929 = CARTESIAN_POINT ( 'NONE',  ( 11.37500000000010658, -1.414213562372979016, 1.414213562372979016 ) ) ;
#29930 = CARTESIAN_POINT ( 'NONE',  ( -5.999999999999962697, 3.323446944526963891E-14, -163.4136751345948539 ) ) ;
#29931 = CARTESIAN_POINT ( 'NONE',  ( 0.000000000000000000, 5.999999999999977796, -90.28867513459482552 ) ) ;
#29932 = DIRECTION ( 'NONE',  ( -1.000000000000000000, 0.000000000000000000, 0.000000000000000000 ) ) ;
#29933 = CARTESIAN_POINT ( 'NONE',  ( 0.8631338372297875372, -15.37878787878788067, -8.351220472436777342 ) ) ;
#29934 = CARTESIAN_POINT ( 'NONE',  ( 111.1877832217622029, 0.7662911109078588412, -1.849990392679411677 ) ) ;
#29935 = CARTESIAN_POINT ( 'NONE',  ( 7.216878364870455975, -6.409875621278545621E-14, -76.44198729810783277 ) ) ;
#29936 = CARTESIAN_POINT ( 'NONE',  ( 7.216878364870455975, -6.409875621278545621E-14, -59.94198729810782567 ) ) ;
#29937 = CARTESIAN_POINT ( 'NONE',  ( -5.196152422706573404, -3.000000000000002665, -170.7886751345948255 ) ) ;
#29938 = CARTESIAN_POINT ( 'NONE',  ( 2.775557561562891351E-14, 6.250000000000033751, -181.9330127018922099 ) ) ;
#29939 = CARTESIAN_POINT ( 'NONE',  ( -6.110151747013052647E-09, -9.999999993889911565, -4.800749288174391616 ) ) ;
#29940 = EDGE_CURVE ( 'NONE', #7050, #8787, #3397, .T. ) ;
#29941 = CARTESIAN_POINT ( 'NONE',  ( 162.0000000000000284, 7.960204194457768853E-16, 6.499999999999977796 ) ) ;
#29942 = CARTESIAN_POINT ( 'NONE',  ( -2.775557561562891351E-14, -5.500000000000115463, -122.2500000000000284 ) ) ;
#29943 = CARTESIAN_POINT ( 'NONE',  ( -5.999999999999944933, 1.607695154586759934, -145.4806624327026441 ) ) ;
#29944 = ORIENTED_EDGE ( 'NONE', *, *, #25590, .F. ) ;
#29945 = CARTESIAN_POINT ( 'NONE',  ( 22.50000000000015987, 1.873492889145067508, -1.873492889144956486 ) ) ;
#29946 = CARTESIAN_POINT ( 'NONE',  ( 0.000000000000000000, 5.999999999999977796, -105.2886751345948397 ) ) ;
#29947 = DIRECTION ( 'NONE',  ( -7.147005652999508048E-36, 5.642372883946980038E-36, 1.000000000000000000 ) ) ;
#29948 = EDGE_CURVE ( 'NONE', #8787, #124, #9894, .T. ) ;
#29949 = CARTESIAN_POINT ( 'NONE',  ( 142.5148502691896510, -3.535533905932725318, -3.535533905932725318 ) ) ;
#29950 = ORIENTED_EDGE ( 'NONE', *, *, #7956, .F. ) ;
#29951 = CARTESIAN_POINT ( 'NONE',  ( 111.1872167782375698, -1.849990392679472073, -0.7662911109075283278 ) ) ;
#29952 = CARTESIAN_POINT ( 'NONE',  ( 118.7113248654050750, 1.999999999999946265, 1.110223024625156540E-13 ) ) ;
#29953 = CARTESIAN_POINT ( 'NONE',  ( 111.6247167782376408, 1.849990392679523588, 0.000000000000000000 ) ) ;
#29954 = CARTESIAN_POINT ( 'NONE',  ( 3.608439182435180470, 6.249999999999982236, -113.6919872981078186 ) ) ;
#29955 = CARTESIAN_POINT ( 'NONE',  ( -5.196152422706573404, -3.000000000000002665, -110.2113248654051887 ) ) ;
#29956 = CARTESIAN_POINT ( 'NONE',  ( -5.999999999999963585, -1.487416814333745711E-14, -87.83632486540521711 ) ) ;
#29957 = VERTEX_POINT ( 'NONE', #6319 ) ;
#29958 = ORIENTED_EDGE ( 'NONE', *, *, #19530, .T. ) ;
#29959 = LINE ( 'NONE', #13733, #23338 ) ;
#29960 = CARTESIAN_POINT ( 'NONE',  ( 141.6562500000000284, -6.000000000000005329, 2.485281374238555774 ) ) ;
#29961 = VECTOR ( 'NONE', #15594, 1000.000000000000000 ) ;
#29962 = COLOUR_RGB ( '', 0.08235294, 0.09019608, 0.10196078) ;
#29963 = VERTEX_POINT ( 'NONE', #29197 ) ;
#29964 = CARTESIAN_POINT ( 'NONE',  ( 5.412658773652712085, -3.125000000000086153, -144.0669872981078470 ) ) ;
#29965 =( NAMED_UNIT ( * ) PLANE_ANGLE_UNIT ( ) SI_UNIT ( $, .RADIAN. ) );
#29966 = STYLED_ITEM ( 'NONE', ( #19512 ), #12132 ) ;
#29967 = DIRECTION ( 'NONE',  ( 0.000000000000000000, 0.000000000000000000, 1.000000000000000000 ) ) ;
#29968 = CARTESIAN_POINT ( 'NONE',  ( 24.56250000000017764, -1.999999999999911626, -0.8284271247462354770 ) ) ;
#29969 =( LENGTH_UNIT ( ) NAMED_UNIT ( * ) SI_UNIT ( .MILLI., .METRE. ) );
#29970 = CARTESIAN_POINT ( 'NONE',  ( 7.216878364870455975, -6.409875621278545621E-14, -63.80801270189225249 ) ) ;
#29971 = CARTESIAN_POINT ( 'NONE',  ( 142.2038997308104058, 2.071067811865468400, 4.999999999999989342 ) ) ;
#29972 = CARTESIAN_POINT ( 'NONE',  ( -5.196152422706601826, 2.999999999999975131, -102.0386751345948539 ) ) ;
#29973 = CYLINDRICAL_SURFACE ( 'NONE', #11392, 6.000000000000000888 ) ;
#29974 = CARTESIAN_POINT ( 'NONE',  ( 0.000000000000000000, 0.000000000000000000, 0.000000000000000000 ) ) ;
#29975 = FACE_OUTER_BOUND ( 'NONE', #1778, .T. ) ;
#29976 = CARTESIAN_POINT ( 'NONE',  ( 109.4374999999998863, -2.499999999999934719, 1.035533905932929599 ) ) ;
#29977 = EDGE_CURVE ( 'NONE', #1984, #16378, #17574, .T. ) ;
#29978 = CARTESIAN_POINT ( 'NONE',  ( 106.6011751345947118, -0.8284271247462053900, 2.000000000000271783 ) ) ;
#29979 = ADVANCED_FACE ( 'NONE', ( #22473 ), #24907, .T. ) ;
#29980 = CARTESIAN_POINT ( 'NONE',  ( -4.763139720814407951, 2.749999999999946709, -124.2500000000000284 ) ) ;
#29981 = CARTESIAN_POINT ( 'NONE',  ( 0.000000000000000000, 0.000000000000000000, 0.000000000000000000 ) ) ;
#29982 = CARTESIAN_POINT ( 'NONE',  ( 2.775557561562891351E-14, 6.250000000000033751, -144.4330127018922383 ) ) ;
#29983 = CARTESIAN_POINT ( 'NONE',  ( 16.16367513459493566, 1.767766952966487448, -1.767766952966431937 ) ) ;
#29984 = SURFACE_STYLE_USAGE ( .BOTH. , #9412 ) ;
#29985 = ORIENTED_EDGE ( 'NONE', *, *, #24748, .F. ) ;
#29986 = AXIS2_PLACEMENT_3D ( 'NONE', #26625, #17007, #7746 ) ;
#29987 = CARTESIAN_POINT ( 'NONE',  ( -6.350852961085760029, -1.281975124255709124E-13, -52.12500000000002842 ) ) ;
#29988 = FACE_OUTER_BOUND ( 'NONE', #20616, .T. ) ;
#29989 = CARTESIAN_POINT ( 'NONE',  ( -5.196152422706601826, 2.999999999999975131, -69.96132486540524553 ) ) ;
#29990 = DIRECTION ( 'NONE',  ( -0.000000000000000000, 1.000000000000000000, 0.000000000000000000 ) ) ;
#29991 = ORIENTED_EDGE ( 'NONE', *, *, #22118, .T. ) ;
#29992 = CARTESIAN_POINT ( 'NONE',  ( 104.8124999999997868, 1.035533905932779275, -2.499999999999904521 ) ) ;
#29993 = CARTESIAN_POINT ( 'NONE',  ( 138.4687500000000284, -2.485281374238585972, 6.000000000000005329 ) ) ;
#29994 = LINE ( 'NONE', #27677, #11159 ) ;
#29995 = CARTESIAN_POINT ( 'NONE',  ( 136.2187500000000284, 2.485281374238555774, -6.000000000000005329 ) ) ;
#29996 = CARTESIAN_POINT ( 'NONE',  ( -9.999999999999793943, 9.000000000000007105, -3.000000000000002665 ) ) ;
#29997 = CARTESIAN_POINT ( 'NONE',  ( 4.763139720814407951, -2.749999999999988454, -135.5000000000000000 ) ) ;
#29998 = ORIENTED_EDGE ( 'NONE', *, *, #332, .T. ) ;
#29999 = COLOUR_RGB ( '', 0.08235294, 0.09019608, 0.10196078) ;
#30000 = CARTESIAN_POINT ( 'NONE',  ( 11.43750000000003197, -1.999999999999911626, 0.8284271247462955401 ) ) ;
#30001 = EDGE_LOOP ( 'NONE', ( #21878, #4198, #14154, #12900 ) ) ;
#30002 = CARTESIAN_POINT ( 'NONE',  ( -6.350852961085760029, -1.281975124255709124E-13, -62.62500000000001421 ) ) ;
#30003 = VECTOR ( 'NONE', #26379, 1000.000000000000000 ) ;
#30004 = CARTESIAN_POINT ( 'NONE',  ( 18.03867513459492145, 1.665334536937734811E-13, -2.500000000000057732 ) ) ;
#30005 = CARTESIAN_POINT ( 'NONE',  ( 5.412658773652739619, 3.124999999999988898, -87.68301270189226670 ) ) ;
#30006 = EDGE_LOOP ( 'NONE', ( #18435, #28200, #7962, #21643 ) ) ;
#30007 = CARTESIAN_POINT ( 'NONE',  ( 105.2261751345946408, 2.000000000000062172, -0.8284271247459947807 ) ) ;
#30008 = CYLINDRICAL_SURFACE ( 'NONE', #15769, 6.000000000000000888 ) ;
#30009 = CARTESIAN_POINT ( 'NONE',  ( 129.9999999999998010, -89.00000000000001421, 3.000000000000002665 ) ) ;
#30010 = DIRECTION ( 'NONE',  ( 1.000000000000000000, -5.551115123125773458E-17, -1.260129944081490338E-35 ) ) ;
#30011 = CARTESIAN_POINT ( 'NONE',  ( 120.6252832217622881, 2.775557561562891351E-14, 1.849990392679523588 ) ) ;
#30012 = PRODUCT_CONTEXT ( 'NONE', #28880, 'mechanical' ) ;
#30013 =( BOUNDED_CURVE ( )  B_SPLINE_CURVE ( 2, ( #3877, #1273, #10686, #20030, #24316, #13308, #7885, #29377, #22029 ),
 .UNSPECIFIED., .F., .T. ) 
 B_SPLINE_CURVE_WITH_KNOTS ( ( 3, 2, 2, 2, 3 ),
 ( 0.5583333333333333481, 0.5592592592592592338, 0.5611111111111111160, 0.5629629629629628873, 0.5638888888888888840 ),
 .UNSPECIFIED. ) 
 CURVE ( )  GEOMETRIC_REPRESENTATION_ITEM ( )  RATIONAL_B_SPLINE_CURVE ( ( 0.9330127018922194093, 0.9330127018922234061, 1.000000000000000000, 0.8660254037844388186, 1.000000000000000000, 0.8660254037844388186, 1.000000000000000000, 0.9330127018922194093, 0.9330127018922194093 ) ) 
 REPRESENTATION_ITEM ( '' )  );
#30014 = EDGE_CURVE ( 'NONE', #27080, #22830, #12981, .T. ) ;
#30015 = CARTESIAN_POINT ( 'NONE',  ( 0.000000000000000000, 5.499999999999991118, -147.0000000000000284 ) ) ;
#30016 = CARTESIAN_POINT ( 'NONE',  ( 140.5000000000000284, -9.600000000000010303, -7.200000000000006395 ) ) ;
#30017 = CARTESIAN_POINT ( 'NONE',  ( -5.412658773652739619, 3.124999999999975131, -159.1830127018922667 ) ) ;
#30018 = CARTESIAN_POINT ( 'NONE',  ( 155.2425748654052313, -2.278174593052205932, -5.499999999999819700 ) ) ;
#30019 = CARTESIAN_POINT ( 'NONE',  ( 6.000000000000000888, -3.330669073875464691E-16, -7.560779664488942560E-35 ) ) ;
#30020 = PRODUCT ( 'Clamp rod', 'Clamp rod', '', ( #30012 ) ) ;
#30021 = CARTESIAN_POINT ( 'NONE',  ( -6.350852961085760029, -1.281975124255709124E-13, -80.62500000000001421 ) ) ;
#30022 = CARTESIAN_POINT ( 'NONE',  ( -5.999999999999963585, 1.780251999655701777E-13, -65.91367513459482552 ) ) ;
#30023 = CARTESIAN_POINT ( 'NONE',  ( 0.000000000000000000, 5.499999999999991118, -72.00000000000001421 ) ) ;
#30024 = CARTESIAN_POINT ( 'NONE',  ( -3.464101615137757051, -5.999999999999979572, -74.66367513459483973 ) ) ;
#30025 = CARTESIAN_POINT ( 'NONE',  ( 147.7648502691896510, 3.535533905932725318, 3.535533905932752852 ) ) ;
#30026 = CARTESIAN_POINT ( 'NONE',  ( -5.999999999999904965, -1.607695154586834541, -114.7693375672974412 ) ) ;
#30027 = DIRECTION ( 'NONE',  ( 1.000000000000000000, 0.000000000000000000, 0.000000000000000000 ) ) ;
#30028 = CARTESIAN_POINT ( 'NONE',  ( -5.999999999999963585, -1.487416814333745711E-14, -76.41367513459481131 ) ) ;
#30029 = CARTESIAN_POINT ( 'NONE',  ( 19.12500000000014211, 1.414213562373256572, 1.414213562373034527 ) ) ;
#30030 = LINE ( 'NONE', #18540, #29569 ) ;
#30031 = CARTESIAN_POINT ( 'NONE',  ( 116.6247167782376692, 1.849990392679523588, 0.000000000000000000 ) ) ;
#30032 = CARTESIAN_POINT ( 'NONE',  ( 0.000000000000000000, -5.999999999999991118, -97.96132486540520290 ) ) ;
#30033 = ORIENTED_EDGE ( 'NONE', *, *, #13655, .T. ) ;
#30034 = CARTESIAN_POINT ( 'NONE',  ( 153.1875000000000284, 4.242640687119269671, 4.242640687119298093 ) ) ;
#30035 = DIRECTION ( 'NONE',  ( -1.000000000000000000, -1.067522139062651904E-16, 0.000000000000000000 ) ) ;
#30036 = CARTESIAN_POINT ( 'NONE',  ( 11.77382486540525797, 2.500000000000144773, 1.035533905932689347 ) ) ;
#30037 = ORIENTED_EDGE ( 'NONE', *, *, #6689, .T. ) ;
#30038 = ORIENTED_EDGE ( 'NONE', *, *, #4604, .F. ) ;
#30039 = ORIENTED_EDGE ( 'NONE', *, *, #3756, .T. ) ;
#30040 = EDGE_CURVE ( 'NONE', #11659, #5958, #13061, .T. ) ;
#30041 = CARTESIAN_POINT ( 'NONE',  ( -3.175426480542816510, -5.500000000000057732, -96.87499999999997158 ) ) ;
#30042 = CARTESIAN_POINT ( 'NONE',  ( -7.216878364870328078, 0.000000000000000000, -103.5580127018922383 ) ) ;
#30043 = VERTEX_POINT ( 'NONE', #28117 ) ;
#30044 = DIRECTION ( 'NONE',  ( 1.260129944081490070E-35, 5.642372883946978702E-36, 1.000000000000000000 ) ) ;
#30045 = CARTESIAN_POINT ( 'NONE',  ( -5.999999999999963585, -1.487416814333745711E-14, -143.9136751345948255 ) ) ;
#30046 = CARTESIAN_POINT ( 'NONE',  ( 4.763139720814407951, -2.749999999999988454, -162.5000000000000284 ) ) ;
#30047 = CARTESIAN_POINT ( 'NONE',  ( 159.6488248654052029, -3.889087296526011706, -3.889087296526011706 ) ) ;
#30048 = ORIENTED_EDGE ( 'NONE', *, *, #20923, .F. ) ;
#30049 = CARTESIAN_POINT ( 'NONE',  ( 13.03867513459488947, 5.551115123125782702E-14, -2.500000000000002220 ) ) ;
#30050 = EDGE_CURVE ( 'NONE', #20271, #20037, #2266, .T. ) ;
#30051 = CARTESIAN_POINT ( 'NONE',  ( -4.763139720814407951, -2.750000000000016431, -170.4999999999999716 ) ) ;
#30052 = FACE_OUTER_BOUND ( 'NONE', #17603, .T. ) ;
#30053 = CARTESIAN_POINT ( 'NONE',  ( 6.350852961086080661, -9.614813431917819062E-14, -166.8750000000000568 ) ) ;
#30054 = CARTESIAN_POINT ( 'NONE',  ( 116.8749999999998863, 1.767766952966320915, -1.767766952966320915 ) ) ;
#30055 = CARTESIAN_POINT ( 'NONE',  ( -4.763139720814407951, -2.750000000000016431, -108.9999999999999858 ) ) ;
#30056 = CARTESIAN_POINT ( 'NONE',  ( 3.464101615137757051, -5.999999999999979572, -122.4136751345947971 ) ) ;
#30057 = CARTESIAN_POINT ( 'NONE',  ( -6.350852961085760029, -1.281975124255709124E-13, -94.12500000000004263 ) ) ;
#30058 = STYLED_ITEM ( 'NONE', ( #15149 ), #1155 ) ;
#30059 = CARTESIAN_POINT ( 'NONE',  ( 161.3586002691896795, 2.071067811865468400, 4.999999999999989342 ) ) ;
#30060 = CARTESIAN_POINT ( 'NONE',  ( 107.2113248654050608, -1.999999999999946265, 0.000000000000000000 ) ) ;
#30061 = ORIENTED_EDGE ( 'NONE', *, *, #14946, .F. ) ;
#30062 = CARTESIAN_POINT ( 'NONE',  ( 12.93750000000013145, -1.097466725451499370, 2.649519052838118061 ) ) ;
#30063 = CARTESIAN_POINT ( 'NONE',  ( 116.4999999999999574, -2.499999999999891198, 0.000000000000000000 ) ) ;
#30064 = CARTESIAN_POINT ( 'NONE',  ( 12.46132486540529882, 1.110223024625156540E-13, -2.500000000000057732 ) ) ;
#30065 = CARTESIAN_POINT ( 'NONE',  ( 107.4377832217621744, 1.849990392679562001, 0.7662911109080692285 ) ) ;
#30066 = CARTESIAN_POINT ( 'NONE',  ( 161.1037658773653050, -2.857005778783127844E-13, 5.603765877365280090 ) ) ;
#30067 = ORIENTED_EDGE ( 'NONE', *, *, #20488, .T. ) ;
#30068 = CARTESIAN_POINT ( 'NONE',  ( 116.0000000000000142, 0.000000000000000000, 0.000000000000000000 ) ) ;
#30069 = CARTESIAN_POINT ( 'NONE',  ( 107.7497167782375982, 1.308140751793668288, 1.308140751793640533 ) ) ;
#30070 = CARTESIAN_POINT ( 'NONE',  ( -7.216878364870328078, 0.000000000000000000, -89.19198729810783277 ) ) ;
#30071 = ORIENTED_EDGE ( 'NONE', *, *, #28235, .F. ) ;
#30072 = CARTESIAN_POINT ( 'NONE',  ( 106.7113248654050324, 2.000000000000001776, 1.110223024625156540E-13 ) ) ;
#30073 = VECTOR ( 'NONE', #24566, 1000.000000000000000 ) ;
#30074 = EDGE_CURVE ( 'NONE', #12110, #19914, #28520, .T. ) ;
#30075 = CARTESIAN_POINT ( 'NONE',  ( 150.1875000000000284, 4.242640687119269671, 4.242640687119298093 ) ) ;
#30076 = ORIENTED_EDGE ( 'NONE', *, *, #17139, .F. ) ;
#30077 = EDGE_CURVE ( 'NONE', #5616, #14191, #25608, .T. ) ;
#30078 = CARTESIAN_POINT ( 'NONE',  ( -4.763139720814407951, -2.750000000000016431, -124.0000000000000000 ) ) ;
#30079 = CARTESIAN_POINT ( 'NONE',  ( 22.12500000000006040, 1.665334536937734811E-13, -2.649519052838500421 ) ) ;
#30080 = CARTESIAN_POINT ( 'NONE',  ( -3.608439182435115633, 6.249999999999965361, -132.3080127018922383 ) ) ;
#30081 = VERTEX_POINT ( 'NONE', #30284 ) ;
#30082 = CARTESIAN_POINT ( 'NONE',  ( 158.8050748654052313, 5.500000000000012434, 2.278174593052012309 ) ) ;
#30083 = CARTESIAN_POINT ( 'NONE',  ( 5.412658773652739619, 3.124999999999988898, -167.8169872981077901 ) ) ;
#30084 = CARTESIAN_POINT ( 'NONE',  ( -3.608439182435115633, 6.249999999999965361, -173.4419872981078470 ) ) ;
#30085 = CARTESIAN_POINT ( 'NONE',  ( 159.0000000000000284, -11.07692307692308908, 4.615384615384620304 ) ) ;
#30086 = CARTESIAN_POINT ( 'NONE',  ( 107.7886751345947403, -1.999999999999835243, 1.110223024625156540E-13 ) ) ;
#30087 = EDGE_LOOP ( 'NONE', ( #15024, #18420, #10962, #10253 ) ) ;
#30088 = CARTESIAN_POINT ( 'NONE',  ( 13.75000000000006750, 2.220446049250313081E-13, -2.000000000000001776 ) ) ;
#30089 = EDGE_CURVE ( 'NONE', #18552, #856, #15335, .T. ) ;
#30090 = DIRECTION ( 'NONE',  ( 1.000000000000000000, -5.551115123125773458E-17, -1.260129944081490338E-35 ) ) ;
#30091 = CARTESIAN_POINT ( 'NONE',  ( 109.7261751345946408, -1.999999999999941602, 0.8284271247463557142 ) ) ;
#30092 = CYLINDRICAL_SURFACE ( 'NONE', #21676, 0.5000000000000000000 ) ;
#30093 = DIRECTION ( 'NONE',  ( 0.000000000000000000, 0.000000000000000000, 1.000000000000000000 ) ) ;
#30094 = CARTESIAN_POINT ( 'NONE',  ( 110.1877832217620750, 0.7662911109078588412, -1.849990392679411677 ) ) ;
#30095 = CARTESIAN_POINT ( 'NONE',  ( -3.608439182435052128, -6.250000000000110134, -76.94198729810784698 ) ) ;
#30096 = CARTESIAN_POINT ( 'NONE',  ( 5.412658773652739619, 3.124999999999988898, -61.31698729810780435 ) ) ;
#30097 = CARTESIAN_POINT ( 'NONE',  ( -2.775557561562891351E-14, -5.500000000000115463, -51.75000000000002132 ) ) ;
#30098 = CARTESIAN_POINT ( 'NONE',  ( -9.757819552369539906E-16, -9.499999999869134015, -4.869076758059751597 ) ) ;
#30099 = DIRECTION ( 'NONE',  ( 0.000000000000000000, 0.000000000000000000, -1.000000000000000000 ) ) ;
#30100 = CARTESIAN_POINT ( 'NONE',  ( -6.000000000000007105, -1.607695154586655129, -53.84668783648703538 ) ) ;
#30101 = CARTESIAN_POINT ( 'NONE',  ( -4.763139720814407951, -2.750000000000016431, -118.0000000000000000 ) ) ;
#30102 = DIRECTION ( 'NONE',  ( -7.147005652999508048E-36, 5.642372883946980038E-36, 1.000000000000000000 ) ) ;
#30103 = CIRCLE ( 'NONE', #20295, 5.500000000000000000 ) ;
#30104 = VERTEX_POINT ( 'NONE', #16355 ) ;
#30105 = CARTESIAN_POINT ( 'NONE',  ( 20.56250000000005684, 2.649519052838298805, -1.097466725451559322 ) ) ;
#30106 = FACE_OUTER_BOUND ( 'NONE', #27154, .T. ) ;
#30107 = FACE_OUTER_BOUND ( 'NONE', #18749, .T. ) ;
#30108 = VERTEX_POINT ( 'NONE', #6783 ) ;
#30109 = CARTESIAN_POINT ( 'NONE',  ( 110.7497167782376550, 1.308140751793640533, 1.308140751793640533 ) ) ;
#30110 = DIRECTION ( 'NONE',  ( -1.000000000000000000, -1.665334536937731113E-16, 1.526556658859586792E-16 ) ) ;
#30111 = CARTESIAN_POINT ( 'NONE',  ( 111.5622167782373566, 1.849990392679591977, -0.7662911109075283278 ) ) ;
#30112 = CARTESIAN_POINT ( 'NONE',  ( 7.216878364870455975, -6.409875621278545621E-14, -110.9419872981078186 ) ) ;
#30113 = CARTESIAN_POINT ( 'NONE',  ( 6.000000000000000888, -6.507448562710137091E-15, -176.1636751345947971 ) ) ;
#30114 =( BOUNDED_SURFACE ( )  B_SPLINE_SURFACE ( 1, 2, ( 
 ( #13195, #8061, #10552, #19909, #10875, #26501, #3447, #22068, #5455, #8216, #14862, #12882, #17632, #24205, #10724, #22219, #3152, #12579, #8382, #19611, #1000, #17792, #5911, #28953, #6077, #7917, #17330, #26646, #5605, #10403, #19757, #8855, #18394, #20369, #16264, #11023, #13803, #2092, #25110, #27871, #23304, #6840, #23149, #15804, #9005, #29579, #6533, #27408, #11175, #1623, #27257, #27712, #6692, #29720, #25583, #4070, #6229, #11497, #4376, #22684, #20838, #4537, #8698, #18092, #15648, #16112, #13492, #22831, #6373, #13339, #30187, #1772, #13962, #9153, #2248, #11650, #18546, #8536, #17942, #20524, #24958, #29876, #18238, #25415, #1931, #27555, #3911, #15956, #25254, #4226, #13644, #22989, #11337, #20682, #30034, #26029, #2973, #25879, #2828, #19137, #7584, #9762, #24029, #4834, #26174, #14261, #28324, #23884, #9307, #9464, #4976, #19002, #21440, #7303, #28614, #14684, #16561, #21590, #14544, #20997, #16707, #12251, #30343, #21142, #79, #23746, #23452, #9914, #16850, #4682, #5120, #18698, #521, #19290, #227, #2675, #16996, #14411, #18849, #12100, #23598, #28020, #25735, #14115, #11961, #372, #6993, #26319, #28472, #5276, #16413, #2391, #7439, #11803, #28173, #7143, #2535, #21287, #9613, #13000, #27074, #24620, #10068, #15134, #7884, #28918, #19581, #5876, #24463, #7735, #965, #17295, #5722, #10366, #6039, #22185, #15457, #19871, #26466, #17441, #8180, #29070, #17596, #3570, #15295, #1120, #26755, #26616, #28766, #5424, #21887, #29217, #19724, #8035, #26912, #3415, #22337, #1272, #24783, #10518, #8343, #12395, #20029, #21740, #10685, #17143, #17749, #24177, #24315, #14833, #680, #12841, #19443, #3122, #12543, #824, #10221, #5570, #14974, #3267, #12695, #22028, #13307, #1891, #6660, #3728, #22953, #20484, #18061, #13161, #10841, #27678, #4191, #6337, #27375, #16076, #23111, #29686, #1589, #22648, #15770, #29843, #16226, #25380, #4340, #8821, #8660, #8970, #20806, #13763, #18511, #29544, #22497, #18205, #2059, #27522, #11461, #6500, #18360, #25076, #6197, #30152, #4033, #15924, #25224, #6802, #9115, #13607, #13453, #1429, #11297, #20194, #27833, #20649, #8500, #29995, #17907, #22799, #27225, #15615, #24927, #3876, #10991, #14079, #9577, #23560, #25994, #11922, #2791, #19255, #21107, #26140, #19109, #7550, #21252, #16819, #25541, #25695, #4648, #28286, #27981, #14511, #21406, #9268, #337, #23266, #5085, #23851, #4796, #7267, #21557, #192, #23415, #18970, #28139, #2208, #18662, #6954, #4501, #13923, #12063 ),
 ( #28583, #12218, #14223, #14372, #16373, #485, #2360, #9733, #28433, #38, #9879, #11612, #20954, #7412, #11764, #4942, #9424, #2498, #18812, #7107, #16527, #25848, #23709, #2644, #16672, #8015, #7156, #18711, #14956, #26596, #14127, #12670, #17423, #2405, #11816, #28036, #7453, #16570, #14271, #23467, #4693, #22007, #9477, #26736, #945, #5703, #15112, #3242, #5551, #10344, #23613, #19705, #25894, #93, #19153, #23756, #28183, #21008, #29050, #4844, #24444, #11972, #3395, #383, #9776, #30354, #26045, #9319, #2546, #7005, #16424, #25746, #239, #2690, #21154, #7313, #18862, #16719, #21300, #9622, #19012, #28336, #4988, #14419, #17274, #12114, #21452, #28490, #24295, #8479, #17889, #22164, #6318, #1410, #15745, #15905, #1718, #22472, #1565, #3549, #29821, #24599, #27356, #25056, #8318, #11115, #6481, #20463, #4013, #29356, #22629, #12822, #20171, #10656, #24763, #15271, #10497, #10971, #20319, #12980, #8798, #17728, #19848, #13430, #18040, #5853, #22776, #18184, #22315, #1247, #29196, #29668, #27052, #6019, #20004, #26890, #27503, #15436, #25202, #1101, #8157, #17573, #3703, #13134, #10820, #29518, #27204, #6179, #15592, #8636, #24906, #3855, #13288, #16502, #9092, #25829, #25514, #7245, #14054, #23393, #11899, #9241, #16653, #18489, #4779, #2340, #21233, #11740, #4165, #27807, #9402, #6782, #11590, #7087, #22930, #23089, #18636, #2184, #4623, #20932, #176, #28265, #30130, #14202, #28116, #13589, #30283, #23540, #1870, #4325, #13743, #6932, #6632, #2479, #17, #18342, #18792, #9557, #27957, #16354, #11273, #18947, #2031, #25675, #20627, #29971, #11437, #21083, #8950, #27656, #16054, #25355, #16203, #20783, #4477, #13902, #23243, #28561, #9860, #28864, #14922, #12197, #23834, #14497, #7529, #21688, #7977, #17239, #7823, #12337, #464, #777, #12630, #26565, #10307, #21385, #25976, #624, #5515, #10008, #24259, #2919, #10158, #16940, #28414, #3207, #26269, #28708, #7681, #29012, #909, #19383, #21538, #4918, #17089, #14349, #5219, #26416, #23689, #21830, #5367, #21977, #19532, #19672, #3069, #14776, #26122, #19091, #2626, #12045, #319, #9708, #7394, #16802, #5069, #24120, #19233, #14633, #2770, #23978, #12493, #17384, #15072, #5664, #24415, #3357, #26701, #21341, #3025, #23941, #136, #21497, #12298, #2725, #21641, #7633, #19342, #5175, #423, #23651, #2447, #9520, #25933, #2878, #5024, #12152, #577, #23789, #9964, #5322, #10116, #26220, #12443, #19487, #24076, #28818, #14733, #11856, #28661, #28226, #28372 ) ),
 .UNSPECIFIED., .F., .F., .T. ) 
 B_SPLINE_SURFACE_WITH_KNOTS ( ( 2, 2 ),
 ( 3, 2, 2, 2, 2, 2, 2, 2, 2, 2, 2, 2, 2, 2, 2, 2, 2, 2, 2, 2, 2, 2, 2, 2, 2, 2, 2, 2, 2, 2, 2, 2, 2, 2, 2, 2, 2, 2, 2, 2, 2, 2, 2, 2, 2, 2, 2, 2, 2, 2, 2, 2, 2, 2, 2, 2, 2, 2, 2, 2, 2, 2, 2, 2, 2, 2, 2, 2, 2, 2, 2, 2, 2, 2, 2, 2, 2, 2, 2, 2, 2, 2, 2, 2, 2, 2, 2, 2, 2, 2, 2, 2, 2, 2, 2, 2, 2, 2, 2, 2, 2, 2, 2, 2, 2, 2, 2, 2, 2, 2, 2, 2, 2, 2, 2, 2, 2, 2, 2, 2, 2, 2, 2, 2, 2, 2, 2, 2, 2, 2, 2, 2, 2, 2, 2, 2, 2, 2, 2, 2, 2, 2, 2, 2, 2, 2, 2, 2, 2, 2, 2, 2, 2, 2, 2, 2, 2, 2, 2, 2, 3 ),
 ( 0.000000000000000000, 1.000000000000000000 ),
 ( 0.000000000000000000, 0.006250000000000000347, 0.01250000000000000069, 0.01874999999999999931, 0.02500000000000000139, 0.03125000000000000000, 0.03749999999999999861, 0.04374999999999999722, 0.05000000000000000278, 0.05625000000000000139, 0.06250000000000000000, 0.06875000000000000555, 0.07499999999999999722, 0.08125000000000000278, 0.08749999999999999445, 0.09375000000000000000, 0.1000000000000000056, 0.1062499999999999972, 0.1125000000000000028, 0.1187499999999999944, 0.1250000000000000000, 0.1312500000000000056, 0.1375000000000000111, 0.1437499999999999889, 0.1499999999999999944, 0.1562500000000000000, 0.1625000000000000056, 0.1687500000000000111, 0.1749999999999999889, 0.1812499999999999944, 0.1875000000000000000, 0.1937500000000000056, 0.2000000000000000111, 0.2062499999999999889, 0.2124999999999999944, 0.2187500000000000000, 0.2250000000000000056, 0.2312500000000000111, 0.2374999999999999889, 0.2437499999999999944, 0.2500000000000000000, 0.2562499999999999778, 0.2625000000000000111, 0.2687499999999999889, 0.2750000000000000222, 0.2812500000000000000, 0.2874999999999999778, 0.2937500000000000111, 0.2999999999999999889, 0.3062500000000000222, 0.3125000000000000000, 0.3187499999999999778, 0.3250000000000000111, 0.3312499999999999889, 0.3375000000000000222, 0.3437500000000000000, 0.3499999999999999778, 0.3562500000000000111, 0.3624999999999999889, 0.3687500000000000222, 0.3750000000000000000, 0.3812499999999999778, 0.3875000000000000111, 0.3937499999999999889, 0.4000000000000000222, 0.4062500000000000000, 0.4124999999999999778, 0.4187500000000000111, 0.4249999999999999889, 0.4312500000000000222, 0.4375000000000000000, 0.4437499999999999778, 0.4500000000000000111, 0.4562499999999999889, 0.4625000000000000222, 0.4687500000000000000, 0.4749999999999999778, 0.4812500000000000111, 0.4874999999999999889, 0.4937500000000000222, 0.5000000000000000000, 0.5062499999999999778, 0.5124999999999999556, 0.5187500000000000444, 0.5250000000000000222, 0.5312500000000000000, 0.5374999999999999778, 0.5437499999999999556, 0.5500000000000000444, 0.5562500000000000222, 0.5625000000000000000, 0.5687499999999999778, 0.5749999999999999556, 0.5812500000000000444, 0.5875000000000000222, 0.5937500000000000000, 0.5999999999999999778, 0.6062499999999999556, 0.6125000000000000444, 0.6187500000000000222, 0.6250000000000000000, 0.6312499999999999778, 0.6374999999999999556, 0.6437500000000000444, 0.6500000000000000222, 0.6562500000000000000, 0.6624999999999999778, 0.6687499999999999556, 0.6750000000000000444, 0.6812500000000000222, 0.6875000000000000000, 0.6937499999999999778, 0.6999999999999999556, 0.7062500000000000444, 0.7125000000000000222, 0.7187500000000000000, 0.7249999999999999778, 0.7312499999999999556, 0.7375000000000000444, 0.7437500000000000222, 0.7500000000000000000, 0.7562499999999999778, 0.7624999999999999556, 0.7687500000000000444, 0.7750000000000000222, 0.7812500000000000000, 0.7874999999999999778, 0.7937499999999999556, 0.8000000000000000444, 0.8062500000000000222, 0.8125000000000000000, 0.8187499999999999778, 0.8249999999999999556, 0.8312500000000000444, 0.8375000000000000222, 0.8437500000000000000, 0.8499999999999999778, 0.8562499999999999556, 0.8625000000000000444, 0.8687500000000000222, 0.8750000000000000000, 0.8812499999999999778, 0.8874999999999999556, 0.8937500000000000444, 0.9000000000000000222, 0.9062500000000000000, 0.9124999999999999778, 0.9187499999999999556, 0.9250000000000000444, 0.9312500000000000222, 0.9375000000000000000, 0.9437499999999999778, 0.9499999999999999556, 0.9562500000000000444, 0.9625000000000000222, 0.9687500000000000000, 0.9749999999999999778, 0.9812499999999999556, 0.9875000000000000444, 0.9937500000000000222, 1.000000000000000000 ),
 .UNSPECIFIED. ) 
 GEOMETRIC_REPRESENTATION_ITEM ( )  RATIONAL_B_SPLINE_SURFACE ( (
 ( 1.000000000000000000, 0.9238795325112867385, 1.000000000000000000, 0.9238795325112867385, 1.000000000000000000, 0.9238795325112867385, 1.000000000000000000, 0.9238795325112867385, 1.000000000000000000, 0.9238795325112867385, 1.000000000000000000, 0.9238795325112867385, 1.000000000000000000, 0.9238795325112867385, 1.000000000000000000, 0.9238795325112867385, 1.000000000000000000, 0.9238795325112867385, 1.000000000000000000, 0.9238795325112867385, 1.000000000000000000, 0.9238795325112867385, 1.000000000000000000, 0.9238795325112867385, 1.000000000000000000, 0.9238795325112867385, 1.000000000000000000, 0.9238795325112867385, 1.000000000000000000, 0.9238795325112867385, 1.000000000000000000, 0.9238795325112867385, 1.000000000000000000, 0.9238795325112867385, 1.000000000000000000, 0.9238795325112867385, 1.000000000000000000, 0.9238795325112867385, 1.000000000000000000, 0.9238795325112867385, 1.000000000000000000, 0.9238795325112867385, 1.000000000000000000, 0.9238795325112867385, 1.000000000000000000, 0.9238795325112867385, 1.000000000000000000, 0.9238795325112867385, 1.000000000000000000, 0.9238795325112867385, 1.000000000000000000, 0.9238795325112867385, 1.000000000000000000, 0.9238795325112867385, 1.000000000000000000, 0.9238795325112867385, 1.000000000000000000, 0.9238795325112867385, 1.000000000000000000, 0.9238795325112867385, 1.000000000000000000, 0.9238795325112867385, 1.000000000000000000, 0.9238795325112867385, 1.000000000000000000, 0.9238795325112867385, 1.000000000000000000, 0.9238795325112867385, 1.000000000000000000, 0.9238795325112867385, 1.000000000000000000, 0.9238795325112867385, 1.000000000000000000, 0.9238795325112867385, 1.000000000000000000, 0.9238795325112867385, 1.000000000000000000, 0.9238795325112867385, 1.000000000000000000, 0.9238795325112867385, 1.000000000000000000, 0.9238795325112867385, 1.000000000000000000, 0.9238795325112867385, 1.000000000000000000, 0.9238795325112867385, 1.000000000000000000, 0.9238795325112867385, 1.000000000000000000, 0.9238795325112867385, 1.000000000000000000, 0.9238795325112867385, 1.000000000000000000, 0.9238795325112867385, 1.000000000000000000, 0.9238795325112867385, 1.000000000000000000, 0.9238795325112867385, 1.000000000000000000, 0.9238795325112867385, 1.000000000000000000, 0.9238795325112867385, 1.000000000000000000, 0.9238795325112867385, 1.000000000000000000, 0.9238795325112867385, 1.000000000000000000, 0.9238795325112867385, 1.000000000000000000, 0.9238795325112867385, 1.000000000000000000, 0.9238795325112867385, 1.000000000000000000, 0.9238795325112867385, 1.000000000000000000, 0.9238795325112867385, 1.000000000000000000, 0.9238795325112867385, 1.000000000000000000, 0.9238795325112867385, 1.000000000000000000, 0.9238795325112867385, 1.000000000000000000, 0.9238795325112867385, 1.000000000000000000, 0.9238795325112867385, 1.000000000000000000, 0.9238795325112867385, 1.000000000000000000, 0.9238795325112867385, 1.000000000000000000, 0.9238795325112867385, 1.000000000000000000, 0.9238795325112867385, 1.000000000000000000, 0.9238795325112867385, 1.000000000000000000, 0.9238795325112867385, 1.000000000000000000, 0.9238795325112867385, 1.000000000000000000, 0.9238795325112867385, 1.000000000000000000, 0.9238795325112867385, 1.000000000000000000, 0.9238795325112867385, 1.000000000000000000, 0.9238795325112867385, 1.000000000000000000, 0.9238795325112867385, 1.000000000000000000, 0.9238795325112867385, 1.000000000000000000, 0.9238795325112867385, 1.000000000000000000, 0.9238795325112867385, 1.000000000000000000, 0.9238795325112867385, 1.000000000000000000, 0.9238795325112867385, 1.000000000000000000, 0.9238795325112867385, 1.000000000000000000, 0.9238795325112867385, 1.000000000000000000, 0.9238795325112867385, 1.000000000000000000, 0.9238795325112867385, 1.000000000000000000, 0.9238795325112867385, 1.000000000000000000, 0.9238795325112867385, 1.000000000000000000, 0.9238795325112867385, 1.000000000000000000, 0.9238795325112867385, 1.000000000000000000, 0.9238795325112867385, 1.000000000000000000, 0.9238795325112867385, 1.000000000000000000, 0.9238795325112867385, 1.000000000000000000, 0.9238795325112867385, 1.000000000000000000, 0.9238795325112867385, 1.000000000000000000, 0.9238795325112867385, 1.000000000000000000, 0.9238795325112867385, 1.000000000000000000, 0.9238795325112867385, 1.000000000000000000, 0.9238795325112867385, 1.000000000000000000, 0.9238795325112867385, 1.000000000000000000, 0.9238795325112867385, 1.000000000000000000, 0.9238795325112867385, 1.000000000000000000, 0.9238795325112867385, 1.000000000000000000, 0.9238795325112867385, 1.000000000000000000, 0.9238795325112867385, 1.000000000000000000, 0.9238795325112867385, 1.000000000000000000, 0.9238795325112867385, 1.000000000000000000, 0.9238795325112867385, 1.000000000000000000, 0.9238795325112867385, 1.000000000000000000, 0.9238795325112867385, 1.000000000000000000, 0.9238795325112867385, 1.000000000000000000, 0.9238795325112867385, 1.000000000000000000, 0.9238795325112867385, 1.000000000000000000, 0.9238795325112867385, 1.000000000000000000, 0.9238795325112867385, 1.000000000000000000, 0.9238795325112867385, 1.000000000000000000, 0.9238795325112867385, 1.000000000000000000, 0.9238795325112867385, 1.000000000000000000, 0.9238795325112867385, 1.000000000000000000, 0.9238795325112867385, 1.000000000000000000, 0.9238795325112867385, 1.000000000000000000, 0.9238795325112867385, 1.000000000000000000, 0.9238795325112867385, 1.000000000000000000, 0.9238795325112867385, 1.000000000000000000, 0.9238795325112867385, 1.000000000000000000, 0.9238795325112867385, 1.000000000000000000, 0.9238795325112867385, 1.000000000000000000, 0.9238795325112867385, 1.000000000000000000, 0.9238795325112867385, 1.000000000000000000, 0.9238795325112867385, 1.000000000000000000, 0.9238795325112867385, 1.000000000000000000, 0.9238795325112867385, 1.000000000000000000, 0.9238795325112867385, 1.000000000000000000, 0.9238795325112867385, 1.000000000000000000, 0.9238795325112867385, 1.000000000000000000, 0.9238795325112867385, 1.000000000000000000, 0.9238795325112867385, 1.000000000000000000, 0.9238795325112867385, 1.000000000000000000, 0.9238795325112867385, 1.000000000000000000, 0.9238795325112867385, 1.000000000000000000, 0.9238795325112867385, 1.000000000000000000, 0.9238795325112867385, 1.000000000000000000, 0.9238795325112867385, 1.000000000000000000, 0.9238795325112867385, 1.000000000000000000, 0.9238795325112867385, 1.000000000000000000, 0.9238795325112867385, 1.000000000000000000, 0.9238795325112867385, 1.000000000000000000, 0.9238795325112867385, 1.000000000000000000, 0.9238795325112867385, 1.000000000000000000, 0.9238795325112867385, 1.000000000000000000, 0.9238795325112867385, 1.000000000000000000, 0.9238795325112867385, 1.000000000000000000, 0.9238795325112867385, 1.000000000000000000, 0.9238795325112867385, 1.000000000000000000, 0.9238795325112867385, 1.000000000000000000, 0.9238795325112867385, 1.000000000000000000, 0.9238795325112867385, 1.000000000000000000, 0.9238795325112867385, 1.000000000000000000, 0.9238795325112867385, 1.000000000000000000, 0.9238795325112867385, 1.000000000000000000, 0.9238795325112867385, 1.000000000000000000, 0.9238795325112867385, 1.000000000000000000),
 ( 1.000000000000000000, 0.9238795325112867385, 1.000000000000000000, 0.9238795325112867385, 1.000000000000000000, 0.9238795325112867385, 1.000000000000000000, 0.9238795325112867385, 1.000000000000000000, 0.9238795325112867385, 1.000000000000000000, 0.9238795325112867385, 1.000000000000000000, 0.9238795325112867385, 1.000000000000000000, 0.9238795325112867385, 1.000000000000000000, 0.9238795325112867385, 1.000000000000000000, 0.9238795325112867385, 1.000000000000000000, 0.9238795325112867385, 1.000000000000000000, 0.9238795325112867385, 1.000000000000000000, 0.9238795325112867385, 1.000000000000000000, 0.9238795325112867385, 1.000000000000000000, 0.9238795325112867385, 1.000000000000000000, 0.9238795325112867385, 1.000000000000000000, 0.9238795325112867385, 1.000000000000000000, 0.9238795325112867385, 1.000000000000000000, 0.9238795325112867385, 1.000000000000000000, 0.9238795325112867385, 1.000000000000000000, 0.9238795325112867385, 1.000000000000000000, 0.9238795325112867385, 1.000000000000000000, 0.9238795325112867385, 1.000000000000000000, 0.9238795325112867385, 1.000000000000000000, 0.9238795325112867385, 1.000000000000000000, 0.9238795325112867385, 1.000000000000000000, 0.9238795325112867385, 1.000000000000000000, 0.9238795325112867385, 1.000000000000000000, 0.9238795325112867385, 1.000000000000000000, 0.9238795325112867385, 1.000000000000000000, 0.9238795325112867385, 1.000000000000000000, 0.9238795325112867385, 1.000000000000000000, 0.9238795325112867385, 1.000000000000000000, 0.9238795325112867385, 1.000000000000000000, 0.9238795325112867385, 1.000000000000000000, 0.9238795325112867385, 1.000000000000000000, 0.9238795325112867385, 1.000000000000000000, 0.9238795325112867385, 1.000000000000000000, 0.9238795325112867385, 1.000000000000000000, 0.9238795325112867385, 1.000000000000000000, 0.9238795325112867385, 1.000000000000000000, 0.9238795325112867385, 1.000000000000000000, 0.9238795325112867385, 1.000000000000000000, 0.9238795325112867385, 1.000000000000000000, 0.9238795325112867385, 1.000000000000000000, 0.9238795325112867385, 1.000000000000000000, 0.9238795325112867385, 1.000000000000000000, 0.9238795325112867385, 1.000000000000000000, 0.9238795325112867385, 1.000000000000000000, 0.9238795325112867385, 1.000000000000000000, 0.9238795325112867385, 1.000000000000000000, 0.9238795325112867385, 1.000000000000000000, 0.9238795325112867385, 1.000000000000000000, 0.9238795325112867385, 1.000000000000000000, 0.9238795325112867385, 1.000000000000000000, 0.9238795325112867385, 1.000000000000000000, 0.9238795325112867385, 1.000000000000000000, 0.9238795325112867385, 1.000000000000000000, 0.9238795325112867385, 1.000000000000000000, 0.9238795325112867385, 1.000000000000000000, 0.9238795325112867385, 1.000000000000000000, 0.9238795325112867385, 1.000000000000000000, 0.9238795325112867385, 1.000000000000000000, 0.9238795325112867385, 1.000000000000000000, 0.9238795325112867385, 1.000000000000000000, 0.9238795325112867385, 1.000000000000000000, 0.9238795325112867385, 1.000000000000000000, 0.9238795325112867385, 1.000000000000000000, 0.9238795325112867385, 1.000000000000000000, 0.9238795325112867385, 1.000000000000000000, 0.9238795325112867385, 1.000000000000000000, 0.9238795325112867385, 1.000000000000000000, 0.9238795325112867385, 1.000000000000000000, 0.9238795325112867385, 1.000000000000000000, 0.9238795325112867385, 1.000000000000000000, 0.9238795325112867385, 1.000000000000000000, 0.9238795325112867385, 1.000000000000000000, 0.9238795325112867385, 1.000000000000000000, 0.9238795325112867385, 1.000000000000000000, 0.9238795325112867385, 1.000000000000000000, 0.9238795325112867385, 1.000000000000000000, 0.9238795325112867385, 1.000000000000000000, 0.9238795325112867385, 1.000000000000000000, 0.9238795325112867385, 1.000000000000000000, 0.9238795325112867385, 1.000000000000000000, 0.9238795325112867385, 1.000000000000000000, 0.9238795325112867385, 1.000000000000000000, 0.9238795325112867385, 1.000000000000000000, 0.9238795325112867385, 1.000000000000000000, 0.9238795325112867385, 1.000000000000000000, 0.9238795325112867385, 1.000000000000000000, 0.9238795325112867385, 1.000000000000000000, 0.9238795325112867385, 1.000000000000000000, 0.9238795325112867385, 1.000000000000000000, 0.9238795325112867385, 1.000000000000000000, 0.9238795325112867385, 1.000000000000000000, 0.9238795325112867385, 1.000000000000000000, 0.9238795325112867385, 1.000000000000000000, 0.9238795325112867385, 1.000000000000000000, 0.9238795325112867385, 1.000000000000000000, 0.9238795325112867385, 1.000000000000000000, 0.9238795325112867385, 1.000000000000000000, 0.9238795325112867385, 1.000000000000000000, 0.9238795325112867385, 1.000000000000000000, 0.9238795325112867385, 1.000000000000000000, 0.9238795325112867385, 1.000000000000000000, 0.9238795325112867385, 1.000000000000000000, 0.9238795325112867385, 1.000000000000000000, 0.9238795325112867385, 1.000000000000000000, 0.9238795325112867385, 1.000000000000000000, 0.9238795325112867385, 1.000000000000000000, 0.9238795325112867385, 1.000000000000000000, 0.9238795325112867385, 1.000000000000000000, 0.9238795325112867385, 1.000000000000000000, 0.9238795325112867385, 1.000000000000000000, 0.9238795325112867385, 1.000000000000000000, 0.9238795325112867385, 1.000000000000000000, 0.9238795325112867385, 1.000000000000000000, 0.9238795325112867385, 1.000000000000000000, 0.9238795325112867385, 1.000000000000000000, 0.9238795325112867385, 1.000000000000000000, 0.9238795325112867385, 1.000000000000000000, 0.9238795325112867385, 1.000000000000000000, 0.9238795325112867385, 1.000000000000000000, 0.9238795325112867385, 1.000000000000000000, 0.9238795325112867385, 1.000000000000000000, 0.9238795325112867385, 1.000000000000000000, 0.9238795325112867385, 1.000000000000000000, 0.9238795325112867385, 1.000000000000000000, 0.9238795325112867385, 1.000000000000000000, 0.9238795325112867385, 1.000000000000000000, 0.9238795325112867385, 1.000000000000000000, 0.9238795325112867385, 1.000000000000000000, 0.9238795325112867385, 1.000000000000000000, 0.9238795325112867385, 1.000000000000000000, 0.9238795325112867385, 1.000000000000000000, 0.9238795325112867385, 1.000000000000000000, 0.9238795325112867385, 1.000000000000000000, 0.9238795325112867385, 1.000000000000000000, 0.9238795325112867385, 1.000000000000000000, 0.9238795325112867385, 1.000000000000000000, 0.9238795325112867385, 1.000000000000000000, 0.9238795325112867385, 1.000000000000000000, 0.9238795325112867385, 1.000000000000000000, 0.9238795325112867385, 1.000000000000000000, 0.9238795325112867385, 1.000000000000000000, 0.9238795325112867385, 1.000000000000000000, 0.9238795325112867385, 1.000000000000000000, 0.9238795325112867385, 1.000000000000000000, 0.9238795325112867385, 1.000000000000000000, 0.9238795325112867385, 1.000000000000000000, 0.9238795325112867385, 1.000000000000000000, 0.9238795325112867385, 1.000000000000000000, 0.9238795325112867385, 1.000000000000000000, 0.9238795325112867385, 1.000000000000000000, 0.9238795325112867385, 1.000000000000000000, 0.9238795325112867385, 1.000000000000000000, 0.9238795325112867385, 1.000000000000000000, 0.9238795325112867385, 1.000000000000000000, 0.9238795325112867385, 1.000000000000000000) ) ) 
 REPRESENTATION_ITEM ( '' )  SURFACE ( )  );
#30115 = CARTESIAN_POINT ( 'NONE',  ( 10.00000000000017053, -0.2656921846150581690, 2.453244723652735271 ) ) ;
#30116 = ORIENTED_EDGE ( 'NONE', *, *, #30294, .T. ) ;
#30117 = ORIENTED_EDGE ( 'NONE', *, *, #6227, .F. ) ;
#30118 = DIRECTION ( 'NONE',  ( 1.000000000000000000, 0.000000000000000000, 0.000000000000000000 ) ) ;
#30119 = CARTESIAN_POINT ( 'NONE',  ( 135.9375000000000568, -4.242640687119298093, -4.242640687119298093 ) ) ;
#30120 = ADVANCED_FACE ( 'NONE', ( #30131 ), #11438, .T. ) ;
#30121 = ORIENTED_EDGE ( 'NONE', *, *, #6262, .T. ) ;
#30122 = CARTESIAN_POINT ( 'NONE',  ( 2.775557561562891351E-14, -6.250000000000061284, -136.8169872981078186 ) ) ;
#30123 = SURFACE_STYLE_USAGE ( .BOTH. , #18482 ) ;
#30124 = CARTESIAN_POINT ( 'NONE',  ( 5.196152422706629359, 3.000000000000002665, -151.4613248654052029 ) ) ;
#30125 = CARTESIAN_POINT ( 'NONE',  ( 21.18750000000019540, 0.8284271247462955401, 2.000000000000031530 ) ) ;
#30126 = CARTESIAN_POINT ( 'NONE',  ( 0.000000000000000000, 5.999999999999977796, -120.2886751345948539 ) ) ;
#30127 = EDGE_CURVE ( 'NONE', #29780, #5395, #25584, .T. ) ;
#30128 = CARTESIAN_POINT ( 'NONE',  ( 2.775557561562891351E-14, -6.250000000000061284, -67.18301270189225249 ) ) ;
#30129 = EDGE_CURVE ( 'NONE', #3793, #11265, #6741, .T. ) ;
#30130 = CARTESIAN_POINT ( 'NONE',  ( 144.3601497308104058, -3.535533905932725318, -3.535533905932725318 ) ) ;
#30131 = FACE_OUTER_BOUND ( 'NONE', #15172, .T. ) ;
#30132 = CARTESIAN_POINT ( 'NONE',  ( -5.999999999999963585, 1.780251999655701777E-13, -73.41367513459483973 ) ) ;
#30133 = DIRECTION ( 'NONE',  ( -7.147005652999508048E-36, 5.642372883946980038E-36, 1.000000000000000000 ) ) ;
#30134 = CARTESIAN_POINT ( 'NONE',  ( 24.70360430863998502, -2.251580690448135247, -0.4762138706651334319 ) ) ;
#30135 = CARTESIAN_POINT ( 'NONE',  ( -3.464101615137757051, -5.999999999999979572, -67.16367513459479710 ) ) ;
#30136 = CARTESIAN_POINT ( 'NONE',  ( 111.4999999999998863, -2.499999999999946709, 1.110223024625156540E-13 ) ) ;
#30137 = LINE ( 'NONE', #2347, #23615 ) ;
#30138 = CARTESIAN_POINT ( 'NONE',  ( 3.175426480543072749, -5.500000000000105693, -126.6249999999999858 ) ) ;
#30139 = FILL_AREA_STYLE_COLOUR ( '', #9767 ) ;
#30140 = CARTESIAN_POINT ( 'NONE',  ( 3.608439182435180470, -6.249999999999997335, -145.0580127018922383 ) ) ;
#30141 = DIRECTION ( 'NONE',  ( 1.000000000000000000, -0.000000000000000000, -0.000000000000000000 ) ) ;
#30142 = DIRECTION ( 'NONE',  ( 1.000000000000000000, -0.000000000000000000, -0.000000000000000000 ) ) ;
#30143 = EDGE_LOOP ( 'NONE', ( #15410, #15614, #22079, #10963 ) ) ;
#30144 = CARTESIAN_POINT ( 'NONE',  ( 4.763139720814407951, -2.749999999999988454, -51.49999999999999289 ) ) ;
#30145 = DIRECTION ( 'NONE',  ( -1.000000000000000000, -0.000000000000000000, -0.000000000000000000 ) ) ;
#30146 = CARTESIAN_POINT ( 'NONE',  ( -5.999999999999963585, 1.780251999655701777E-13, -69.83632486540523132 ) ) ;
#30147 = CARTESIAN_POINT ( 'NONE',  ( 6.000000000000000888, -3.330669073875464691E-16, -7.560779664488942560E-35 ) ) ;
#30148 = ORIENTED_EDGE ( 'NONE', *, *, #3229, .T. ) ;
#30149 = CARTESIAN_POINT ( 'NONE',  ( 140.7187500000000284, 2.485281374238556218, -6.000000000000005329 ) ) ;
#30150 = CARTESIAN_POINT ( 'NONE',  ( 159.9743574244512843, -12.51706875447920275, -3.259670390775218696 ) ) ;
#30151 = CARTESIAN_POINT ( 'NONE',  ( -5.999999999999971578, 1.607695154586715303, -176.4033121635129930 ) ) ;
#30152 = CARTESIAN_POINT ( 'NONE',  ( 137.5312500000000284, -2.485281374238555774, -6.000000000000005329 ) ) ;
#30153 = CARTESIAN_POINT ( 'NONE',  ( 119.8124999999998721, 1.035533905932839227, -2.499999999999844569 ) ) ;
#30154 =( BOUNDED_CURVE ( )  B_SPLINE_CURVE ( 2, ( #26968, #8400, #5774, #3621, #3468, #19635, #7938, #26123, #10421 ),
 .UNSPECIFIED., .F., .F. ) 
 B_SPLINE_CURVE_WITH_KNOTS ( ( 3, 2, 2, 2, 3 ),
 ( 0.6470588235294116863, 0.6544117647058823595, 0.6617647058823529216, 0.6691176470588235947, 0.6764705882352941568 ),
 .UNSPECIFIED. ) 
 CURVE ( )  GEOMETRIC_REPRESENTATION_ITEM ( )  RATIONAL_B_SPLINE_CURVE ( ( 1.000000000000000000, 0.9238795325112867385, 1.000000000000000000, 0.9238795325112867385, 1.000000000000000000, 0.9238795325112867385, 1.000000000000000000, 0.9238795325112867385, 1.000000000000000000 ) ) 
 REPRESENTATION_ITEM ( '' )  );
#30155 = ADVANCED_FACE ( 'NONE', ( #13744 ), #177, .T. ) ;
#30156 = CARTESIAN_POINT ( 'NONE',  ( 3.175426480543072749, -5.500000000000105693, -137.1250000000000568 ) ) ;
#30157 = VERTEX_POINT ( 'NONE', #2032 ) ;
#30158 = CARTESIAN_POINT ( 'NONE',  ( 12.75000000000017764, 1.665334536937734811E-13, -2.000000000000001776 ) ) ;
#30159 = ORIENTED_EDGE ( 'NONE', *, *, #19742, .T. ) ;
#30160 = CARTESIAN_POINT ( 'NONE',  ( -6.350852961085760029, -1.281975124255709124E-13, -68.62500000000004263 ) ) ;
#30161 = EDGE_CURVE ( 'NONE', #3569, #12154, #19319, .T. ) ;
#30162 = CARTESIAN_POINT ( 'NONE',  ( -5.412658773652739619, 3.124999999999975131, -88.68301270189226670 ) ) ;
#30163 = ORIENTED_EDGE ( 'NONE', *, *, #28612, .T. ) ;
#30164 = CARTESIAN_POINT ( 'NONE',  ( -11.00000000000000000, 1.957734142605923910E-15, -14.99152654425661702 ) ) ;
#30165 =( LENGTH_UNIT ( ) NAMED_UNIT ( * ) SI_UNIT ( .MILLI., .METRE. ) );
#30166 = CARTESIAN_POINT ( 'NONE',  ( 140.0769230769231228, -11.53846153846154898, -4.615384615384614087 ) ) ;
#30167 = CARTESIAN_POINT ( 'NONE',  ( 119.0002832217622455, -1.308140751793585022, -1.308140751793529510 ) ) ;
#30168 = CARTESIAN_POINT ( 'NONE',  ( 4.763139720814407951, 2.750000000000002665, -147.2500000000000000 ) ) ;
#30169 = CARTESIAN_POINT ( 'NONE',  ( 139.7785334105569461, -9.309084377508947128, -7.921262206628336244 ) ) ;
#30170 = TOROIDAL_SURFACE ( 'NONE', #16962, 14.49999999999999289, 0.5000000000000000000 ) ;
#30171 = CARTESIAN_POINT ( 'NONE',  ( 7.216878364870455975, -6.409875621278545621E-14, -159.8080127018922667 ) ) ;
#30172 = PRESENTATION_STYLE_ASSIGNMENT (( #26013 ) ) ;
#30173 = CARTESIAN_POINT ( 'NONE',  ( 3.464101615137852974, 5.999999999999884537, -89.83632486540521711 ) ) ;
#30174 = CARTESIAN_POINT ( 'NONE',  ( -4.763139720814407951, -2.750000000000016431, -76.00000000000001421 ) ) ;
#30175 = CARTESIAN_POINT ( 'NONE',  ( 116.7113248654051318, 2.000000000000057288, 0.000000000000000000 ) ) ;
#30176 = CARTESIAN_POINT ( 'NONE',  ( -4.763139720814407951, 2.749999999999946709, -76.25000000000004263 ) ) ;
#30177 = CARTESIAN_POINT ( 'NONE',  ( 139.9672529042787517, -9.668691406906541275, 7.713138574913902978 ) ) ;
#30178 = CARTESIAN_POINT ( 'NONE',  ( -39.00000000000000000, -20.00000000000021316, 3.000000000000002665 ) ) ;
#30179 = CARTESIAN_POINT ( 'NONE',  ( 156.7500000000000284, -6.000000000000005329, 0.000000000000000000 ) ) ;
#30180 = CARTESIAN_POINT ( 'NONE',  ( 144.0863248654052313, 0.000000000000000000, 5.500000000000005329 ) ) ;
#30181 = VECTOR ( 'NONE', #23295, 1000.000000000000000 ) ;
#30182 = CARTESIAN_POINT ( 'NONE',  ( 140.6185434356032715, -11.23708687120643646, -4.230991509104588211 ) ) ;
#30183 = LINE ( 'NONE', #75, #30278 ) ;
#30184 = CARTESIAN_POINT ( 'NONE',  ( 118.6247167782376408, 1.849990392679468076, 0.000000000000000000 ) ) ;
#30185 = FACE_OUTER_BOUND ( 'NONE', #21371, .T. ) ;
#30186 = ORIENTED_EDGE ( 'NONE', *, *, #18645, .T. ) ;
#30187 = CARTESIAN_POINT ( 'NONE',  ( 155.4375000000000284, -4.242640687119298093, -4.242640687119298093 ) ) ;
#30188 = CARTESIAN_POINT ( 'NONE',  ( 0.000000000000000000, -5.999999999999991118, -157.0386751345948539 ) ) ;
#30189 = CARTESIAN_POINT ( 'NONE',  ( 115.1877832217620892, 0.7662911109078588412, -1.849990392679231599 ) ) ;
#30190 = CARTESIAN_POINT ( 'NONE',  ( -4.763139720814407951, 2.749999999999946709, -154.2500000000000000 ) ) ;
#30191 = EDGE_CURVE ( 'NONE', #7007, #3410, #14498, .T. ) ;
#30192 = CARTESIAN_POINT ( 'NONE',  ( 11.52382486540523132, 1.035533905932869425, -2.500000000000024425 ) ) ;
#30193 = ORIENTED_EDGE ( 'NONE', *, *, #873, .T. ) ;
#30194 = ORIENTED_EDGE ( 'NONE', *, *, #11654, .T. ) ;
#30195 = EDGE_CURVE ( 'NONE', #12734, #11750, #23455, .T. ) ;
#30196 = CIRCLE ( 'NONE', #24300, 0.4999999999999980016 ) ;
#30197 = ORIENTED_EDGE ( 'NONE', *, *, #29940, .T. ) ;
#30198 = CARTESIAN_POINT ( 'NONE',  ( -3.175426480542816510, -5.500000000000057732, -87.87500000000000000 ) ) ;
#30199 =( BOUNDED_CURVE ( )  B_SPLINE_CURVE ( 2, ( #8217, #20234, #26954, #22373, #17943, #3304, #12883, #29413, #22220 ),
 .UNSPECIFIED., .F., .T. ) 
 B_SPLINE_CURVE_WITH_KNOTS ( ( 3, 2, 2, 2, 3 ),
 ( 0.1972222222222222987, 0.1981481481481481843, 0.1999999999999999556, 0.2018518518518518379, 0.2027777777777777235 ),
 .UNSPECIFIED. ) 
 CURVE ( )  GEOMETRIC_REPRESENTATION_ITEM ( )  RATIONAL_B_SPLINE_CURVE ( ( 0.9330127018922194093, 0.9330127018922234061, 1.000000000000000000, 0.8660254037844388186, 1.000000000000000000, 0.8660254037844388186, 1.000000000000000000, 0.9330127018922234061, 0.9330127018922194093 ) ) 
 REPRESENTATION_ITEM ( '' )  );
#30200 = CARTESIAN_POINT ( 'NONE',  ( -5.412658773652739619, 3.124999999999975131, -109.6830127018922383 ) ) ;
#30201 = CARTESIAN_POINT ( 'NONE',  ( -7.956235894060313657E-16, -9.500000000000008882, -4.414213562373099364 ) ) ;
#30202 = CARTESIAN_POINT ( 'NONE',  ( 0.7566289708993888530, -15.57043887889865985, 7.988295740404301348 ) ) ;
#30203 = CARTESIAN_POINT ( 'NONE',  ( 4.763139720814407951, -2.749999999999988454, -165.4999999999999716 ) ) ;
#30204 = CARTESIAN_POINT ( 'NONE',  ( 159.8363248654052313, 0.000000000000000000, -5.500000000000005329 ) ) ;
#30205 = EDGE_LOOP ( 'NONE', ( #23483, #10517, #19841, #26437 ) ) ;
#30206 = CARTESIAN_POINT ( 'NONE',  ( 6.000000000000000888, -1.859271017917181981E-14, -47.16367513459483263 ) ) ;
#30207 = SURFACE_STYLE_FILL_AREA ( #20853 ) ;
#30208 = CARTESIAN_POINT ( 'NONE',  ( -6.350852961085760029, -1.281975124255709124E-13, -173.6250000000000284 ) ) ;
#30209 = CARTESIAN_POINT ( 'NONE',  ( -2.775557561562891351E-14, -5.500000000000115463, -164.2500000000000000 ) ) ;
#30210 = CARTESIAN_POINT ( 'NONE',  ( 113.2499999999998437, 2.775557561562891351E-14, 2.500000000000168754 ) ) ;
#30211 = CARTESIAN_POINT ( 'NONE',  ( -6.350852961085760029, -1.281975124255709124E-13, -101.6250000000000000 ) ) ;
#30212 = CARTESIAN_POINT ( 'NONE',  ( -3.175426480542816510, -5.500000000000057732, -98.37500000000000000 ) ) ;
#30213 = LINE ( 'NONE', #9176, #7440 ) ;
#30214 = CARTESIAN_POINT ( 'NONE',  ( 160.6086002691896795, -2.071067811865468400, -4.999999999999989342 ) ) ;
#30215 = CARTESIAN_POINT ( 'NONE',  ( 0.1950273200666144402, -15.66255992321439905, 7.807776097887577649 ) ) ;
#30216 = ORIENTED_EDGE ( 'NONE', *, *, #1965, .T. ) ;
#30217 = CARTESIAN_POINT ( 'NONE',  ( 10.68750000000010658, 2.649519052838419153, 1.097466725451619718 ) ) ;
#30218 = CARTESIAN_POINT ( 'NONE',  ( 116.3124999999997158, -1.035533905932598975, 2.500000000000144773 ) ) ;
#30219 = CARTESIAN_POINT ( 'NONE',  ( -6.000000000000000888, 1.067854986875958443E-15, 7.560779664488942560E-35 ) ) ;
#30220 = CARTESIAN_POINT ( 'NONE',  ( 107.9377832217621886, -1.849990392679472073, -0.7662911109075283278 ) ) ;
#30221 = CARTESIAN_POINT ( 'NONE',  ( 157.5074251345948824, 2.278174593052074925, -5.499999999999950262 ) ) ;
#30222 = EDGE_LOOP ( 'NONE', ( #8729, #13699, #10558, #21246 ) ) ;
#30223 =( NAMED_UNIT ( * ) PLANE_ANGLE_UNIT ( ) SI_UNIT ( $, .RADIAN. ) );
#30224 = CIRCLE ( 'NONE', #12115, 1.000000000000000888 ) ;
#30225 = CARTESIAN_POINT ( 'NONE',  ( 0.000000000000000000, 0.000000000000000000, -200.0000000000000000 ) ) ;
#30226 = VERTEX_POINT ( 'NONE', #1167 ) ;
#30227 = CARTESIAN_POINT ( 'NONE',  ( -5.999999999999963585, 1.780251999655701777E-13, -79.41367513459482552 ) ) ;
#30228 = EDGE_CURVE ( 'NONE', #24536, #22842, #6555, .T. ) ;
#30229 = ORIENTED_EDGE ( 'NONE', *, *, #7994, .F. ) ;
#30230 = CARTESIAN_POINT ( 'NONE',  ( 148.8750000000000284, 0.000000000000000000, 6.000000000000005329 ) ) ;
#30231 = ORIENTED_EDGE ( 'NONE', *, *, #23781, .F. ) ;
#30232 = CARTESIAN_POINT ( 'NONE',  ( 4.763139720814407951, 2.750000000000002665, -112.7500000000000142 ) ) ;
#30233 = CARTESIAN_POINT ( 'NONE',  ( 24.06250000000015632, -1.097466725451439196, -2.649519052838419153 ) ) ;
#30234 = CARTESIAN_POINT ( 'NONE',  ( 2.775557561562891351E-14, -6.250000000000061284, -131.6830127018922667 ) ) ;
#30235 = ORIENTED_EDGE ( 'NONE', *, *, #15752, .T. ) ;
#30236 = CYLINDRICAL_SURFACE ( 'NONE', #4852, 5.500000000000000000 ) ;
#30237 = CARTESIAN_POINT ( 'NONE',  ( 5.412658773652739619, 3.124999999999988898, -169.3169872981078470 ) ) ;
#30238 = CARTESIAN_POINT ( 'NONE',  ( 3.608439182435180470, -6.249999999999997335, -177.1919872981078470 ) ) ;
#30239 = VERTEX_POINT ( 'NONE', #24376 ) ;
#30240 = CARTESIAN_POINT ( 'NONE',  ( 111.2261751345945981, 2.000000000000061728, -0.8284271247459952248 ) ) ;
#30241 = CARTESIAN_POINT ( 'NONE',  ( 138.0863248654052313, 0.000000000000000000, 5.500000000000005329 ) ) ;
#30242 = CARTESIAN_POINT ( 'NONE',  ( 125.0000000000000568, -55.00000000000000711, 7.500000000000007105 ) ) ;
#30243 = CARTESIAN_POINT ( 'NONE',  ( 158.3363248654052313, 0.000000000000000000, -5.500000000000005329 ) ) ;
#30244 = CARTESIAN_POINT ( 'NONE',  ( 112.3127832217622455, 1.849990392679411677, -0.7662911109077087390 ) ) ;
#30245 = CARTESIAN_POINT ( 'NONE',  ( -5.412658773652739619, 3.124999999999975131, -62.31698729810780435 ) ) ;
#30246 = CARTESIAN_POINT ( 'NONE',  ( -2.775557561562891351E-14, -5.500000000000115463, -53.25000000000002132 ) ) ;
#30247 = CARTESIAN_POINT ( 'NONE',  ( 0.000000000000000000, -5.999999999999991118, -111.4613248654052171 ) ) ;
#30248 = CARTESIAN_POINT ( 'NONE',  ( 6.000000000000000888, 1.743066579297358182E-13, -51.66367513459483263 ) ) ;
#30249 = CARTESIAN_POINT ( 'NONE',  ( -5.999999999999962697, 3.323446944526963891E-14, -158.9136751345947971 ) ) ;
#30250 = CARTESIAN_POINT ( 'NONE',  ( -4.763139720814407951, 2.749999999999946709, -124.2500000000000284 ) ) ;
#30251 = CARTESIAN_POINT ( 'NONE',  ( 135.0000000000000284, -7.709521259191705056, -8.196030540009623166 ) ) ;
#30252 = DIRECTION ( 'NONE',  ( -1.000000000000000000, -1.665334536937731113E-16, 1.526556658859586792E-16 ) ) ;
#30253 = ORIENTED_EDGE ( 'NONE', *, *, #13614, .F. ) ;
#30254 = PRESENTATION_LAYER_ASSIGNMENT (  '', '', ( #8174 ) ) ;
#30255 = CARTESIAN_POINT ( 'NONE',  ( 22.43750000000002842, 1.097466725451559322, -2.649519052838298805 ) ) ;
#30256 = EDGE_CURVE ( 'NONE', #4026, #15395, #6097, .T. ) ;
#30257 = DIRECTION ( 'NONE',  ( -0.000000000000000000, -0.000000000000000000, -1.000000000000000000 ) ) ;
#30258 = DIRECTION ( 'NONE',  ( -7.147005652999508048E-36, 5.642372883946980038E-36, 1.000000000000000000 ) ) ;
#30259 = MECHANICAL_DESIGN_GEOMETRIC_PRESENTATION_REPRESENTATION (  '', ( #25329 ), #9658 ) ;
#30260 = ORIENTED_EDGE ( 'NONE', *, *, #13890, .T. ) ;
#30261 = CARTESIAN_POINT ( 'NONE',  ( 111.1247167782376124, -1.849990392679579099, 1.110223024625156540E-13 ) ) ;
#30262 = DIRECTION ( 'NONE',  ( -7.147005652999508048E-36, 5.642372883946980038E-36, 1.000000000000000000 ) ) ;
#30263 = CARTESIAN_POINT ( 'NONE',  ( -3.608439182435115633, 6.249999999999965361, -110.4419872981078186 ) ) ;
#30264 = CARTESIAN_POINT ( 'NONE',  ( 22.14882486540523132, -2.499999999999964473, 1.035533905932749299 ) ) ;
#30265 = EDGE_CURVE ( 'NONE', #3730, #24742, #30154, .T. ) ;
#30266 = CARTESIAN_POINT ( 'NONE',  ( 110.3363248654051318, -1.414213562373201061, -1.414213562373034527 ) ) ;
#30267 =( GEOMETRIC_REPRESENTATION_CONTEXT ( 3 ) GLOBAL_UNCERTAINTY_ASSIGNED_CONTEXT ( ( #10708 ) ) GLOBAL_UNIT_ASSIGNED_CONTEXT ( ( #20839, #13963, #25416 ) ) REPRESENTATION_CONTEXT ( 'NONE', 'WORKASPACE' ) );
#30268 = VERTEX_POINT ( 'NONE', #19773 ) ;
#30269 = ORIENTED_EDGE ( 'NONE', *, *, #1141, .T. ) ;
#30270 = DIRECTION ( 'NONE',  ( -0.000000000000000000, -0.000000000000000000, -1.000000000000000000 ) ) ;
#30271 = CARTESIAN_POINT ( 'NONE',  ( 133.8750000000000284, 0.000000000000000000, 6.000000000000005329 ) ) ;
#30272 = ORIENTED_EDGE ( 'NONE', *, *, #28171, .F. ) ;
#30273 = CARTESIAN_POINT ( 'NONE',  ( 3.608439182435180470, -6.249999999999997335, -136.6919872981078470 ) ) ;
#30274 = B_SPLINE_CURVE_WITH_KNOTS ( 'NONE', 3,
 ( #20787, #22476, #8322, #13138, #10823, #28418, #9407, #2484, #26127, #16507, #18640, #25833, #2344, #27813, #4482, #13906, #12201, #30134, #16656, #16207, #4626, #25678, #23544, #11904, #21237, #14059, #16806, #7248, #23248, #4783 ),
 .UNSPECIFIED., .F., .F.,
 ( 4, 2, 2, 2, 2, 2, 2, 2, 2, 2, 2, 2, 2, 2, 4 ),
 ( 0.0006116782145977108518, 0.001065641339918334783, 0.001519604465238958823, 0.001973567590559582429, 0.002427530715880206469, 0.003335456966521454115, 0.003789420091842078155, 0.004243383217162701761, 0.004697346342483326234, 0.005151309467803949840, 0.006059235718445197920, 0.006513198843765822393, 0.006967161969086445999, 0.007421125094407070473, 0.007875088219727693212 ),
 .UNSPECIFIED. ) ;
#30275 = AXIS2_PLACEMENT_3D ( 'NONE', #28407, #16647, #25970 ) ;
#30276 = CARTESIAN_POINT ( 'NONE',  ( 10.81250000000010125, -2.649519052838178457, 1.097466725451499370 ) ) ;
#30277 = FILL_AREA_STYLE ('',( #14048 ) ) ;
#30278 = VECTOR ( 'NONE', #28016, 1000.000000000000000 ) ;
#30279 = CARTESIAN_POINT ( 'NONE',  ( 24.75000000000010658, 1.665334536937734811E-13, -2.000000000000001776 ) ) ;
#30280 = DIRECTION ( 'NONE',  ( -0.7371541402007405486, -3.751025204431188723E-17, 0.6757246285173472700 ) ) ;
#30281 = LINE ( 'NONE', #14, #10819 ) ;
#30282 = CARTESIAN_POINT ( 'NONE',  ( 5.412658773652739619, 3.124999999999988898, -66.68301270189225249 ) ) ;
#30283 = CARTESIAN_POINT ( 'NONE',  ( 143.9851497308104058, -3.535533905932725318, 3.535533905932725318 ) ) ;
#30284 = CARTESIAN_POINT ( 'NONE',  ( 104.7401757384974417, 1.849990392679521589, 1.011113220803300925E-30 ) ) ;
#30285 = FACE_OUTER_BOUND ( 'NONE', #17489, .T. ) ;
#30286 = LINE ( 'NONE', #28866, #15380 ) ;
#30287 = CARTESIAN_POINT ( 'NONE',  ( 124.9999999999999432, -71.00000000000001421, -5.000000000000004441 ) ) ;
#30288 = CARTESIAN_POINT ( 'NONE',  ( 16.60117513459497118, -1.035533905932689347, 2.499999999999904521 ) ) ;
#30289 = CARTESIAN_POINT ( 'NONE',  ( 111.0624999999998295, 2.500000000000054623, 1.035533905932929599 ) ) ;
#30290 = CARTESIAN_POINT ( 'NONE',  ( 0.000000000000000000, 5.499999999999991118, -124.5000000000000568 ) ) ;
#30291 = CARTESIAN_POINT ( 'NONE',  ( 15.96132486540519047, 1.665334536937734811E-13, 2.500000000000057732 ) ) ;
#30292 = CARTESIAN_POINT ( 'NONE',  ( 0.000000000000000000, 5.999999999999977796, -148.7886751345948255 ) ) ;
#30293 = ORIENTED_EDGE ( 'NONE', *, *, #16267, .F. ) ;
#30294 = EDGE_CURVE ( 'NONE', #16705, #4423, #17646, .T. ) ;
#30295 = CARTESIAN_POINT ( 'NONE',  ( 0.000000000000000000, 5.499999999999991118, -58.50000000000000000 ) ) ;
#30296 = CARTESIAN_POINT ( 'NONE',  ( -5.196152422706601826, 2.999999999999975131, -120.9613248654052313 ) ) ;
#30297 =( BOUNDED_CURVE ( )  B_SPLINE_CURVE ( 2, ( #16788, #310, #13893, #4766, #9698, #14193, #19081, #28403, #7381 ),
 .UNSPECIFIED., .F., .T. ) 
 B_SPLINE_CURVE_WITH_KNOTS ( ( 3, 2, 2, 2, 3 ),
 ( 0.2972222222222222210, 0.2981481481481481621, 0.2999999999999999889, 0.3018518518518518712, 0.3027777777777777568 ),
 .UNSPECIFIED. ) 
 CURVE ( )  GEOMETRIC_REPRESENTATION_ITEM ( )  RATIONAL_B_SPLINE_CURVE ( ( 0.9330127018922194093, 0.9330127018922194093, 1.000000000000000000, 0.8660254037844388186, 1.000000000000000000, 0.8660254037844388186, 1.000000000000000000, 0.9330127018922214077, 0.9330127018922194093 ) ) 
 REPRESENTATION_ITEM ( '' )  );
#30298 = EDGE_LOOP ( 'NONE', ( #2350, #29767, #24106 ) ) ;
#30299 = CARTESIAN_POINT ( 'NONE',  ( 105.9374999999997584, 2.500000000000144773, -1.035533905932568777 ) ) ;
#30300 = COLOUR_RGB ( '', 0.08235294, 0.09019608, 0.10196078) ;
#30301 = CARTESIAN_POINT ( 'NONE',  ( 137.4375000000000568, -4.242640687119298093, -4.242640687119298093 ) ) ;
#30302 = CARTESIAN_POINT ( 'NONE',  ( 159.9864233307189352, -11.54654450223875095, -3.293895598147179360 ) ) ;
#30303 = CARTESIAN_POINT ( 'NONE',  ( 2.775557561562891351E-14, -6.250000000000061284, -103.8169872981078470 ) ) ;
#30304 = CARTESIAN_POINT ( 'NONE',  ( 20.03867513459486815, 1.665334536937734811E-13, -2.500000000000057732 ) ) ;
#30305 = AXIS2_PLACEMENT_3D ( 'NONE', #18930, #28251, #7227 ) ;
#30306 = EDGE_CURVE ( 'NONE', #2399, #341, #8234, .T. ) ;
#30307 = ADVANCED_FACE ( 'NONE', ( #12902 ), #26663, .T. ) ;
#30308 = CARTESIAN_POINT ( 'NONE',  ( 21.53867513459484329, 0.000000000000000000, 2.500000000000002220 ) ) ;
#30309 = CARTESIAN_POINT ( 'NONE',  ( 3.175426480543072749, 5.499999999999865885, -138.1250000000000284 ) ) ;
#30310 = ORIENTED_EDGE ( 'NONE', *, *, #26836, .T. ) ;
#30311 = PRESENTATION_LAYER_ASSIGNMENT (  '', '', ( #392 ) ) ;
#30312 = CARTESIAN_POINT ( 'NONE',  ( 14.43750000000014033, -1.999999999999851674, 0.8284271247462955401 ) ) ;
#30313 = ORIENTED_EDGE ( 'NONE', *, *, #3123, .T. ) ;
#30314 = CARTESIAN_POINT ( 'NONE',  ( 3.175426480543072749, 5.499999999999865885, -69.12500000000002842 ) ) ;
#30315 = CARTESIAN_POINT ( 'NONE',  ( 6.000000000000000888, -3.330669073875464691E-16, -7.560779664488942560E-35 ) ) ;
#30316 = CARTESIAN_POINT ( 'NONE',  ( -5.196152422706573404, -3.000000000000002665, -124.2886751345948539 ) ) ;
#30317 = CARTESIAN_POINT ( 'NONE',  ( 2.775557561562891351E-14, -6.250000000000061284, -88.18301270189220986 ) ) ;
#30318 = CARTESIAN_POINT ( 'NONE',  ( 154.6949251345948255, 5.500000000000012434, -2.278174593052012309 ) ) ;
#30319 = CARTESIAN_POINT ( 'NONE',  ( 104.6247167782375271, 1.849990392679523588, 0.000000000000000000 ) ) ;
#30320 = CARTESIAN_POINT ( 'NONE',  ( -5.999999999999965361, 1.068766945199469465, -179.9582070906448052 ) ) ;
#30321 = CARTESIAN_POINT ( 'NONE',  ( 117.5627832217621460, 0.7662911109078588412, 1.849990392679772278 ) ) ;
#30322 = CARTESIAN_POINT ( 'NONE',  ( 3.175426480543072749, -5.500000000000105693, -149.1250000000000284 ) ) ;
#30323 = LINE ( 'NONE', #4208, #3015 ) ;
#30324 = CARTESIAN_POINT ( 'NONE',  ( 4.763139720814407951, 2.750000000000002665, -135.2500000000000284 ) ) ;
#30325 = CARTESIAN_POINT ( 'NONE',  ( 7.216878364870455975, -6.409875621278545621E-14, -162.8080127018922667 ) ) ;
#30326 = CARTESIAN_POINT ( 'NONE',  ( -2.910268709469100014E-14, -10.99999999999998224, -14.99152654425661702 ) ) ;
#30327 = EDGE_CURVE ( 'NONE', #3967, #17636, #24220, .T. ) ;
#30328 = CARTESIAN_POINT ( 'NONE',  ( 3.175426480543072749, 5.499999999999865885, -79.62500000000002842 ) ) ;
#30329 = CARTESIAN_POINT ( 'NONE',  ( 5.196152422706629359, -2.999999999999988898, -140.2886751345948539 ) ) ;
#30330 = CARTESIAN_POINT ( 'NONE',  ( 116.0000000000000142, 0.000000000000000000, 0.000000000000000000 ) ) ;
#30331 = CARTESIAN_POINT ( 'NONE',  ( 3.175426480543072749, -5.500000000000105693, -63.62500000000001421 ) ) ;
#30332 = CARTESIAN_POINT ( 'NONE',  ( 150.4836002691896795, 4.999999999999989342, -2.071067811865468400 ) ) ;
#30333 = CARTESIAN_POINT ( 'NONE',  ( 6.000000000000052403, -1.607695154586662678, -87.73066243270261566 ) ) ;
#30334 = DIRECTION ( 'NONE',  ( 0.000000000000000000, 0.000000000000000000, 1.000000000000000000 ) ) ;
#30335 = CARTESIAN_POINT ( 'NONE',  ( 158.3437500000001137, -6.000000000000005329, -2.485281374238556218 ) ) ;
#30336 =( NAMED_UNIT ( * ) PLANE_ANGLE_UNIT ( ) SI_UNIT ( $, .RADIAN. ) );
#30337 = CARTESIAN_POINT ( 'NONE',  ( 20.31250000000012079, -0.8284271247461152399, 2.000000000000031530 ) ) ;
#30338 = DIRECTION ( 'NONE',  ( 5.551115123125785167E-17, -1.000000000000000000, -8.881784197001256268E-16 ) ) ;
#30339 = CARTESIAN_POINT ( 'NONE',  ( -5.196152422706573404, -3.000000000000002665, -98.78867513459482552 ) ) ;
#30340 = CARTESIAN_POINT ( 'NONE',  ( 117.8122167782374135, 0.7662911109077388261, 1.849990392679832230 ) ) ;
#30341 = ADVANCED_FACE ( 'NONE', ( #8555 ), #15972, .F. ) ;
#30342 = ORIENTED_EDGE ( 'NONE', *, *, #11945, .F. ) ;
#30343 = CARTESIAN_POINT ( 'NONE',  ( 150.5625000000000568, -4.242640687119298093, 4.242640687119298093 ) ) ;
#30344 = CARTESIAN_POINT ( 'NONE',  ( 14.83632486540520290, 1.767766952966376426, 1.767766952966376426 ) ) ;
#30345 = CARTESIAN_POINT ( 'NONE',  ( 113.2502832217622455, 1.308140751793612777, -1.308140751793640533 ) ) ;
#30346 = CARTESIAN_POINT ( 'NONE',  ( 3.464101615137757051, -5.999999999999979572, -84.91367513459481131 ) ) ;
#30347 = VERTEX_POINT ( 'NONE', #25431 ) ;
#30348 = ORIENTED_EDGE ( 'NONE', *, *, #29300, .T. ) ;
#30349 = ORIENTED_EDGE ( 'NONE', *, *, #21507, .T. ) ;
#30350 = CARTESIAN_POINT ( 'NONE',  ( -3.175426480542816510, -5.500000000000057732, -89.37500000000001421 ) ) ;
#30351 = CARTESIAN_POINT ( 'NONE',  ( -3.608439182435052128, -6.250000000000110134, -104.8080127018922383 ) ) ;
#30352 = ORIENTED_EDGE ( 'NONE', *, *, #30265, .F. ) ;
#30353 = SURFACE_SIDE_STYLE ('',( #10039 ) ) ;
#30354 = CARTESIAN_POINT ( 'NONE',  ( 155.3288997308104342, 4.999999999999989342, -2.071067811865468400 ) ) ;
#30355 = CARTESIAN_POINT ( 'NONE',  ( 159.7425748654052313, -2.278174593052159302, -5.499999999999864997 ) ) ;
#30356 = VERTEX_POINT ( 'NONE', #18562 ) ;
#30357 = CARTESIAN_POINT ( 'NONE',  ( -5.999999999999963585, -1.487416814333745711E-14, -92.91367513459482552 ) ) ;
#30358 = CARTESIAN_POINT ( 'NONE',  ( 3.175426480543072749, 5.499999999999865885, -174.1250000000000284 ) ) ;
#30359 = CARTESIAN_POINT ( 'NONE',  ( 23.47617513459499250, 1.035533905932809473, 2.499999999999904521 ) ) ;
#30360 = CARTESIAN_POINT ( 'NONE',  ( -4.763139720814407951, -2.750000000000016431, -152.5000000000000284 ) ) ;
#30361 = CARTESIAN_POINT ( 'NONE',  ( 111.4374999999997300, -2.499999999999904521, 1.035533905932869425 ) ) ;
#30362 = EDGE_CURVE ( 'NONE', #8862, #2367, #2068, .T. ) ;
#30363 = CARTESIAN_POINT ( 'NONE',  ( 4.763139720814407951, -2.749999999999988454, -102.5000000000000284 ) ) ;
#30364 = CARTESIAN_POINT ( 'NONE',  ( 0.000000000000000000, 0.000000000000000000, 0.000000000000000000 ) ) ;
#30365 = ADVANCED_FACE ( 'NONE', ( #13664 ), #1949, .T. ) ;
#30366 = CARTESIAN_POINT ( 'NONE',  ( 6.350852961086080661, -9.614813431917819062E-14, -94.87500000000004263 ) ) ;
#30367 = CARTESIAN_POINT ( 'NONE',  ( 162.2961002691896510, 2.071067811865468400, -4.999999999999989342 ) ) ;
#30368 = CARTESIAN_POINT ( 'NONE',  ( 0.8631338372297875372, -15.37878787878789133, 8.351220472436782671 ) ) ;
#30369 = VERTEX_POINT ( 'NONE', #30049 ) ;
#30370 = CARTESIAN_POINT ( 'NONE',  ( 11.18750000000003908, -2.649519052838238409, -1.097466725451559322 ) ) ;
#30371 = CARTESIAN_POINT ( 'NONE',  ( 115.0624999999998153, 2.499999999999994671, 1.035533905932929599 ) ) ;
#30372 = CARTESIAN_POINT ( 'NONE',  ( -3.464101615137725076, 5.999999999999979572, -130.0863248654052029 ) ) ;
#30373 = CARTESIAN_POINT ( 'NONE',  ( 107.5002832217622881, 1.308140751793585022, 1.308140751793751555 ) ) ;
#30374 = DIRECTION ( 'NONE',  ( -7.147005652999508048E-36, 5.642372883946980038E-36, 1.000000000000000000 ) ) ;
#30375 = ORIENTED_EDGE ( 'NONE', *, *, #13663, .F. ) ;
#30376 = DIRECTION ( 'NONE',  ( -7.147005652999508048E-36, 5.642372883946980038E-36, 1.000000000000000000 ) ) ;
#30377 = DIRECTION ( 'NONE',  ( 0.000000000000000000, -1.000000000000000000, 0.000000000000000000 ) ) ;
#30378 = CARTESIAN_POINT ( 'NONE',  ( 106.6872167782374277, 1.849990392679562001, 0.7662911109079489913 ) ) ;
#30379 = EDGE_LOOP ( 'NONE', ( #22578, #15101, #8594, #21148 ) ) ;
#30380 = DIRECTION ( 'NONE',  ( 1.000000000000000000, -5.551115123125774074E-17, 0.000000000000000000 ) ) ;
#30381 =( BOUNDED_CURVE ( )  B_SPLINE_CURVE ( 2, ( #22374, #26955, #5757, #28955, #28803, #24207, #17332, #10725, #1002 ),
 .UNSPECIFIED., .F., .T. ) 
 B_SPLINE_CURVE_WITH_KNOTS ( ( 3, 2, 2, 2, 3 ),
 ( 0.7583333333333333037, 0.7592592592592593004, 0.7611111111111110716, 0.7629629629629629539, 0.7638888888888889506 ),
 .UNSPECIFIED. ) 
 CURVE ( )  GEOMETRIC_REPRESENTATION_ITEM ( )  RATIONAL_B_SPLINE_CURVE ( ( 0.9330127018922194093, 0.9330127018922154125, 1.000000000000000000, 0.8660254037844388186, 1.000000000000000000, 0.8660254037844388186, 1.000000000000000000, 0.9330127018922154125, 0.9330127018922194093 ) ) 
 REPRESENTATION_ITEM ( '' )  );
#30382 = VERTEX_POINT ( 'NONE', #18410 ) ;
#30383 = CARTESIAN_POINT ( 'NONE',  ( 150.2812500000000284, 2.485281374238585972, 6.000000000000005329 ) ) ;
#30384 = ORIENTED_EDGE ( 'NONE', *, *, #16101, .T. ) ;
#30385 = CARTESIAN_POINT ( 'NONE',  ( -6.350852961085760029, -1.281975124255709124E-13, -112.1249999999999858 ) ) ;
#30386 = CARTESIAN_POINT ( 'NONE',  ( 23.24999999999999289, 1.873492889144956486, -1.873492889144900975 ) ) ;
#30387 = CARTESIAN_POINT ( 'NONE',  ( -7.216878364870328078, 0.000000000000000000, -133.5580127018922667 ) ) ;
#30388 = ORIENTED_EDGE ( 'NONE', *, *, #7409, .T. ) ;
#30389 = LINE ( 'NONE', #7047, #13263 ) ;
#30390 = CONICAL_SURFACE ( 'NONE', #22059, 1000.000000000000682, 0.7853981633974479459 ) ;
#30391 = CARTESIAN_POINT ( 'NONE',  ( -3.608439182435115633, 6.249999999999965361, -170.4419872981078186 ) ) ;
#30392 = CARTESIAN_POINT ( 'NONE',  ( 107.6249999999998721, -1.767766952966376426, -1.767766952966320915 ) ) ;
#30393 = VECTOR ( 'NONE', #24639, 1000.000000000000000 ) ;
#30394 = ORIENTED_EDGE ( 'NONE', *, *, #12545, .T. ) ;
#30395 = FACE_OUTER_BOUND ( 'NONE', #24170, .T. ) ;
#30396 = DIRECTION ( 'NONE',  ( 0.000000000000000000, 0.000000000000000000, 1.000000000000000000 ) ) ;
#30397 = CARTESIAN_POINT ( 'NONE',  ( 158.2425748654052029, -2.278174593052166852, -5.499999999999857003 ) ) ;
#30398 = CARTESIAN_POINT ( 'NONE',  ( 107.6252832217623308, -2.775557561562891351E-14, 1.849990392679523588 ) ) ;
#30399 = CARTESIAN_POINT ( 'NONE',  ( -7.216878364870328078, 0.000000000000000000, -175.5580127018922667 ) ) ;
#30400 = CARTESIAN_POINT ( 'NONE',  ( -0.5000000000000009992, -10.00000000000000888, -5.000000000000004441 ) ) ;
#30401 = DIRECTION ( 'NONE',  ( -0.000000000000000000, -0.000000000000000000, -1.000000000000000000 ) ) ;
#30402 = EDGE_CURVE ( 'NONE', #4728, #20271, #13509, .T. ) ;
#30403 = CARTESIAN_POINT ( 'NONE',  ( -2.775557561562891351E-14, -5.500000000000115463, -123.7500000000000284 ) ) ;
#30404 = CARTESIAN_POINT ( 'NONE',  ( 135.0000000000000284, -7.311326655561703802, -8.296327616267555882 ) ) ;
#30405 = CARTESIAN_POINT ( 'NONE',  ( 5.196152422706629359, 3.000000000000002665, -146.0386751345948539 ) ) ;
#30406 = ORIENTED_EDGE ( 'NONE', *, *, #16980, .T. ) ;
#30407 = CARTESIAN_POINT ( 'NONE',  ( 21.31250000000010658, -1.097466725451379244, -2.649519052838358757 ) ) ;
#30408 = CARTESIAN_POINT ( 'NONE',  ( 6.000000000000000888, -1.859271017917181981E-14, -72.08632486540521711 ) ) ;
#30409 = CIRCLE ( 'NONE', #13280, 0.5000000000000004441 ) ;
#30410 = FACE_OUTER_BOUND ( 'NONE', #10924, .T. ) ;
#30411 = CYLINDRICAL_SURFACE ( 'NONE', #27043, 6.000000000000000888 ) ;
#30412 = VERTEX_POINT ( 'NONE', #22549 ) ;
#30413 = CARTESIAN_POINT ( 'NONE',  ( 109.9372167782373424, -0.7662911109076785410, 1.849990392679712103 ) ) ;
#30414 = CARTESIAN_POINT ( 'NONE',  ( 6.000000000000000888, -1.859271017917181981E-14, -135.0863248654052029 ) ) ;
#30415 = CARTESIAN_POINT ( 'NONE',  ( 6.000000000000000888, -1.859271017917181981E-14, -159.0863248654052029 ) ) ;
#30416 = NEXT_ASSEMBLY_USAGE_OCCURRENCE ( 'NAUO1', ' ', ' ', #22683, #20816, $ ) ;
#30417 = NEXT_ASSEMBLY_USAGE_OCCURRENCE ( 'NAUO2', ' ', ' ', #22683, #6719, $ ) ;
#30418 = NEXT_ASSEMBLY_USAGE_OCCURRENCE ( 'NAUO3', ' ', ' ', #22683, #29032, $ ) ;
#30419 = NEXT_ASSEMBLY_USAGE_OCCURRENCE ( 'NAUO4', ' ', ' ', #22683, #10482, $ ) ;
#30420 = NEXT_ASSEMBLY_USAGE_OCCURRENCE ( 'NAUO5', ' ', ' ', #22683, #21369, $ ) ;
ENDSEC;
END-ISO-10303-21;
